#51149 = EDGE_CURVE ( 'NONE', #33316, #12604, #86124, .T. ) ;
#51148 = DIRECTION ( 'NONE',  ( -1.000000000000000000, 2.464095846557964090E-17, -0.000000000000000000 ) ) ;
#51150 =( REPRESENTATION_RELATIONSHIP ('NONE','NONE', #96270, #91803 ) REPRESENTATION_RELATIONSHIP_WITH_TRANSFORMATION ( #78954 )SHAPE_REPRESENTATION_RELATIONSHIP( ) );
#51151 = CARTESIAN_POINT ( 'NONE',  ( -63.52287095715006160, -23.47596703998600631, 11.44779298504228926 ) ) ;
#51153 = ORIENTED_EDGE ( 'NONE', *, *, #74616, .F. ) ;
#51152 = ADVANCED_FACE ( 'NONE', ( #62302 ), #48075, .T. ) ;
#51154 = CARTESIAN_POINT ( 'NONE',  ( 5.872047395031165351, -6.376774720514415407, 20.29192741308114734 ) ) ;
#51155 = EDGE_CURVE ( 'NONE', #53334, #80380, #70912, .T. ) ;
#51156 = CARTESIAN_POINT ( 'NONE',  ( -14.90462150274475306, 17.49973755783957685, 11.49999999999999645 ) ) ;
#51157 = CARTESIAN_POINT ( 'NONE',  ( -22.19569011343799048, 5.130922947863589378, 11.49999999999998934 ) ) ;
#51158 = CARTESIAN_POINT ( 'NONE',  ( -70.35039385224574460, -25.30458797330573972, 4.853613872476585378 ) ) ;
#51159 = EDGE_CURVE ( 'NONE', #89315, #78100, #93226, .T. ) ;
#51160 = CARTESIAN_POINT ( 'NONE',  ( -93.62287095715005592, -23.47593901973091235, -1.443836447539002865 ) ) ;
#51161 = DIRECTION ( 'NONE',  ( 1.000000000000000000, -7.960204194457801640E-17, 0.000000000000000000 ) ) ;
#51162 = CARTESIAN_POINT ( 'NONE',  ( -50.55620429048339304, -25.00158670708909270, 2.256160236439166855 ) ) ;
#51163 = EDGE_CURVE ( 'NONE', #89486, #99675, #54687, .T. ) ;
#51164 = CARTESIAN_POINT ( 'NONE',  ( -110.5132613601996070, -24.63355581998384380, 0.9682620441943931011 ) ) ;
#51165 = CARTESIAN_POINT ( 'NONE',  ( 17.35060923807083810, -13.37414737355047656, 11.49999999999998934 ) ) ;
#51166 = CARTESIAN_POINT ( 'NONE',  ( -59.62287095715004881, -24.64965695001468404, 8.947790433994185832 ) ) ;
#51167 = VECTOR ( 'NONE', #72036, 1000.000000000000227 ) ;
#51168 = DIRECTION ( 'NONE',  ( -3.773278334453079618E-23, 0.9999999999976377785, 2.173523156925979552E-06 ) ) ;
#51169 = DIRECTION ( 'NONE',  ( -0.8264557562326038109, 6.454799914155187856E-16, -0.5630016722799275897 ) ) ;
#51170 = DIRECTION ( 'NONE',  ( 5.328431011793917330E-15, 0.000000000000000000, 1.000000000000000000 ) ) ;
#51171 = VERTEX_POINT ( 'NONE', #8998 ) ;
#51172 = CIRCLE ( 'NONE', #85206, 1.249999999999997558 ) ;
#51173 = CARTESIAN_POINT ( 'NONE',  ( 1.124825640313904973, 20.40429917142216354, -1.500000000000002220 ) ) ;
#51174 = EDGE_LOOP ( 'NONE', ( #58205, #64185, #94069, #29016, #48778 ) ) ;
#51175 = VECTOR ( 'NONE', #52242, 1000.000000000000114 ) ;
#51176 = EDGE_LOOP ( 'NONE', ( #59918, #97243, #72844, #45718 ) ) ;
#51177 = ORIENTED_EDGE ( 'NONE', *, *, #40417, .T. ) ;
#51179 = EDGE_CURVE ( 'NONE', #1598, #7141, #16106, .T. ) ;
#51178 = ORIENTED_EDGE ( 'NONE', *, *, #7281, .F. ) ;
#51180 = CARTESIAN_POINT ( 'NONE',  ( 8.428894486204411507, 21.44871590506140890, -1.500000000000002220 ) ) ;
#51181 = CARTESIAN_POINT ( 'NONE',  ( 15.08554537508440774, -5.152774720514413431, -26.79085230644761495 ) ) ;
#51182 = CARTESIAN_POINT ( 'NONE',  ( -13.58233929615340152, 14.99024694321910900, -1.500000000000002220 ) ) ;
#51183 = AXIS2_PLACEMENT_3D ( 'NONE', #54480, #13528, #73954 ) ;
#51184 = ORIENTED_EDGE ( 'NONE', *, *, #13101, .T. ) ;
#51185 = CARTESIAN_POINT ( 'NONE',  ( -97.62287095715002749, -24.51283580621364067, 0.6167428607019886933 ) ) ;
#51186 = LINE ( 'NONE', #3518, #66039 ) ;
#51188 = EDGE_CURVE ( 'NONE', #29733, #65705, #16600, .T. ) ;
#51187 = AXIS2_PLACEMENT_3D ( 'NONE', #38541, #16199, #93830 ) ;
#51189 = CARTESIAN_POINT ( 'NONE',  ( -95.50514233772729256, -24.73486907724918282, 1.287355809206966128 ) ) ;
#51190 = CARTESIAN_POINT ( 'NONE',  ( -99.62355594549717352, -24.66019654487200086, 8.947790411086115725 ) ) ;
#51192 = ORIENTED_EDGE ( 'NONE', *, *, #67886, .F. ) ;
#51191 = CARTESIAN_POINT ( 'NONE',  ( 4.555389213293416617, -20.86945110937667280, 11.49999999999999645 ) ) ;
#51193 = CARTESIAN_POINT ( 'NONE',  ( 6.826756808399247589, -5.876774720514423400, 21.36722843294932161 ) ) ;
#51194 = VERTEX_POINT ( 'NONE', #8504 ) ;
#51195 = CARTESIAN_POINT ( 'NONE',  ( 18.30470771955606679, 12.64531542519679697, -1.500000000000002220 ) ) ;
#51196 = CARTESIAN_POINT ( 'NONE',  ( -6.067718162532647064, 19.77315050736717694, -1.500000000000002220 ) ) ;
#51197 = EDGE_LOOP ( 'NONE', ( #70031, #81041, #62892, #56052, #31066, #72434, #83010, #95801 ) ) ;
#51198 = CARTESIAN_POINT ( 'NONE',  ( 2.905472630834636139, -5.876774720514415407, 19.87563926270137671 ) ) ;
#51199 = ORIENTED_EDGE ( 'NONE', *, *, #59342, .F. ) ;
#51200 = CARTESIAN_POINT ( 'NONE',  ( -81.52287095715006160, -24.65952944569304606, 1.056160979905698794 ) ) ;
#51201 = VERTEX_POINT ( 'NONE', #79003 ) ;
#51202 = B_SPLINE_CURVE_WITH_KNOTS ( 'NONE', 3,
 ( #9464, #47038, #8467, #78964 ),
 .UNSPECIFIED., .F., .F.,
 ( 4, 4 ),
 ( 1.387778780781445676E-17, 0.0001000000000000028779 ),
 .UNSPECIFIED. ) ;
#51203 = CARTESIAN_POINT ( 'NONE',  ( -2.368302597431856782, 20.80102113048726409, -1.500000000000002220 ) ) ;
#51205 = EDGE_CURVE ( 'NONE', #47480, #59988, #32843, .T. ) ;
#51204 = CARTESIAN_POINT ( 'NONE',  ( 6.492371748702247203, -20.92784845389783399, 11.49999999999999645 ) ) ;
#51206 = CARTESIAN_POINT ( 'NONE',  ( -89.58585360431281686, -24.51419770103157703, 9.386484678747175181 ) ) ;
#51207 = CARTESIAN_POINT ( 'NONE',  ( -16.74547196562220464, 15.07928529822544661, 11.49999999999998934 ) ) ;
#51208 = CARTESIAN_POINT ( 'NONE',  ( 20.71091302404612833, 3.140364381853995912, 11.49999999999998934 ) ) ;
#51209 = CARTESIAN_POINT ( 'NONE',  ( -92.55472525529691552, -23.96169478059712787, 10.65365249895717525 ) ) ;
#51210 = CARTESIAN_POINT ( 'NONE',  ( -106.5228709571500758, -23.47596703998600631, 11.44779298504228038 ) ) ;
#51211 = CARTESIAN_POINT ( 'NONE',  ( -119.5211651280569924, -23.73791477778912551, 11.05961554403169878 ) ) ;
#51212 = DIRECTION ( 'NONE',  ( 0.000000000000000000, 0.000000000000000000, 1.000000000000000000 ) ) ;
#51213 = ORIENTED_EDGE ( 'NONE', *, *, #51359, .T. ) ;
#51214 = ORIENTED_EDGE ( 'NONE', *, *, #14916, .F. ) ;
#51215 = ORIENTED_EDGE ( 'NONE', *, *, #17363, .F. ) ;
#51216 = DIRECTION ( 'NONE',  ( 3.773278334444167608E-23, -1.000000000000000000, 0.000000000000000000 ) ) ;
#51217 = CARTESIAN_POINT ( 'NONE',  ( -20.40864349294084334, -6.676163967499375573, -1.500000000000002220 ) ) ;
#51218 = ADVANCED_FACE ( 'NONE', ( #94732 ), #62814, .F. ) ;
#51219 = DIRECTION ( 'NONE',  ( -1.000000000000000000, -3.773278334444166432E-23, -8.201307841325785021E-29 ) ) ;
#51220 = EDGE_LOOP ( 'NONE', ( #7175, #96514, #28714, #93768 ) ) ;
#51221 = CARTESIAN_POINT ( 'NONE',  ( -14.90395405082875335, 14.90835605916499418, -1.500000000000002220 ) ) ;
#51222 = DIRECTION ( 'NONE',  ( 0.000000000000000000, 0.000000000000000000, -1.000000000000000000 ) ) ;
#51223 = CARTESIAN_POINT ( 'NONE',  ( 3.797776442307698286, -6.376774720514427841, 21.83974358974358410 ) ) ;
#51224 = CARTESIAN_POINT ( 'NONE',  ( -50.55077666165203709, -24.15602025860895097, 10.28564288303536856 ) ) ;
#51225 = CARTESIAN_POINT ( 'NONE',  ( 11.80640562518893866, 3.316774720514426011, -27.06722565682295567 ) ) ;
#51226 = FACE_OUTER_BOUND ( 'NONE', #53815, .T. ) ;
#51227 = CARTESIAN_POINT ( 'NONE',  ( 17.94654606563480215, 12.89224558282342947, -1.500000000000002220 ) ) ;
#51228 = CARTESIAN_POINT ( 'NONE',  ( 9.940598223437577374, -5.876774720514426953, 17.91871304725684766 ) ) ;
#51229 = EDGE_CURVE ( 'NONE', #60724, #13389, #87633, .T. ) ;
#51230 = CARTESIAN_POINT ( 'NONE',  ( -44.62287095715004881, -24.65952944569303895, 1.056160979905693686 ) ) ;
#51231 = CARTESIAN_POINT ( 'NONE',  ( -94.52287095715006160, -24.65952944569304961, 1.056160979905700570 ) ) ;
#51232 = VECTOR ( 'NONE', #83691, 1000.000000000000114 ) ;
#51233 = CARTESIAN_POINT ( 'NONE',  ( -81.88534077628074215, -29.50249666744127808, 6.293933732382250845 ) ) ;
#51234 = CARTESIAN_POINT ( 'NONE',  ( 13.34776491790984210, -16.67230741956907991, 11.49999999999998934 ) ) ;
#51235 = CARTESIAN_POINT ( 'NONE',  ( -113.5562042904834072, -23.48786465467241769, 11.44779295918254292 ) ) ;
#51236 = DIRECTION ( 'NONE',  ( -1.000000000000000000, 1.232047923278981953E-16, 0.000000000000000000 ) ) ;
#51237 = PLANE ( 'NONE',  #81075 ) ;
#51238 = FACE_OUTER_BOUND ( 'NONE', #32061, .T. ) ;
#51239 = CC_DESIGN_DATE_AND_TIME_ASSIGNMENT ( #35911, #8456, ( #2120 ) ) ;
#51240 = CARTESIAN_POINT ( 'NONE',  ( -18.78231125015805958, 12.62931641965373153, -1.500000000000002220 ) ) ;
#51241 = AXIS2_PLACEMENT_3D ( 'NONE', #46919, #54533, #33189 ) ;
#51242 = ORIENTED_EDGE ( 'NONE', *, *, #21644, .T. ) ;
#51243 = CIRCLE ( 'NONE', #10752, 252.4458649670781085 ) ;
#51244 = DIRECTION ( 'NONE',  ( -3.773278334453080206E-23, 0.9999999999976377785, 2.173523156925979975E-06 ) ) ;
#51245 = CARTESIAN_POINT ( 'NONE',  ( -79.52213164415213953, -23.48783264082476308, -1.443836473390096575 ) ) ;
#51246 = CARTESIAN_POINT ( 'NONE',  ( -19.57314199983870751, -2.777824058246878280, 11.49999999999999645 ) ) ;
#51247 = CARTESIAN_POINT ( 'NONE',  ( -4.968349358974361252, -6.376774720514411854, 19.46153846153847056 ) ) ;
#51248 = VECTOR ( 'NONE', #7055, 1000.000000000000000 ) ;
#51249 = CARTESIAN_POINT ( 'NONE',  ( -67.53678271749727458, -24.65952944569304606, 1.056160979905700570 ) ) ;
#51250 = B_SPLINE_CURVE_WITH_KNOTS ( 'NONE', 3,
 ( #6593, #53782, #68498, #92821 ),
 .UNSPECIFIED., .F., .F.,
 ( 4, 4 ),
 ( 0.000000000000000000, 1.000000000000000000 ),
 .UNSPECIFIED. ) ;
#51251 = ORIENTED_EDGE ( 'NONE', *, *, #73199, .T. ) ;
#51252 = AXIS2_PLACEMENT_3D ( 'NONE', #6179, #21387, #91910 ) ;
#51253 = CARTESIAN_POINT ( 'NONE',  ( -54.52287095715006870, -29.50248528299804818, 1.056150453629033370 ) ) ;
#51254 = CARTESIAN_POINT ( 'NONE',  ( -29.31644179857717347, -25.26026486303936025, 2.549173870068830006 ) ) ;
#51255 = LINE ( 'NONE', #34536, #82058 ) ;
#51256 = CARTESIAN_POINT ( 'NONE',  ( -16.79864850723062020, -13.61054813162024679, -1.500000000000002220 ) ) ;
#51257 = CARTESIAN_POINT ( 'NONE',  ( 31.88667425545054002, -1.477225279485574028, -9.651215965565025812 ) ) ;
#51259 = CARTESIAN_POINT ( 'NONE',  ( -11.15089393765527959, -15.82809448842462885, -1.500000000000002220 ) ) ;
#51258 = AXIS2_PLACEMENT_3D ( 'NONE', #35924, #98306, #88722 ) ;
#51260 = B_SPLINE_CURVE_WITH_KNOTS ( 'NONE', 3,
 ( #58441, #75139, #5630, #51821, #81761, #42227 ),
 .UNSPECIFIED., .F., .F.,
 ( 4, 2, 4 ),
 ( 0.000000000000000000, 0.001380764517854760412, 0.002761529035709520824 ),
 .UNSPECIFIED. ) ;
#51261 = CARTESIAN_POINT ( 'NONE',  ( -10.23311166579590825, -4.222446552888387217, 29.28685113854110966 ) ) ;
#51262 = CARTESIAN_POINT ( 'NONE',  ( 282.9764569301858046, -5.356774720514427379, 20.79159422840526616 ) ) ;
#51263 = CARTESIAN_POINT ( 'NONE',  ( -2.602694502683683631, -19.63732897141692391, 11.49999999999998934 ) ) ;
#51264 = VERTEX_POINT ( 'NONE', #42474 ) ;
#51265 = CARTESIAN_POINT ( 'NONE',  ( -3.898967980886277829, 19.90457959416237088, 11.49999999999999645 ) ) ;
#51266 = CARTESIAN_POINT ( 'NONE',  ( 6.875727764383598561, 6.376774720514445605, -25.57138887952572404 ) ) ;
#51267 = CARTESIAN_POINT ( 'NONE',  ( 6.044119082205957838, -6.376774720514424288, 21.40268112089023589 ) ) ;
#51268 = VERTEX_POINT ( 'NONE', #4893 ) ;
#51269 = CARTESIAN_POINT ( 'NONE',  ( -110.5228709571500616, -24.99132157543167310, 2.256160258750667502 ) ) ;
#51270 = CARTESIAN_POINT ( 'NONE',  ( 15.15958133180904355, -5.152774720514426754, -26.63299148310929709 ) ) ;
#51271 = CYLINDRICAL_SURFACE ( 'NONE', #80804, 2.499999999999995115 ) ;
#51272 = DIRECTION ( 'NONE',  ( 0.000000000000000000, 0.000000000000000000, -1.000000000000000000 ) ) ;
#51273 = CARTESIAN_POINT ( 'NONE',  ( 18.22465585706453339, 0.000000000000000000, -2.153101996372891236 ) ) ;
#51274 = CARTESIAN_POINT ( 'NONE',  ( -13.81204400269958654, 14.50282280199826701, -1.500000000000002220 ) ) ;
#51275 = CARTESIAN_POINT ( 'NONE',  ( 32.45853543194704116, 0.3587747205144265483, 9.169203677920338080 ) ) ;
#51276 = ORIENTED_EDGE ( 'NONE', *, *, #9825, .F. ) ;
#51277 = VECTOR ( 'NONE', #30905, 1000.000000000000000 ) ;
#51278 = DIRECTION ( 'NONE',  ( 7.150924204855701834E-40, 2.173523156925979975E-06, -0.9999999999976378895 ) ) ;
#51279 = ADVANCED_FACE ( 'NONE', ( #18604 ), #28289, .T. ) ;
#51280 = CARTESIAN_POINT ( 'NONE',  ( -129.5228709571500758, -24.64898659630529920, 1.056161002820834804 ) ) ;
#51281 = CARTESIAN_POINT ( 'NONE',  ( -3.106028565906091998, -5.876774720514426953, 3.106028565906120864 ) ) ;
#51282 = EDGE_CURVE ( 'NONE', #39531, #72799, #81522, .T. ) ;
#51283 = CARTESIAN_POINT ( 'NONE',  ( -113.5228709571500616, -24.64898659630368627, 1.056161002820831474 ) ) ;
#51284 = DIRECTION ( 'NONE',  ( -3.773278334453079618E-23, 0.9999999999976377785, 2.173523156925979975E-06 ) ) ;
#51285 = B_SPLINE_CURVE_WITH_KNOTS ( 'NONE', 3,
 ( #37975, #78896, #61828, #68429, #1796, #76518, #17512, #7024, #40355, #60833, #48479, #91751 ),
 .UNSPECIFIED., .F., .F.,
 ( 4, 2, 2, 2, 2, 4 ),
 ( 6.686686736723900881E-09, 0.0004767310751705819308, 0.0009534554636544272143, 0.001430179852138272444, 0.001668542046380201618, 0.001906904240622130792 ),
 .UNSPECIFIED. ) ;
#51286 = CARTESIAN_POINT ( 'NONE',  ( -71.52287095715010423, -24.66019654487200086, 8.947790411086115725 ) ) ;
#51287 = ORIENTED_EDGE ( 'NONE', *, *, #25140, .F. ) ;
#51288 = CARTESIAN_POINT ( 'NONE',  ( 9.809556900635294951, 17.81656380412256269, 11.49999999999998934 ) ) ;
#51289 = ORIENTED_EDGE ( 'NONE', *, *, #71711, .T. ) ;
#51290 = EDGE_CURVE ( 'NONE', #88013, #54552, #41972, .T. ) ;
#51291 = CARTESIAN_POINT ( 'NONE',  ( -3.094460115123966570, -22.75893099265358188, 11.49999999999998934 ) ) ;
#51293 = CARTESIAN_POINT ( 'NONE',  ( -32.57492585626526704, -24.65952944569304606, 1.056160979905696351 ) ) ;
#51292 = B_SPLINE_CURVE_WITH_KNOTS ( 'NONE', 3,
 ( #95921, #94918, #33523, #16791 ),
 .UNSPECIFIED., .F., .F.,
 ( 4, 4 ),
 ( 0.09985723008135170831, 0.1088636613534670478 ),
 .UNSPECIFIED. ) ;
#51294 = ORIENTED_EDGE ( 'NONE', *, *, #12249, .F. ) ;
#51295 = DIRECTION ( 'NONE',  ( 0.000000000000000000, -2.173523156925980399E-06, 0.9999999999976378895 ) ) ;
#51296 = AXIS2_PLACEMENT_3D ( 'NONE', #41157, #48775, #49280 ) ;
#51297 = CARTESIAN_POINT ( 'NONE',  ( -77.62287095715005592, -24.64965695001468404, 8.947790433994182280 ) ) ;
#51298 = LINE ( 'NONE', #82238, #54501 ) ;
#51300 = VERTEX_POINT ( 'NONE', #34347 ) ;
#51299 = CARTESIAN_POINT ( 'NONE',  ( -13.45780860896912934, -16.40347334334247265, 11.49999999999999645 ) ) ;
#51301 = VERTEX_POINT ( 'NONE', #11005 ) ;
#51302 = CARTESIAN_POINT ( 'NONE',  ( -18.12599551585701008, -12.76988789260850332, -1.500000000000002220 ) ) ;
#51303 = CARTESIAN_POINT ( 'NONE',  ( -3.210669876418242197, 20.33209092710186638, 11.49999999999998934 ) ) ;
#51304 = CIRCLE ( 'NONE', #2717, 1.249999999999996003 ) ;
#51305 = EDGE_LOOP ( 'NONE', ( #40065, #51825, #84510, #1919 ) ) ;
#51306 = ORIENTED_EDGE ( 'NONE', *, *, #69404, .F. ) ;
#51307 = CARTESIAN_POINT ( 'NONE',  ( -94.52287095715006160, -29.50248528299804818, 1.056150453629040253 ) ) ;
#51308 = PLANE ( 'NONE',  #61596 ) ;
#51309 = ORIENTED_EDGE ( 'NONE', *, *, #88162, .F. ) ;
#51310 = VECTOR ( 'NONE', #4276, 1000.000000000000114 ) ;
#51311 = ORIENTED_EDGE ( 'NONE', *, *, #78969, .F. ) ;
#51312 = CIRCLE ( 'NONE', #64311, 1.500000000000000666 ) ;
#51313 = VERTEX_POINT ( 'NONE', #72416 ) ;
#51314 = CARTESIAN_POINT ( 'NONE',  ( 0.000000000000000000, 0.000000000000000000, 0.000000000000000000 ) ) ;
#51315 = CARTESIAN_POINT ( 'NONE',  ( -28.62972572368664714, -24.36142566672730325, 9.386484685950513551 ) ) ;
#51316 = PLANE ( 'NONE',  #14705 ) ;
#51317 = CARTESIAN_POINT ( 'NONE',  ( -0.3852054317258338245, -20.75737367715079174, -1.500000000000002220 ) ) ;
#51318 = CARTESIAN_POINT ( 'NONE',  ( 18.41774212405765709, -11.57998961627671441, 11.49999999999999645 ) ) ;
#51319 = ORIENTED_EDGE ( 'NONE', *, *, #22163, .F. ) ;
#51320 = CARTESIAN_POINT ( 'NONE',  ( -40.45231480346743069, -25.27806139640134120, 5.081397595443370996 ) ) ;
#51321 = DIRECTION ( 'NONE',  ( -3.773278334453080206E-23, 0.9999999999976377785, 2.173523156925979975E-06 ) ) ;
#51322 = CARTESIAN_POINT ( 'NONE',  ( -115.5516351120022591, -24.73486907724918282, 1.287355809206964352 ) ) ;
#51323 = CARTESIAN_POINT ( 'NONE',  ( -17.72129891523481149, -13.73837202384828515, -1.500000000000002220 ) ) ;
#51324 = DIRECTION ( 'NONE',  ( -3.773278334453080206E-23, 0.9999999999976377785, 2.173523156925979975E-06 ) ) ;
#51325 = CARTESIAN_POINT ( 'NONE',  ( 23.07151214508650128, 3.625915217019311583E-15, 0.000000000000000000 ) ) ;
#51327 = EDGE_CURVE ( 'NONE', #57623, #75580, #89851, .T. ) ;
#51326 = ORIENTED_EDGE ( 'NONE', *, *, #5495, .T. ) ;
#51328 = CARTESIAN_POINT ( 'NONE',  ( -0.3059464777392852941, -8.530684776139525027, -9.000000000000000000 ) ) ;
#51329 = CARTESIAN_POINT ( 'NONE',  ( -86.52287095715006160, -23.48783264083431277, -1.443836473375255336 ) ) ;
#51330 = ORIENTED_EDGE ( 'NONE', *, *, #13785, .T. ) ;
#51331 = B_SPLINE_CURVE_WITH_KNOTS ( 'NONE', 3,
 ( #86988, #72782, #94098, #55558 ),
 .UNSPECIFIED., .F., .F.,
 ( 4, 4 ),
 ( 0.000000000000000000, 9.999999999997510880E-05 ),
 .UNSPECIFIED. ) ;
#51332 = VERTEX_POINT ( 'NONE', #26229 ) ;
#51333 = CARTESIAN_POINT ( 'NONE',  ( 25.61870917940689196, -0.3587747205144265483, 28.79814474876424768 ) ) ;
#51334 = ADVANCED_FACE ( 'NONE', ( #49083 ), #20107, .F. ) ;
#51335 = ORIENTED_EDGE ( 'NONE', *, *, #65704, .T. ) ;
#51336 = CARTESIAN_POINT ( 'NONE',  ( -20.61954105445765251, -5.431428859615135885, -1.500000000000002220 ) ) ;
#51337 = B_SPLINE_CURVE_WITH_KNOTS ( 'NONE', 3,
 ( #71069, #77653, #9665, #70055 ),
 .UNSPECIFIED., .F., .F.,
 ( 4, 4 ),
 ( 0.000000000000000000, 9.999999999996123101E-05 ),
 .UNSPECIFIED. ) ;
#51338 = ORIENTED_EDGE ( 'NONE', *, *, #94608, .T. ) ;
#51339 = CYLINDRICAL_SURFACE ( 'NONE', #36538, 24.00000000000000000 ) ;
#51340 = CARTESIAN_POINT ( 'NONE',  ( 8.107222467604051630, 20.28165043084963060, 11.49999999999998934 ) ) ;
#51341 = CARTESIAN_POINT ( 'NONE',  ( -3.826923076923078426, -6.376774720514408301, 19.19230769230769695 ) ) ;
#51342 = CARTESIAN_POINT ( 'NONE',  ( 4.020035926878589905, 22.33396232419688587, 11.49999999999998934 ) ) ;
#51343 = CARTESIAN_POINT ( 'NONE',  ( -112.5895376238167245, -24.65952944569305316, 1.056160979905713670 ) ) ;
#51344 = CARTESIAN_POINT ( 'NONE',  ( -49.52287095715004028, -23.73934037231756022, 11.05740245334329153 ) ) ;
#51345 = CARTESIAN_POINT ( 'NONE',  ( 19.17116566557315949, -10.70166234769870961, -1.500000000000002220 ) ) ;
#51346 = DIRECTION ( 'NONE',  ( 0.000000000000000000, -0.9999999999976377785, -2.173523156925979975E-06 ) ) ;
#51347 = VERTEX_POINT ( 'NONE', #58189 ) ;
#51348 = CARTESIAN_POINT ( 'NONE',  ( 29.70917971445138051, -6.219445159570049064, 27.14760184111773356 ) ) ;
#51349 = CARTESIAN_POINT ( 'NONE',  ( -84.52287095715006160, -29.50250243563736774, 8.947779886222141599 ) ) ;
#51350 = VECTOR ( 'NONE', #80516, 1000.000000000000000 ) ;
#51351 = EDGE_LOOP ( 'NONE', ( #77587, #79306, #34967, #68654, #40460, #53071, #44821, #11575, #20305, #27278, #78489, #36997, #8512, #17264, #88504, #17088, #13729, #8465, #22625, #38810, #95082, #1931, #79262, #29647, #81531, #84377, #71651, #21972, #60101, #62389, #65302, #48465, #76140, #38484, #6305, #77231, #94603, #17104, #49511, #72415, #34215, #53736, #81343, #4012, #93531, #11029, #10873, #42856, #42118, #71820, #3869, #31675, #86209, #50982, #71535, #69745, #43980, #3815, #9919, #29087, #39720, #1000, #82347, #95984, #20997, #58950, #7034, #83903, #73603, #2434, #1661, #2324, #54322, #60198, #32215, #7485, #90233, #47094, #33174, #24963, #88435, #14732, #63720, #68966, #64391, #80048, #16802, #49092, #10573, #53846, #46301, #73806, #98452, #54586, #66156, #40868, #94996, #81552, #97253, #40734, #19819 ) ) ;
#51352 = DIRECTION ( 'NONE',  ( -3.773278334453080206E-23, 0.9999999999976377785, 2.173523156925979975E-06 ) ) ;
#51353 = CARTESIAN_POINT ( 'NONE',  ( 5.097264368846952998, 6.475225279485573360, -27.56135813788808164 ) ) ;
#51354 = AXIS2_PLACEMENT_3D ( 'NONE', #60720, #70820, #29752 ) ;
#51355 = CARTESIAN_POINT ( 'NONE',  ( -0.1490770655183800975, -21.12008023607309681, -1.443836447538997314 ) ) ;
#51356 = CARTESIAN_POINT ( 'NONE',  ( -13.59518820711925358, -16.35513075224449864, 11.49999999999998934 ) ) ;
#51357 = CARTESIAN_POINT ( 'NONE',  ( -112.5905343604989923, -24.15543982623908192, -0.2315651400026420559 ) ) ;
#51358 = CARTESIAN_POINT ( 'NONE',  ( -26.21213932664330670, -24.75186287970886667, 3.737064058008186418 ) ) ;
#51359 = EDGE_CURVE ( 'NONE', #42617, #99563, #83323, .T. ) ;
#51360 = DIRECTION ( 'NONE',  ( -0.2007054744626894649, 0.000000000000000000, 0.9796516281417116945 ) ) ;
#51361 = PLANE ( 'NONE',  #57336 ) ;
#51362 = B_SPLINE_SURFACE_WITH_KNOTS ( 'NONE', 3, 3, ( 
 ( #88698, #65880, #19166, #27786 ),
 ( #58739, #95798, #50135, #43022 ),
 ( #27294, #89688, #50628, #18669 ),
 ( #82071, #12557, #80078, #73966 ),
 ( #97790, #41523, #26292, #88198 ),
 ( #33903, #81582, #4464, #77912 ),
 ( #23196, #61789, #76980, #54181 ) ),
 .UNSPECIFIED., .F., .F., .F.,
 ( 4, 3, 4 ),
 ( 4, 4 ),
 ( 0.0004766839783824310508, 0.1029713700210899002, 0.2054660560637973643 ),
 ( 0.2595600248839645130, 0.2606925099585566397 ),
 .UNSPECIFIED. ) ;
#51363 = CARTESIAN_POINT ( 'NONE',  ( -117.5188394651187167, -24.15620529776629510, 10.23563542870659582 ) ) ;
#51364 = VERTEX_POINT ( 'NONE', #2911 ) ;
#51365 = CARTESIAN_POINT ( 'NONE',  ( 19.09806219120973125, -4.162641619376711510, 11.49999999999999645 ) ) ;
#51366 = CARTESIAN_POINT ( 'NONE',  ( -66.62287095715002749, -24.35013146730203459, 9.818937971375113705 ) ) ;
#51367 = CARTESIAN_POINT ( 'NONE',  ( -29.81175120719462157, -25.24633111994858581, 4.942810988825437235 ) ) ;
#51368 = ORIENTED_EDGE ( 'NONE', *, *, #58290, .F. ) ;
#51369 = CARTESIAN_POINT ( 'NONE',  ( 4.332134589405623792, -5.876774720514426953, 21.69242924468134959 ) ) ;
#51370 = EDGE_CURVE ( 'NONE', #17140, #30450, #76905, .T. ) ;
#51371 = CARTESIAN_POINT ( 'NONE',  ( -101.5228709571500758, -24.64965694238407323, 8.947790433994194714 ) ) ;
#51372 = CIRCLE ( 'NONE', #62762, 2.249999999999998668 ) ;
#51373 = CARTESIAN_POINT ( 'NONE',  ( -27.61217026053484958, -24.64375301970309806, 8.250468979048056539 ) ) ;
#51374 = CARTESIAN_POINT ( 'NONE',  ( 6.499999999999992895, 0.9999999999999993339, 1.084202172485504187E-16 ) ) ;
#51375 = CARTESIAN_POINT ( 'NONE',  ( 16.13486940644654766, 11.28601765141728741, 11.49999999999998934 ) ) ;
#51376 = ORIENTED_EDGE ( 'NONE', *, *, #57239, .F. ) ;
#51377 = DIRECTION ( 'NONE',  ( 0.000000000000000000, 0.000000000000000000, -1.000000000000000000 ) ) ;
#51378 = CARTESIAN_POINT ( 'NONE',  ( -72.62287095715005592, -29.50247984919015209, -1.443849546365055359 ) ) ;
#51379 = AXIS2_PLACEMENT_3D ( 'NONE', #20813, #6098, #45672 ) ;
#51380 = COORDINATED_UNIVERSAL_TIME_OFFSET ( 0, 0, .AHEAD. ) ;
#51381 = ORIENTED_EDGE ( 'NONE', *, *, #55274, .F. ) ;
#51382 = CARTESIAN_POINT ( 'NONE',  ( 8.456965425111590662, -0.2003331576018148041, 3.712238059855193839 ) ) ;
#51383 = CARTESIAN_POINT ( 'NONE',  ( -45.62287095715005592, -24.92604778743018556, 8.074972756849359001 ) ) ;
#51384 = CARTESIAN_POINT ( 'NONE',  ( -55.56003731193040807, -23.85016227208578954, -0.8807180028928371929 ) ) ;
#51385 = CARTESIAN_POINT ( 'NONE',  ( -63.22287095715004313, -23.47593901973090524, -1.443836447538997536 ) ) ;
#51386 = CARTESIAN_POINT ( 'NONE',  ( -31.62287095715005236, -23.95044443724991368, 10.65354141964649948 ) ) ;
#51387 = AXIS2_PLACEMENT_3D ( 'NONE', #17513, #62707, #63718 ) ;
#51388 = AXIS2_PLACEMENT_3D ( 'NONE', #84396, #99601, #55459 ) ;
#51389 = DIRECTION ( 'NONE',  ( 0.000000000000000000, -0.9999999999976377785, -2.173523156925979975E-06 ) ) ;
#51390 = ADVANCED_FACE ( 'NONE', ( #65814 ), #88137, .F. ) ;
#51391 = CARTESIAN_POINT ( 'NONE',  ( -107.6280297884409265, -24.15543982623907837, -0.2315651400026443874 ) ) ;
#51393 = EDGE_CURVE ( 'NONE', #88212, #81441, #85350, .T. ) ;
#51392 = CARTESIAN_POINT ( 'NONE',  ( 19.82558669001425500, -2.195561414069463702, 11.49999999999998934 ) ) ;
#51394 = DIRECTION ( 'NONE',  ( -3.773278334453079618E-23, 0.9999999999976377785, 2.173523156925979975E-06 ) ) ;
#51395 = CARTESIAN_POINT ( 'NONE',  ( -0.03888317010184255684, -22.54662680705505551, 8.463919116204994708 ) ) ;
#51396 = ORIENTED_EDGE ( 'NONE', *, *, #44976, .T. ) ;
#51397 = DIRECTION ( 'NONE',  ( -3.773278334453079618E-23, 0.9999999999976377785, 2.173523156925979975E-06 ) ) ;
#51398 = DIRECTION ( 'NONE',  ( 1.000000000000000000, 0.000000000000000000, 0.000000000000000000 ) ) ;
#51399 = PLANE ( 'NONE',  #71841 ) ;
#51400 = DIRECTION ( 'NONE',  ( -0.7071067811865516806, -0.7071067811865434649, 0.000000000000000000 ) ) ;
#51401 = FACE_OUTER_BOUND ( 'NONE', #73789, .T. ) ;
#51402 = ADVANCED_FACE ( 'NONE', ( #29718 ), #100209, .T. ) ;
#51403 = CARTESIAN_POINT ( 'NONE',  ( -2.070328576748420524, -6.376774720514410077, 19.46575348430201657 ) ) ;
#51404 = B_SPLINE_CURVE_WITH_KNOTS ( 'NONE', 3,
 ( #19637, #13516, #5418, #67329 ),
 .UNSPECIFIED., .F., .F.,
 ( 4, 4 ),
 ( 0.000000000000000000, 1.000000000000000000 ),
 .UNSPECIFIED. ) ;
#51405 = ORIENTED_EDGE ( 'NONE', *, *, #49017, .F. ) ;
#51406 = CARTESIAN_POINT ( 'NONE',  ( -97.52287095715007581, -23.47593901973090524, -1.443836447538996648 ) ) ;
#51407 = EDGE_CURVE ( 'NONE', #75293, #99976, #14982, .T. ) ;
#51408 = CARTESIAN_POINT ( 'NONE',  ( 6.274899854645557440, -5.876774720514428729, 21.83451738260096775 ) ) ;
#51409 = ORIENTED_EDGE ( 'NONE', *, *, #20418, .F. ) ;
#51410 = CARTESIAN_POINT ( 'NONE',  ( 3.706880958665978998, 19.89330832657401515, -1.500000000000002220 ) ) ;
#51411 = B_SPLINE_CURVE_WITH_KNOTS ( 'NONE', 3,
 ( #8285, #95024, #86908, #9786 ),
 .UNSPECIFIED., .F., .F.,
 ( 4, 4 ),
 ( 2.775557561562891351E-17, 8.203124999998923084E-05 ),
 .UNSPECIFIED. ) ;
#51412 = DIRECTION ( 'NONE',  ( -0.1478094111296165691, 0.9890158633619158257, 6.377659838150018832E-17 ) ) ;
#51413 = EDGE_CURVE ( 'NONE', #7766, #68548, #92545, .T. ) ;
#51414 = CARTESIAN_POINT ( 'NONE',  ( 15.03086228770605004, 5.128928118853486318, -26.95277610321158335 ) ) ;
#51415 = AXIS2_PLACEMENT_3D ( 'NONE', #47344, #1674, #47845 ) ;
#51416 = ADVANCED_FACE ( 'NONE', ( #28728 ), #76374, .F. ) ;
#51417 = CARTESIAN_POINT ( 'NONE',  ( -58.52287095715004739, -23.47593901973090169, -1.443836447538997092 ) ) ;
#51418 = ORIENTED_EDGE ( 'NONE', *, *, #62512, .F. ) ;
#51419 = CARTESIAN_POINT ( 'NONE',  ( -105.9228709571500673, -23.47596703998600631, 11.44779298504227860 ) ) ;
#51420 = FACE_OUTER_BOUND ( 'NONE', #64052, .T. ) ;
#51421 = CARTESIAN_POINT ( 'NONE',  ( 20.03642891561555928, 0.6179553080306146029, -1.500000000000002220 ) ) ;
#51422 = CARTESIAN_POINT ( 'NONE',  ( 19.54352652498339182, 7.673529024697476331, 11.49999999999999645 ) ) ;
#51423 = CIRCLE ( 'NONE', #7666, 1.700000000000008837 ) ;
#51424 = CARTESIAN_POINT ( 'NONE',  ( -28.94471403569382773, -25.05935760451456318, 6.779848816579228554 ) ) ;
#51425 = CARTESIAN_POINT ( 'NONE',  ( -111.6228709571500417, -24.50321055353806088, 9.387540953477531147 ) ) ;
#51426 = CARTESIAN_POINT ( 'NONE',  ( -21.42919730060085115, -5.301375089729956969, 11.49999999999998934 ) ) ;
#51427 = B_SPLINE_CURVE_WITH_KNOTS ( 'NONE', 3,
 ( #45543, #24185, #77461, #7961 ),
 .UNSPECIFIED., .F., .F.,
 ( 4, 4 ),
 ( 0.000000000000000000, 9.999999999998897304E-05 ),
 .UNSPECIFIED. ) ;
#51428 = CARTESIAN_POINT ( 'NONE',  ( -66.55620429048339304, -24.66019654487199020, 8.947790411086131712 ) ) ;
#51429 = CARTESIAN_POINT ( 'NONE',  ( -47.62287095715004881, -24.64898659630367916, 1.056161002820821038 ) ) ;
#51430 = CARTESIAN_POINT ( 'NONE',  ( -50.30027857337484676, -25.27344760046473482, 3.296100333510875391 ) ) ;
#51431 = ORIENTED_EDGE ( 'NONE', *, *, #55153, .T. ) ;
#51432 = LINE ( 'NONE', #21945, #5685 ) ;
#51433 = CARTESIAN_POINT ( 'NONE',  ( -31.56131489220916819, -23.73766607897669800, -1.055555164236445131 ) ) ;
#51434 = ORIENTED_EDGE ( 'NONE', *, *, #28038, .T. ) ;
#51435 = ORIENTED_EDGE ( 'NONE', *, *, #97339, .F. ) ;
#51436 = CARTESIAN_POINT ( 'NONE',  ( 16.26279755680690542, -1.684774720514426560, -27.67997040356620531 ) ) ;
#51437 = FACE_OUTER_BOUND ( 'NONE', #16117, .T. ) ;
#51438 = CARTESIAN_POINT ( 'NONE',  ( -76.55419634045316002, -23.96119346886880663, -0.6495511937832058047 ) ) ;
#51439 = CARTESIAN_POINT ( 'NONE',  ( -16.28974412851428255, -12.55652860423730388, -1.500000000000002220 ) ) ;
#51440 = CARTESIAN_POINT ( 'NONE',  ( -19.30636564405121902, 9.640216152154000184, 11.49999999999999645 ) ) ;
#51441 = ORIENTED_EDGE ( 'NONE', *, *, #6831, .F. ) ;
#51442 = CARTESIAN_POINT ( 'NONE',  ( -50.26609345566524922, -25.13378748658239559, 7.097951806649573037 ) ) ;
#51443 = CARTESIAN_POINT ( 'NONE',  ( -99.12672354517025042, -25.27198829872966712, 4.094481813589349706 ) ) ;
#51444 = PLANE ( 'NONE',  #22110 ) ;
#51445 = CARTESIAN_POINT ( 'NONE',  ( 4.697571063781373013, 21.84268702631108994, 11.49999999999998934 ) ) ;
#51446 = VECTOR ( 'NONE', #91788, 1000.000000000000114 ) ;
#51447 = CARTESIAN_POINT ( 'NONE',  ( -50.62287095715004170, -23.48783264082478084, -1.443836473390070596 ) ) ;
#51448 = CARTESIAN_POINT ( 'NONE',  ( -20.77875734969026311, 6.143225279485574397, 27.35402280011862430 ) ) ;
#51449 = ORIENTED_EDGE ( 'NONE', *, *, #11070, .T. ) ;
#51450 = DIRECTION ( 'NONE',  ( -0.1593164160933057683, 0.000000000000000000, 0.9872275723272647685 ) ) ;
#51451 = LINE ( 'NONE', #35229, #96093 ) ;
#51452 = CARTESIAN_POINT ( 'NONE',  ( 17.92008016455634589, 10.74458801173053324, 11.49999999999998934 ) ) ;
#51453 = ORIENTED_EDGE ( 'NONE', *, *, #29385, .T. ) ;
#51455 = ORIENTED_EDGE ( 'NONE', *, *, #91076, .T. ) ;
#51454 = FACE_OUTER_BOUND ( 'NONE', #35363, .T. ) ;
#51456 = CIRCLE ( 'NONE', #48202, 4.299999999999999822 ) ;
#51457 = ORIENTED_EDGE ( 'NONE', *, *, #90424, .T. ) ;
#51458 = EDGE_CURVE ( 'NONE', #32849, #33122, #80153, .T. ) ;
#51459 = CARTESIAN_POINT ( 'NONE',  ( -100.5576076336107434, -23.85049219812686161, 10.88485053497527133 ) ) ;
#51460 = CARTESIAN_POINT ( 'NONE',  ( -3.482456173223098528, 20.84670800329844198, -1.500000000000002220 ) ) ;
#51461 = ORIENTED_EDGE ( 'NONE', *, *, #79934, .F. ) ;
#51462 = DIRECTION ( 'NONE',  ( 0.000000000000000000, 0.000000000000000000, -1.000000000000000000 ) ) ;
#51463 = DIRECTION ( 'NONE',  ( 1.000000000000000000, 0.000000000000000000, 0.000000000000000000 ) ) ;
#51464 = CARTESIAN_POINT ( 'NONE',  ( -129.5895376238167387, -23.48786465467241769, 11.44779295918253581 ) ) ;
#51465 = VECTOR ( 'NONE', #69187, 1000.000000000000000 ) ;
#51466 = PLANE ( 'NONE',  #90704 ) ;
#51467 = CARTESIAN_POINT ( 'NONE',  ( 7.107139210497321002, -5.876774720514413630, 19.78447747620696617 ) ) ;
#51468 = CARTESIAN_POINT ( 'NONE',  ( -21.74948284930419717, -1.071797830193938372, -1.500000000000002220 ) ) ;
#51469 = CARTESIAN_POINT ( 'NONE',  ( -107.5228709571501042, -23.48783264083360578, -1.443836473376361118 ) ) ;
#51471 = VERTEX_POINT ( 'NONE', #30713 ) ;
#51470 = CARTESIAN_POINT ( 'NONE',  ( -7.140196579304709523, 21.16591527347414115, 11.49999999999999645 ) ) ;
#51472 = CARTESIAN_POINT ( 'NONE',  ( -57.52287095715005449, -23.48786465467241058, 11.44779295918254824 ) ) ;
#51473 = LINE ( 'NONE', #73802, #71916 ) ;
#51474 = CARTESIAN_POINT ( 'NONE',  ( -106.5228709571500900, -24.33927499327855060, 9.819080762295804732 ) ) ;
#51475 = ORIENTED_EDGE ( 'NONE', *, *, #37639, .T. ) ;
#51476 = ORIENTED_EDGE ( 'NONE', *, *, #67681, .T. ) ;
#51477 = ORIENTED_EDGE ( 'NONE', *, *, #40103, .T. ) ;
#51478 = PLANE ( 'NONE',  #70760 ) ;
#51479 = CARTESIAN_POINT ( 'NONE',  ( -86.58953762381669605, -23.47596703998600631, 11.44779298504227683 ) ) ;
#51480 = CARTESIAN_POINT ( 'NONE',  ( 30.59430046144282400, -4.508643932895013862, 26.46466010020539272 ) ) ;
#51481 = CARTESIAN_POINT ( 'NONE',  ( -43.62287095715004881, -24.64965695001467694, 8.947790433994187609 ) ) ;
#51482 = EDGE_CURVE ( 'NONE', #45115, #46021, #23518, .T. ) ;
#51483 = CARTESIAN_POINT ( 'NONE',  ( -87.52287095715006160, -24.33927499327855770, 9.819080762295810061 ) ) ;
#51484 = B_SPLINE_CURVE_WITH_KNOTS ( 'NONE', 3,
 ( #55001, #40269, #64131, #85940 ),
 .UNSPECIFIED., .F., .F.,
 ( 4, 4 ),
 ( 0.000000000000000000, 1.000000000000000000 ),
 .UNSPECIFIED. ) ;
#51485 = CARTESIAN_POINT ( 'NONE',  ( -36.52287095715009002, -24.66019654487199730, 8.947790411086124607 ) ) ;
#51486 = VERTEX_POINT ( 'NONE', #61683 ) ;
#51487 = CARTESIAN_POINT ( 'NONE',  ( 14.41255161864883583, -12.98630880007775268, 11.49999999999999645 ) ) ;
#51488 = LINE ( 'NONE', #52990, #37388 ) ;
#51489 = ORIENTED_EDGE ( 'NONE', *, *, #80045, .T. ) ;
#51490 = CARTESIAN_POINT ( 'NONE',  ( 3.202571139211427553, -6.376774720514406525, 18.81074098386681470 ) ) ;
#51491 = CARTESIAN_POINT ( 'NONE',  ( 2.710830299132254595, -5.876774720514410966, 19.05039662921485544 ) ) ;
#51492 = EDGE_CURVE ( 'NONE', #67443, #36561, #63648, .T. ) ;
#51493 = AXIS2_PLACEMENT_3D ( 'NONE', #89779, #90772, #66954 ) ;
#51494 = EDGE_CURVE ( 'NONE', #31671, #48067, #70281, .T. ) ;
#51495 = FACE_OUTER_BOUND ( 'NONE', #84125, .T. ) ;
#51496 = EDGE_CURVE ( 'NONE', #22449, #60562, #40329, .T. ) ;
#51497 = CARTESIAN_POINT ( 'NONE',  ( -36.52287095715006870, -23.96177878511308279, 10.65340807706330573 ) ) ;
#51498 = CARTESIAN_POINT ( 'NONE',  ( 10.47639735327893362, 16.54961352017854637, 11.49999999999998934 ) ) ;
#51499 = B_SPLINE_SURFACE_WITH_KNOTS ( 'NONE', 3, 1, ( 
 ( #47392, #45896 ),
 ( #30155, #61128 ),
 ( #76319, #77809 ),
 ( #78319, #86445 ),
 ( #23524, #8825 ),
 ( #39762, #70724 ),
 ( #31154, #92056 ),
 ( #54503, #7819 ),
 ( #6818, #92551 ),
 ( #77318, #85437 ),
 ( #1218, #23023 ),
 ( #32152, #38764 ),
 ( #63127, #15923 ),
 ( #94053, #22527 ),
 ( #24539, #55509 ),
 ( #53520, #46891 ),
 ( #84443, #76813 ),
 ( #38266, #69224 ),
 ( #8321, #100139 ) ),
 .UNSPECIFIED., .F., .F., .F.,
 ( 4, 1, 1, 1, 1, 1, 1, 1, 1, 1, 1, 1, 1, 1, 1, 1, 4 ),
 ( 2, 2 ),
 ( 0.000000000000000000, 0.06879079439061809575, 0.1351032894311278987, 0.1989786743106516376, 0.2619042997808557205, 0.3234949693679702309, 0.3851953779660500787, 0.4469692387407731005, 0.5097647767031340260, 0.5722505688473688013, 0.6334051756611546180, 0.6932511629217514848, 0.7525831627856720552, 0.8125792661534239070, 0.8732750849201905696, 0.9355499428950290186, 1.000000000000000000 ),
 ( 0.000000000000000000, 1.000000000000000000 ),
 .UNSPECIFIED. ) ;
#51500 = CARTESIAN_POINT ( 'NONE',  ( -66.62287095715005592, -23.48786465467241058, 11.44779295918254647 ) ) ;
#51502 = EDGE_CURVE ( 'NONE', #62579, #5690, #53750, .T. ) ;
#51501 = ORIENTED_EDGE ( 'NONE', *, *, #67948, .T. ) ;
#51503 = CARTESIAN_POINT ( 'NONE',  ( 18.51311748589099082, 11.02308708543723270, -1.500000000000002220 ) ) ;
#51504 = CARTESIAN_POINT ( 'NONE',  ( -56.52287095715006870, -24.64898659630367916, 1.056161002820822592 ) ) ;
#51505 = CARTESIAN_POINT ( 'NONE',  ( -70.51930845923730828, -25.12219141572745684, 7.087032725586937865 ) ) ;
#51506 = DIRECTION ( 'NONE',  ( -3.773278334453080206E-23, 0.9999999999976377785, 2.173523156925979975E-06 ) ) ;
#51507 = CARTESIAN_POINT ( 'NONE',  ( -99.52764846858842418, -25.27473375014014678, 3.999772248440511824 ) ) ;
#51508 = CARTESIAN_POINT ( 'NONE',  ( -21.75629724252761577, 7.406401271465676395, -1.500000000000002220 ) ) ;
#51509 = COORDINATED_UNIVERSAL_TIME_OFFSET ( 0, 0, .AHEAD. ) ;
#51510 = CARTESIAN_POINT ( 'NONE',  ( -49.52287095715006160, -24.64965694238406613, 8.947790433994203596 ) ) ;
#51511 = CARTESIAN_POINT ( 'NONE',  ( 32.60294298177590377, 2.682774720514426559, -11.48871326860665931 ) ) ;
#51512 = CARTESIAN_POINT ( 'NONE',  ( -5.623992922573770592, 19.38241096367466199, 11.49999999999999645 ) ) ;
#51513 = CARTESIAN_POINT ( 'NONE',  ( -109.2412217894342916, -25.10927504460140725, 3.330161293093501396 ) ) ;
#51514 = CARTESIAN_POINT ( 'NONE',  ( -91.52287095715009002, -23.73907113216989728, -1.053371485793250129 ) ) ;
#51515 = PRODUCT ( 'Plastic Part 2', 'Plastic Part 2', '', ( #74216 ) ) ;
#51516 = CARTESIAN_POINT ( 'NONE',  ( -104.5562042904834215, -24.65952944569305316, 1.056160979905702568 ) ) ;
#51517 = CARTESIAN_POINT ( 'NONE',  ( -121.6228709571500417, -24.65952944569305316, 1.056160979905705677 ) ) ;
#51518 = FACE_OUTER_BOUND ( 'NONE', #32349, .T. ) ;
#51520 = EDGE_CURVE ( 'NONE', #39655, #50276, #93102, .T. ) ;
#51519 = CARTESIAN_POINT ( 'NONE',  ( -19.70454523906213495, -2.556213046838741842, -1.500000000000002220 ) ) ;
#51521 = CARTESIAN_POINT ( 'NONE',  ( -113.5144507812068753, -24.65952944569304606, 1.056160979905704789 ) ) ;
#51522 = CARTESIAN_POINT ( 'NONE',  ( 19.74453702311487646, -0.1846442961375113490, -1.500000000000002220 ) ) ;
#51523 = VECTOR ( 'NONE', #21037, 1000.000000000000114 ) ;
#51524 = CARTESIAN_POINT ( 'NONE',  ( -126.5896042291024202, -24.35071581493544457, 9.817618358456011052 ) ) ;
#51525 = CARTESIAN_POINT ( 'NONE',  ( -0.4686347352592966087, -6.376774720514411854, 19.46274624311237034 ) ) ;
#51526 = DIRECTION ( 'NONE',  ( 0.000000000000000000, -2.173523156925979552E-06, 0.9999999999976378895 ) ) ;
#51527 = CARTESIAN_POINT ( 'NONE',  ( -7.851838630353038972, -19.11370409007043847, 11.49999999999999645 ) ) ;
#51528 = CARTESIAN_POINT ( 'NONE',  ( -53.58953762381672448, -24.66019654487199020, 8.947790411086131712 ) ) ;
#51529 = EDGE_CURVE ( 'NONE', #38437, #43756, #44027, .T. ) ;
#51530 = CIRCLE ( 'NONE', #69336, 1.306876713926001354 ) ;
#51531 = CARTESIAN_POINT ( 'NONE',  ( 31.30917625415073502, 4.464831821618584051, 0.9454093304329914682 ) ) ;
#51532 = CARTESIAN_POINT ( 'NONE',  ( -22.63693132222386950, 1.387278323242118416, 11.49999999999999645 ) ) ;
#51533 = ORIENTED_EDGE ( 'NONE', *, *, #87828, .T. ) ;
#51534 = CARTESIAN_POINT ( 'NONE',  ( -1.044871794871793602, -6.376774720514418959, 20.44941907051282115 ) ) ;
#51535 = EDGE_CURVE ( 'NONE', #70943, #98477, #99717, .T. ) ;
#51536 = CARTESIAN_POINT ( 'NONE',  ( -62.58953762381672448, -23.47593901973091235, -1.443836447539007972 ) ) ;
#51537 = AXIS2_PLACEMENT_3D ( 'NONE', #80809, #73204, #11292 ) ;
#51538 = CARTESIAN_POINT ( 'NONE',  ( -63.49532551922489176, -24.51314013834316796, 0.6176544820404160641 ) ) ;
#51539 = ADVANCED_FACE ( 'NONE', ( #1275 ), #8877, .T. ) ;
#51540 = DIRECTION ( 'NONE',  ( 0.000000000000000000, -1.000000000000000000, 0.000000000000000000 ) ) ;
#51541 = ORIENTED_EDGE ( 'NONE', *, *, #30695, .T. ) ;
#51542 = EDGE_CURVE ( 'NONE', #73142, #59834, #39821, .T. ) ;
#51543 = VERTEX_POINT ( 'NONE', #24590 ) ;
#51544 = DIRECTION ( 'NONE',  ( 1.000000000000000000, 0.000000000000000000, 0.000000000000000000 ) ) ;
#51545 = CARTESIAN_POINT ( 'NONE',  ( -6.237877366497927234, -22.00199818733190327, -1.500000000000002220 ) ) ;
#51547 = EDGE_CURVE ( 'NONE', #31857, #85110, #94881, .T. ) ;
#51546 = CARTESIAN_POINT ( 'NONE',  ( -6.660000000000001030, -9.123836073446797812, -2.666350264951732552 ) ) ;
#51548 = CARTESIAN_POINT ( 'NONE',  ( -13.01863397230089170, 17.21462230531794901, -1.500000000000002220 ) ) ;
#51549 = AXIS2_PLACEMENT_3D ( 'NONE', #93541, #78810, #1217 ) ;
#51550 = CARTESIAN_POINT ( 'NONE',  ( -113.5871604955099059, -24.66019654487200086, 8.947790411086106843 ) ) ;
#51551 = CARTESIAN_POINT ( 'NONE',  ( -32.55620429048340014, -23.48783264082478084, -1.443836473390075037 ) ) ;
#51552 = CARTESIAN_POINT ( 'NONE',  ( 4.940617368476682536, -22.01678987175928981, 11.49999999999999645 ) ) ;
#51553 = VERTEX_POINT ( 'NONE', #8374 ) ;
#51554 = CARTESIAN_POINT ( 'NONE',  ( -43.52287095715005449, -23.96127896942127933, -0.6493128930940295085 ) ) ;
#51555 = CARTESIAN_POINT ( 'NONE',  ( 17.26801960494244881, -13.64313956103151071, 11.49999999999998934 ) ) ;
#51556 = CARTESIAN_POINT ( 'NONE',  ( -64.52287095715006160, -24.50216790748205398, 0.6166512839542503954 ) ) ;
#51557 = CARTESIAN_POINT ( 'NONE',  ( -41.58766378979927936, -25.10925883918385537, 3.364589983749641799 ) ) ;
#51558 = EDGE_LOOP ( 'NONE', ( #30483, #10273, #15103, #27225, #55284, #45632 ) ) ;
#51559 = EDGE_CURVE ( 'NONE', #16105, #99116, #31613, .T. ) ;
#51560 = PLANE ( 'NONE',  #81611 ) ;
#51561 = CARTESIAN_POINT ( 'NONE',  ( -90.62479060358214156, -24.92592662359561473, 8.075495903018000021 ) ) ;
#51562 = ORIENTED_EDGE ( 'NONE', *, *, #38024, .F. ) ;
#51563 = LINE ( 'NONE', #28718, #33919 ) ;
#51564 = ORIENTED_EDGE ( 'NONE', *, *, #74322, .F. ) ;
#51565 = EDGE_LOOP ( 'NONE', ( #928, #80976 ) ) ;
#51566 = CARTESIAN_POINT ( 'NONE',  ( -65.52287095715004739, -24.91544648472619627, 1.928969306349230806 ) ) ;
#51567 = CARTESIAN_POINT ( 'NONE',  ( -92.62287095715005592, -23.48786465467241413, 11.44779295918254469 ) ) ;
#51568 = CARTESIAN_POINT ( 'NONE',  ( -57.62781167713143304, -24.51314013834315375, 0.6176544820404114011 ) ) ;
#51569 = CARTESIAN_POINT ( 'NONE',  ( 5.143668500415711442, -19.74887971880038151, -1.500000000000002220 ) ) ;
#51570 = ORIENTED_EDGE ( 'NONE', *, *, #44414, .T. ) ;
#51571 = CARTESIAN_POINT ( 'NONE',  ( -2.889365861140832159, -6.376774720514410077, 19.43823095447973870 ) ) ;
#51572 = CARTESIAN_POINT ( 'NONE',  ( -105.5497180537893200, -24.63355581998386867, 0.9682620441943899925 ) ) ;
#51573 = PLANE ( 'NONE',  #17266 ) ;
#51574 = ORIENTED_EDGE ( 'NONE', *, *, #34775, .F. ) ;
#51575 = CARTESIAN_POINT ( 'NONE',  ( -100.5228709571500616, -23.47596703998600631, 11.44779298504228215 ) ) ;
#51576 = CARTESIAN_POINT ( 'NONE',  ( -27.99827674658315502, -24.63646060442122732, 8.232207369485870174 ) ) ;
#51577 = ORIENTED_EDGE ( 'NONE', *, *, #50241, .T. ) ;
#51578 = CARTESIAN_POINT ( 'NONE',  ( 1.081820405348005165, -20.78239343107542680, 11.49999999999998934 ) ) ;
#51579 = ORIENTED_EDGE ( 'NONE', *, *, #36887, .F. ) ;
#51581 = VERTEX_POINT ( 'NONE', #71281 ) ;
#51580 = CARTESIAN_POINT ( 'NONE',  ( -101.5985593676237499, -23.48783264082477018, -1.443836473390089248 ) ) ;
#51582 = B_SPLINE_CURVE_WITH_KNOTS ( 'NONE', 3,
 ( #38445, #69397, #31841, #71407 ),
 .UNSPECIFIED., .F., .F.,
 ( 4, 4 ),
 ( 0.000000000000000000, 0.0001000000000000028644 ),
 .UNSPECIFIED. ) ;
#51583 = B_SPLINE_SURFACE_WITH_KNOTS ( 'NONE', 3, 1, ( 
 ( #60566, #92481 ),
 ( #22953, #5759 ),
 ( #91988, #76743 ),
 ( #7244, #22459 ),
 ( #53447, #15355 ),
 ( #90992, #20973 ),
 ( #53945, #21963 ),
 ( #84874, #46320 ),
 ( #98599, #76255 ),
 ( #5260, #91484 ),
 ( #84375, #82874 ),
 ( #13360, #75265 ),
 ( #71667, #7753 ),
 ( #64076, #54941 ),
 ( #85882, #8763 ),
 ( #71165, #31084 ),
 ( #17873, #23971 ),
 ( #9250, #32592 ),
 ( #16360, #39699 ) ),
 .UNSPECIFIED., .F., .F., .F.,
 ( 4, 1, 1, 1, 1, 1, 1, 1, 1, 1, 1, 1, 1, 1, 1, 1, 4 ),
 ( 2, 2 ),
 ( 0.000000000000000000, 0.06420729528298517452, 0.1264246897797454694, 0.1876802842649225589, 0.2482164244552149956, 0.3083050600086130189, 0.3696609913251429069, 0.4316985517867830136, 0.4959468922087650333, 0.5597580239721172690, 0.6222954078261602184, 0.6839106352841730629, 0.7450924080566231344, 0.8067402253892927977, 0.8690866181212024699, 0.9332900029747993598, 1.000000000000000000 ),
 ( 0.000000000000000000, 1.000000000000000000 ),
 .UNSPECIFIED. ) ;
#51584 = CARTESIAN_POINT ( 'NONE',  ( 30.53060340732036337, 5.297812262124996785, 1.539714685317421505 ) ) ;
#51585 = PLANE ( 'NONE',  #13034 ) ;
#51586 = VERTEX_POINT ( 'NONE', #1769 ) ;
#51587 = VERTEX_POINT ( 'NONE', #81886 ) ;
#51588 = CARTESIAN_POINT ( 'NONE',  ( -78.62287095715005592, -24.51283580621364777, 0.6167428607019836972 ) ) ;
#51589 = CARTESIAN_POINT ( 'NONE',  ( -76.52287095715011844, -24.33927499327856125, 9.819080762295813614 ) ) ;
#51590 = CARTESIAN_POINT ( 'NONE',  ( -52.62287095715004881, -23.96177878511308634, 10.65340807706330217 ) ) ;
#51591 = CARTESIAN_POINT ( 'NONE',  ( -71.20303962927951602, -25.24515144792784227, 5.785490083912771198 ) ) ;
#51593 = ORIENTED_EDGE ( 'NONE', *, *, #20604, .F. ) ;
#51592 = CARTESIAN_POINT ( 'NONE',  ( 14.67205787815721862, 16.58792043909384262, 11.49999999999999645 ) ) ;
#51594 = CARTESIAN_POINT ( 'NONE',  ( -108.6261718626276149, -24.34968618360934300, 0.1864209137778971292 ) ) ;
#51595 = CARTESIAN_POINT ( 'NONE',  ( 22.57354875331468591, -1.174960877787051716, -1.500000000000002220 ) ) ;
#51596 = AXIS2_PLACEMENT_3D ( 'NONE', #76684, #37146, #77687 ) ;
#51598 = ORIENTED_EDGE ( 'NONE', *, *, #53511, .T. ) ;
#51597 = CARTESIAN_POINT ( 'NONE',  ( -46.52287095715006160, -23.48786465467241058, 11.44779295918255002 ) ) ;
#51599 = ORIENTED_EDGE ( 'NONE', *, *, #26993, .F. ) ;
#51600 = CARTESIAN_POINT ( 'NONE',  ( -78.55620429048339304, -24.66019654487199730, 8.947790411086128159 ) ) ;
#51601 = EDGE_CURVE ( 'NONE', #93020, #64856, #26607, .T. ) ;
#51602 = CARTESIAN_POINT ( 'NONE',  ( -57.65693448539914812, -23.48786465467241058, 11.44779295918254647 ) ) ;
#51603 = ORIENTED_EDGE ( 'NONE', *, *, #17223, .T. ) ;
#51604 = EDGE_CURVE ( 'NONE', #88839, #93802, #64191, .T. ) ;
#51605 = VECTOR ( 'NONE', #51779, 1000.000000000000000 ) ;
#51606 = CARTESIAN_POINT ( 'NONE',  ( -126.5228709571500616, -23.73907113216990084, -1.053371485793243911 ) ) ;
#51607 = CARTESIAN_POINT ( 'NONE',  ( 14.63995501510512653, -16.76770752772931772, -1.500000000000002220 ) ) ;
#51608 = CARTESIAN_POINT ( 'NONE',  ( -24.90875734969025501, -3.316774720514426456, 26.43402280011862615 ) ) ;
#51609 = EDGE_CURVE ( 'NONE', #3529, #45653, #4765, .T. ) ;
#51610 = ORIENTED_EDGE ( 'NONE', *, *, #48272, .F. ) ;
#51611 = CARTESIAN_POINT ( 'NONE',  ( -110.5895376238167387, -23.48786465467241769, 11.44779295918254114 ) ) ;
#51612 = LINE ( 'NONE', #15027, #79970 ) ;
#51613 = DIRECTION ( 'NONE',  ( -3.773278334453080206E-23, 0.9999999999976377785, 2.173523156925979975E-06 ) ) ;
#51614 = EDGE_CURVE ( 'NONE', #34532, #17884, #72287, .T. ) ;
#51615 = ADVANCED_FACE ( 'NONE', ( #12362 ), #25601, .F. ) ;
#51616 = CARTESIAN_POINT ( 'NONE',  ( -108.6228709571500701, -23.96127896941633750, -0.6493128931037804863 ) ) ;
#51617 = CARTESIAN_POINT ( 'NONE',  ( -63.62287095715004881, -29.50247984919015209, -1.443849546365056913 ) ) ;
#51619 = CIRCLE ( 'NONE', #77528, 1.835999999999999632 ) ;
#51618 = CARTESIAN_POINT ( 'NONE',  ( 14.32981562401322506, -13.22600733894156200, -1.500000000000002220 ) ) ;
#51620 = ADVANCED_FACE ( 'NONE', ( #73283 ), #41332, .F. ) ;
#51621 = CARTESIAN_POINT ( 'NONE',  ( -15.31780299886000485, -15.04297462106122474, 11.49999999999998934 ) ) ;
#51622 = CARTESIAN_POINT ( 'NONE',  ( -25.54641640974780259, -24.58000095359798820, 4.381686515786591407 ) ) ;
#51623 = DIRECTION ( 'NONE',  ( 0.000000000000000000, 0.000000000000000000, -1.000000000000000000 ) ) ;
#51624 = FACE_BOUND ( 'NONE', #10379, .T. ) ;
#51625 = CARTESIAN_POINT ( 'NONE',  ( -7.631545101075025705, 21.52643039700453897, -1.500000000000002220 ) ) ;
#51626 = DATE_AND_TIME ( #53131, #11590 ) ;
#51627 = CARTESIAN_POINT ( 'NONE',  ( -106.5141254747104824, -24.35071581493544457, 9.817618358456019934 ) ) ;
#51628 = DIRECTION ( 'NONE',  ( 0.000000000000000000, 0.000000000000000000, 1.000000000000000000 ) ) ;
#51629 = CARTESIAN_POINT ( 'NONE',  ( 13.83478396660306942, -14.44641118834825910, 11.49999999999999645 ) ) ;
#51630 = FACE_OUTER_BOUND ( 'NONE', #52532, .T. ) ;
#51631 = CARTESIAN_POINT ( 'NONE',  ( -57.58953762381671737, -23.48786465467241058, 11.44779295918254824 ) ) ;
#51632 = CARTESIAN_POINT ( 'NONE',  ( -76.52287095715007581, -23.47596703998600631, 11.44779298504228571 ) ) ;
#51633 = ORIENTED_EDGE ( 'NONE', *, *, #97033, .T. ) ;
#51634 = CARTESIAN_POINT ( 'NONE',  ( 33.69795529655567634, -0.6647747205144264315, 23.11160796525322070 ) ) ;
#51635 = EDGE_CURVE ( 'NONE', #42990, #78774, #95112, .T. ) ;
#51636 = CARTESIAN_POINT ( 'NONE',  ( -65.52287095715010423, -24.15516710230292929, 10.28746687063725851 ) ) ;
#51637 = CARTESIAN_POINT ( 'NONE',  ( 19.97611268498323511, -8.487024919450899318, -1.500000000000002220 ) ) ;
#51638 = CARTESIAN_POINT ( 'NONE',  ( -60.62287095715004881, -25.00158670708908915, 2.256160236439166855 ) ) ;
#51639 = CARTESIAN_POINT ( 'NONE',  ( 12.76379665850700640, 14.79237594083867080, -1.500000000000002220 ) ) ;
#51640 = CARTESIAN_POINT ( 'NONE',  ( -129.5228709571500758, -29.50250786944525672, 11.44777988621622633 ) ) ;
#51641 = B_SPLINE_CURVE_WITH_KNOTS ( 'NONE', 3,
 ( #23401, #54387, #11698, #65527 ),
 .UNSPECIFIED., .F., .F.,
 ( 4, 4 ),
 ( 0.000000000000000000, 0.0001000000000000028915 ),
 .UNSPECIFIED. ) ;
#51642 = B_SPLINE_CURVE_WITH_KNOTS ( 'NONE', 3,
 ( #19779, #51750, #73095, #19284 ),
 .UNSPECIFIED., .F., .F.,
 ( 4, 4 ),
 ( 0.000000000000000000, 1.000000000000000000 ),
 .UNSPECIFIED. ) ;
#51643 = EDGE_CURVE ( 'NONE', #21243, #54056, #58558, .T. ) ;
#51644 = ORIENTED_EDGE ( 'NONE', *, *, #35484, .F. ) ;
#51645 = PERSON_AND_ORGANIZATION_ROLE ( 'classification_officer' ) ;
#51646 = FACE_OUTER_BOUND ( 'NONE', #3656, .T. ) ;
#51647 = CARTESIAN_POINT ( 'NONE',  ( 26.73860345374794178, 5.236715237616461849, -5.784298989603305685 ) ) ;
#51648 = CARTESIAN_POINT ( 'NONE',  ( 5.889875310795558150, 19.62242631308348706, 11.49999999999999645 ) ) ;
#51649 = CARTESIAN_POINT ( 'NONE',  ( 9.451856243913134392, -6.475225279485569807, -27.03492916892036746 ) ) ;
#51650 = CARTESIAN_POINT ( 'NONE',  ( -113.5562042904833788, -24.66019654487199730, 8.947790411086124607 ) ) ;
#51651 = VERTEX_POINT ( 'NONE', #34223 ) ;
#51652 = CARTESIAN_POINT ( 'NONE',  ( -109.4120340803280982, -25.29715050432110601, 4.545091671428740376 ) ) ;
#51653 = CARTESIAN_POINT ( 'NONE',  ( -39.44687923781921057, -25.28892616455411613, 4.188173659901107904 ) ) ;
#51654 = CARTESIAN_POINT ( 'NONE',  ( -127.6228709571500559, -23.47593901973091235, -1.443836447538995760 ) ) ;
#51655 = VECTOR ( 'NONE', #92388, 1000.000000000000114 ) ;
#51656 = CARTESIAN_POINT ( 'NONE',  ( -123.5228709571500474, -24.50321055353804311, 9.387540953477502725 ) ) ;
#51657 = ORIENTED_EDGE ( 'NONE', *, *, #44272, .T. ) ;
#51658 = DIRECTION ( 'NONE',  ( 0.000000000000000000, 0.000000000000000000, 1.000000000000000000 ) ) ;
#51659 = AXIS2_PLACEMENT_3D ( 'NONE', #52190, #67926, #45084 ) ;
#51660 = EDGE_CURVE ( 'NONE', #18886, #47314, #12126, .T. ) ;
#51661 = CARTESIAN_POINT ( 'NONE',  ( -20.34888222059871410, 10.79260868881566715, 11.49999999999999645 ) ) ;
#51662 = CARTESIAN_POINT ( 'NONE',  ( -21.15473383059569557, 8.456223909384457116, 11.49999999999998934 ) ) ;
#51663 = LINE ( 'NONE', #22182, #17836 ) ;
#51664 = CARTESIAN_POINT ( 'NONE',  ( -54.52287095715006870, -29.50247984919015209, -1.443849546365058689 ) ) ;
#51665 = CARTESIAN_POINT ( 'NONE',  ( -60.72380231473932355, -25.13069340115295702, 2.947789388436138580 ) ) ;
#51666 = VECTOR ( 'NONE', #31673, 1000.000000000000000 ) ;
#51667 = PLANE ( 'NONE',  #17133 ) ;
#51668 = CARTESIAN_POINT ( 'NONE',  ( -110.5509718465033018, -24.63355581998384380, 0.9682620441943931011 ) ) ;
#51669 = EDGE_CURVE ( 'NONE', #76243, #88521, #6466, .T. ) ;
#51670 = CARTESIAN_POINT ( 'NONE',  ( 18.32745805453730981, -11.99952526121574259, 11.49999999999998934 ) ) ;
#51671 = CARTESIAN_POINT ( 'NONE',  ( 6.420673076923079314, -5.876774720514427841, 21.83974358974358765 ) ) ;
#51672 = B_SPLINE_CURVE_WITH_KNOTS ( 'NONE', 3,
 ( #21378, #60481, #91397, #558 ),
 .UNSPECIFIED., .F., .F.,
 ( 4, 4 ),
 ( 0.000000000000000000, 1.000000000000000000 ),
 .UNSPECIFIED. ) ;
#51673 = LINE ( 'NONE', #59793, #93025 ) ;
#51674 = CARTESIAN_POINT ( 'NONE',  ( -103.5562042904833930, -24.65952944569304606, 1.056160979905701680 ) ) ;
#51675 = DIRECTION ( 'NONE',  ( -4.015954566446630556E-15, -1.000000000000000000, -1.297050502119899750E-15 ) ) ;
#51676 = ORIENTED_EDGE ( 'NONE', *, *, #52866, .T. ) ;
#51677 = B_SPLINE_CURVE_WITH_KNOTS ( 'NONE', 3,
 ( #89837, #64539, #89346, #10723, #81728, #20308 ),
 .UNSPECIFIED., .F., .F.,
 ( 4, 2, 4 ),
 ( 6.391158118969316353E-06, 0.001387004593080787881, 0.002767618028042606766 ),
 .UNSPECIFIED. ) ;
#51678 = CARTESIAN_POINT ( 'NONE',  ( 20.14718400222343320, -3.498931157112906476, -1.500000000000002220 ) ) ;
#51679 = VERTEX_POINT ( 'NONE', #87502 ) ;
#51680 = EDGE_LOOP ( 'NONE', ( #46212, #62805, #95448, #37692 ) ) ;
#51681 = ORIENTED_EDGE ( 'NONE', *, *, #73281, .F. ) ;
#51682 = ORIENTED_EDGE ( 'NONE', *, *, #76895, .F. ) ;
#51683 = CARTESIAN_POINT ( 'NONE',  ( -22.27228905017084060, 5.866681652885556986, 11.49999999999998934 ) ) ;
#51684 = DIRECTION ( 'NONE',  ( 0.000000000000000000, -1.000000000000000000, -0.000000000000000000 ) ) ;
#51685 = CARTESIAN_POINT ( 'NONE',  ( 20.24638344296597836, 0.1212440198127159030, -1.500000000000002220 ) ) ;
#51686 = ORIENTED_EDGE ( 'NONE', *, *, #79921, .F. ) ;
#51687 = DIRECTION ( 'NONE',  ( -3.773278334444167608E-23, 1.000000000000000000, 0.000000000000000000 ) ) ;
#51688 = PLANE ( 'NONE',  #33638 ) ;
#51689 = CARTESIAN_POINT ( 'NONE',  ( -95.54323782235148599, -24.92564183028979485, 1.928384488918254425 ) ) ;
#51690 = CARTESIAN_POINT ( 'NONE',  ( -53.56763007331336723, -23.48786465467240703, 11.44779295918255002 ) ) ;
#51692 = ORIENTED_EDGE ( 'NONE', *, *, #68448, .F. ) ;
#51691 = CARTESIAN_POINT ( 'NONE',  ( 21.15477495681221143, 3.540436534888726783, 11.49999999999999645 ) ) ;
#51693 = CARTESIAN_POINT ( 'NONE',  ( 32.16024265030974050, -5.965225279485572685, 14.03360796525321774 ) ) ;
#51694 = ORIENTED_EDGE ( 'NONE', *, *, #70217, .F. ) ;
#51695 = CARTESIAN_POINT ( 'NONE',  ( 14.63995501510512653, -16.76770752772931772, -1.500000000000002220 ) ) ;
#51696 = CARTESIAN_POINT ( 'NONE',  ( 7.508984785159893427, -19.29828013722326929, -1.500000000000002220 ) ) ;
#51698 = CLOSED_SHELL ( 'NONE', ( #92542, #89023, #93682, #62388, #73182, #62176, #37177, #71440, #34314, #22615, #79672, #1810, #1825, #31722, #89823, #10591, #91958, #65386, #86031, #83450, #82390, #53892, #22413, #37816, #10964, #49015, #19023, #84481, #31582, #26594, #22474, #26622, #79806, #59065, #8224, #11530, #92659 ) ) ;
#51697 = ORIENTED_EDGE ( 'NONE', *, *, #45378, .F. ) ;
#51699 = CARTESIAN_POINT ( 'NONE',  ( -28.66134147976880442, -23.58502333657346028, -1.055554491438110309 ) ) ;
#51700 = ORIENTED_EDGE ( 'NONE', *, *, #48454, .T. ) ;
#51701 = LINE ( 'NONE', #89260, #57502 ) ;
#51702 = ORIENTED_EDGE ( 'NONE', *, *, #21720, .T. ) ;
#51703 = CARTESIAN_POINT ( 'NONE',  ( 20.88312143257166653, -1.666129412636018214, -1.500000000000002220 ) ) ;
#51704 = CARTESIAN_POINT ( 'NONE',  ( -11.13288495942205536, 18.84158392345546318, 11.49999999999999645 ) ) ;
#51705 = CARTESIAN_POINT ( 'NONE',  ( -73.64405303056334162, -23.73791477778911840, 11.05961554403170766 ) ) ;
#51706 = CARTESIAN_POINT ( 'NONE',  ( -6.869692127560369066, -21.44495933931894527, -1.500000000000002220 ) ) ;
#51707 = CARTESIAN_POINT ( 'NONE',  ( 17.97375762979478253, -10.76934015532128797, -1.500000000000002220 ) ) ;
#51708 = CARTESIAN_POINT ( 'NONE',  ( 6.127395130496778641, -6.376774720514417183, 20.13872869980892943 ) ) ;
#51709 = CARTESIAN_POINT ( 'NONE',  ( -119.6248171011402519, -24.35071581493544457, 9.817618358456018157 ) ) ;
#51710 = CARTESIAN_POINT ( 'NONE',  ( -31.24388727629348494, -29.50250091417111520, 8.247779886223803203 ) ) ;
#51711 = EDGE_LOOP ( 'NONE', ( #11255, #87893, #78070, #34043, #23098, #38974 ) ) ;
#51712 = ORIENTED_EDGE ( 'NONE', *, *, #67777, .T. ) ;
#51713 = ORIENTED_EDGE ( 'NONE', *, *, #17001, .F. ) ;
#51714 = B_SPLINE_CURVE_WITH_KNOTS ( 'NONE', 3,
 ( #1097, #85829, #78692, #1604 ),
 .UNSPECIFIED., .F., .F.,
 ( 4, 4 ),
 ( 0.000000000000000000, 9.999999999999592548E-05 ),
 .UNSPECIFIED. ) ;
#51715 = CARTESIAN_POINT ( 'NONE',  ( -66.65278898335940028, -23.48783264082476308, -1.443836473390097463 ) ) ;
#51716 = CARTESIAN_POINT ( 'NONE',  ( -5.860608850286626925, 20.67097946995454905, -1.500000000000002220 ) ) ;
#51717 = ADVANCED_FACE ( 'NONE', ( #17989 ), #66191, .F. ) ;
#51718 = DIRECTION ( 'NONE',  ( -3.773278334453079618E-23, 0.9999999999976377785, 2.173523156925979975E-06 ) ) ;
#51719 = ORIENTED_EDGE ( 'NONE', *, *, #83070, .F. ) ;
#51720 = CARTESIAN_POINT ( 'NONE',  ( -13.19772682967519195, -16.48504770976277101, -1.500000000000002220 ) ) ;
#51721 = CARTESIAN_POINT ( 'NONE',  ( -100.4326965455114902, -25.19502912051678578, 3.293943094755625633 ) ) ;
#51722 = VECTOR ( 'NONE', #56675, 1000.000000000000000 ) ;
#51723 = ADVANCED_FACE ( 'NONE', ( #42351 ), #79878, .F. ) ;
#51724 = CARTESIAN_POINT ( 'NONE',  ( -64.57975988545082657, -24.65952944569304250, 1.056160979905695685 ) ) ;
#51726 = CARTESIAN_POINT ( 'NONE',  ( -83.55442485235529659, -23.96169478059713143, 10.65365249895718058 ) ) ;
#51725 = VECTOR ( 'NONE', #59155, 1000.000000000000000 ) ;
#51727 = DIRECTION ( 'NONE',  ( -3.773278334453079618E-23, 0.9999999999976377785, 2.173523156925979975E-06 ) ) ;
#51728 = DIRECTION ( 'NONE',  ( -0.000000000000000000, 2.173523156925979552E-06, -0.9999999999976378895 ) ) ;
#51729 = CARTESIAN_POINT ( 'NONE',  ( -11.88820881604258339, -18.65297325734525913, -1.500000000000002220 ) ) ;
#51730 = DIRECTION ( 'NONE',  ( 0.000000000000000000, -1.000000000000000000, 0.000000000000000000 ) ) ;
#51731 = EDGE_CURVE ( 'NONE', #34090, #15342, #10372, .T. ) ;
#51732 = CARTESIAN_POINT ( 'NONE',  ( -109.0560589239626950, -25.30235252500154175, 4.712086642211391840 ) ) ;
#51733 = DIRECTION ( 'NONE',  ( 1.000000000000000000, 0.000000000000000000, 0.000000000000000000 ) ) ;
#51734 = AXIS2_PLACEMENT_3D ( 'NONE', #24861, #47718, #10145 ) ;
#51735 = ADVANCED_FACE ( 'NONE', ( #50442 ), #42841, .F. ) ;
#51736 = B_SPLINE_CURVE_WITH_KNOTS ( 'NONE', 3,
 ( #35079, #43197, #58914, #98450 ),
 .UNSPECIFIED., .F., .F.,
 ( 4, 4 ),
 ( 0.000000000000000000, 9.999999999998897304E-05 ),
 .UNSPECIFIED. ) ;
#51737 = CARTESIAN_POINT ( 'NONE',  ( -100.6369790529841310, -23.85016227208580020, -0.8807180028928295323 ) ) ;
#51738 = AXIS2_PLACEMENT_3D ( 'NONE', #88126, #54801, #61911 ) ;
#51739 = CARTESIAN_POINT ( 'NONE',  ( -17.77321681866180469, -7.816401696202086136, -1.500000000000002220 ) ) ;
#51740 = AXIS2_PLACEMENT_3D ( 'NONE', #31441, #23314, #14203 ) ;
#51741 = CARTESIAN_POINT ( 'NONE',  ( -1.966620079519992181, -21.27258529651320274, -1.500000000000002220 ) ) ;
#51742 = DIRECTION ( 'NONE',  ( -3.773278334453080206E-23, 0.9999999999976377785, 2.173523156925979975E-06 ) ) ;
#51743 = EDGE_CURVE ( 'NONE', #45940, #42876, #7273, .T. ) ;
#51744 = CARTESIAN_POINT ( 'NONE',  ( -91.16090919880674903, -25.31768024997816013, 4.634761245912265792 ) ) ;
#51745 = FACE_OUTER_BOUND ( 'NONE', #72675, .T. ) ;
#51746 = LINE ( 'NONE', #36504, #99230 ) ;
#51747 = CARTESIAN_POINT ( 'NONE',  ( 19.67839991682829748, -11.23141783594569354, -1.500000000000002220 ) ) ;
#51748 = VERTEX_POINT ( 'NONE', #89005 ) ;
#51749 = CARTESIAN_POINT ( 'NONE',  ( -92.62287095715005592, -24.64898659630368627, 1.056161002820827921 ) ) ;
#51750 = CARTESIAN_POINT ( 'NONE',  ( -99.55620429048340725, -23.47593901973091235, -1.443836447539001089 ) ) ;
#51751 = CARTESIAN_POINT ( 'NONE',  ( 19.71268880909926580, -1.816447362451163450, 11.49999999999999645 ) ) ;
#51752 = DIRECTION ( 'NONE',  ( 0.000000000000000000, 1.000000000000000000, 0.000000000000000000 ) ) ;
#51753 = CONICAL_SURFACE ( 'NONE', #67909, 2.999999999999999112, 0.7853981633974412846 ) ;
#51754 = CARTESIAN_POINT ( 'NONE',  ( -119.5228709571500616, -24.66019654487200441, 8.947790411086108620 ) ) ;
#51755 = ORIENTED_EDGE ( 'NONE', *, *, #72123, .T. ) ;
#51756 = LINE ( 'NONE', #44639, #500 ) ;
#51757 = CARTESIAN_POINT ( 'NONE',  ( -29.47844009783932862, -24.60094155636027580, 2.848996143664383141 ) ) ;
#51758 = DIRECTION ( 'NONE',  ( 0.000000000000000000, 1.000000000000000000, 0.000000000000000000 ) ) ;
#51759 = CARTESIAN_POINT ( 'NONE',  ( 10.18377579766961283, -19.05927572544859672, 11.49999999999998934 ) ) ;
#51760 = CARTESIAN_POINT ( 'NONE',  ( -0.02075734969026423599, -3.316774720514426456, -0.08597719988137648983 ) ) ;
#51761 = CARTESIAN_POINT ( 'NONE',  ( -101.5562042904833930, -23.48786465467241413, 11.44779295918254469 ) ) ;
#51762 = CARTESIAN_POINT ( 'NONE',  ( -109.5228709571500616, -23.47593901973090524, -1.443836447538996426 ) ) ;
#51763 = DIRECTION ( 'NONE',  ( 0.7682573101345366862, 0.000000000000000000, -0.6401411605457395515 ) ) ;
#51764 = CARTESIAN_POINT ( 'NONE',  ( -18.99895575154661742, -5.639348582513488140, -1.500000000000002220 ) ) ;
#51765 = ORIENTED_EDGE ( 'NONE', *, *, #69369, .T. ) ;
#51766 = B_SPLINE_CURVE_WITH_KNOTS ( 'NONE', 3,
 ( #44324, #92465, #44820, #75740 ),
 .UNSPECIFIED., .F., .F.,
 ( 4, 4 ),
 ( 0.000000000000000000, 0.009506788565010804160 ),
 .UNSPECIFIED. ) ;
#51767 = CARTESIAN_POINT ( 'NONE',  ( 0.8729654516333695824, -20.24016528753796962, 11.49999999999999645 ) ) ;
#51768 = DIRECTION ( 'NONE',  ( 1.000000000000000000, 3.773278334444166432E-23, 8.201307841325785021E-29 ) ) ;
#51769 = AXIS2_PLACEMENT_3D ( 'NONE', #63631, #45895, #8824 ) ;
#51770 = CARTESIAN_POINT ( 'NONE',  ( 33.62145766639996936, -4.037870770857248104, -12.08356088300365094 ) ) ;
#51771 = ORIENTED_EDGE ( 'NONE', *, *, #48794, .T. ) ;
#51772 = B_SPLINE_SURFACE_WITH_KNOTS ( 'NONE', 3, 3, ( 
 ( #14348, #31580, #133, #47318 ),
 ( #39190, #92971, #14848, #77237 ),
 ( #632, #77736, #32080, #85362 ),
 ( #70650, #38690, #70146, #92471 ),
 ( #69656, #63056, #39691, #45324 ),
 ( #15348, #76246, #99574, #6743 ),
 ( #53935, #45814, #23963, #54429 ) ),
 .UNSPECIFIED., .F., .F., .F.,
 ( 4, 3, 4 ),
 ( 4, 4 ),
 ( 0.7945040050992245861, 0.8970133687736505657, 0.9995227324480764342 ),
 ( 0.6196514592668809218, 0.6209502560550047567 ),
 .UNSPECIFIED. ) ;
#51773 = CARTESIAN_POINT ( 'NONE',  ( -30.60464735295150263, -24.58764167366260622, 9.439037205594624780 ) ) ;
#51774 = LINE ( 'NONE', #97441, #34728 ) ;
#51775 = CARTESIAN_POINT ( 'NONE',  ( -71.52287095715010423, -23.96177878511308279, 10.65340807706330217 ) ) ;
#51776 = DIRECTION ( 'NONE',  ( 0.000000000000000000, 0.000000000000000000, -1.000000000000000000 ) ) ;
#51777 = CARTESIAN_POINT ( 'NONE',  ( -31.52287095715005449, -24.50321055353804311, 9.387540953477531147 ) ) ;
#51778 = CARTESIAN_POINT ( 'NONE',  ( -5.826506878040391690, 19.21762618028343184, -1.500000000000002220 ) ) ;
#51779 = DIRECTION ( 'NONE',  ( 0.000000000000000000, 0.000000000000000000, 1.000000000000000000 ) ) ;
#51780 = ORIENTED_EDGE ( 'NONE', *, *, #77008, .T. ) ;
#51781 = CARTESIAN_POINT ( 'NONE',  ( 20.53691900564983186, 10.01969956684014207, 11.49999999999999645 ) ) ;
#51782 = CARTESIAN_POINT ( 'NONE',  ( -102.5228709571500616, -24.50216790748204332, 0.6166512839542633850 ) ) ;
#51783 = CARTESIAN_POINT ( 'NONE',  ( -125.6228709571500559, -29.50250786944525672, 11.44777988621622633 ) ) ;
#51784 = DIRECTION ( 'NONE',  ( -0.000000000000000000, 2.173523156925979552E-06, -0.9999999999976378895 ) ) ;
#51785 = CARTESIAN_POINT ( 'NONE',  ( 30.54125281784916268, 0.6647747205144264315, 23.11160796525322070 ) ) ;
#51787 = EDGE_CURVE ( 'NONE', #47794, #58273, #89497, .T. ) ;
#51786 = AXIS2_PLACEMENT_3D ( 'NONE', #83919, #74801, #14896 ) ;
#51788 = DIRECTION ( 'NONE',  ( 0.000000000000000000, 0.9999999999976377785, 2.173523156925979975E-06 ) ) ;
#51790 = EDGE_CURVE ( 'NONE', #33210, #5560, #1620, .T. ) ;
#51789 = CARTESIAN_POINT ( 'NONE',  ( 4.981011153104904388, 21.88276397462241363, 11.49999999999999645 ) ) ;
#51791 = LINE ( 'NONE', #82725, #56610 ) ;
#51792 = ORIENTED_EDGE ( 'NONE', *, *, #17255, .F. ) ;
#51793 = AXIS2_PLACEMENT_3D ( 'NONE', #94966, #17850, #48811 ) ;
#51794 = CARTESIAN_POINT ( 'NONE',  ( -16.75749313124890350, -11.57646860041911019, -1.500000000000002220 ) ) ;
#51795 = ORIENTED_EDGE ( 'NONE', *, *, #86346, .F. ) ;
#51796 = B_SPLINE_CURVE_WITH_KNOTS ( 'NONE', 3,
 ( #90189, #99288, #51636, #29786, #22154, #82571, #76443, #44014 ),
 .UNSPECIFIED., .F., .F.,
 ( 4, 2, 2, 4 ),
 ( 6.391158118959873630E-06, 0.002007136338672917044, 0.003007508928949899959, 0.004007881519226882440 ),
 .UNSPECIFIED. ) ;
#51797 = CARTESIAN_POINT ( 'NONE',  ( 21.44032754495887261, 8.191337786432022483, -1.500000000000002220 ) ) ;
#51798 = DIRECTION ( 'NONE',  ( -0.000000000000000000, 0.000000000000000000, 1.000000000000000000 ) ) ;
#51799 = ORIENTED_EDGE ( 'NONE', *, *, #93664, .F. ) ;
#51800 = AXIS2_PLACEMENT_3D ( 'NONE', #46223, #9159, #1058 ) ;
#51801 = CARTESIAN_POINT ( 'NONE',  ( -37.62287095715006302, -24.33832256526968507, 0.1851278514119858165 ) ) ;
#51802 = CARTESIAN_POINT ( 'NONE',  ( -77.59209893028688043, -24.15620529776628800, 10.23563542870659937 ) ) ;
#51803 = VECTOR ( 'NONE', #27359, 1000.000000000000114 ) ;
#51804 = CARTESIAN_POINT ( 'NONE',  ( -5.366453405989236813, 0.000000000000000000, 0.000000000000000000 ) ) ;
#51806 = VERTEX_POINT ( 'NONE', #28596 ) ;
#51805 = CARTESIAN_POINT ( 'NONE',  ( 9.380127297304197143, -19.07726845333505494, 11.49999999999999645 ) ) ;
#51807 = CIRCLE ( 'NONE', #63190, 0.8160000000000007248 ) ;
#51808 = ORIENTED_EDGE ( 'NONE', *, *, #65552, .F. ) ;
#51809 = CARTESIAN_POINT ( 'NONE',  ( -22.11311035156252558, 1.696007508605793301, 11.49999999999998934 ) ) ;
#51810 = CARTESIAN_POINT ( 'NONE',  ( 19.39738937107077632, -6.937168198526852514, 11.49999999999998934 ) ) ;
#51811 = B_SPLINE_CURVE_WITH_KNOTS ( 'NONE', 3,
 ( #43574, #11117, #10621, #81129, #74512, #20216 ),
 .UNSPECIFIED., .F., .F.,
 ( 4, 2, 4 ),
 ( 6.391158118959990520E-06, 0.001387004593080782460, 0.002767618028042605031 ),
 .UNSPECIFIED. ) ;
#51813 = EDGE_LOOP ( 'NONE', ( #19097, #7228, #61426, #79283 ) ) ;
#51812 = VECTOR ( 'NONE', #97133, 1000.000000000000114 ) ;
#51814 = ORIENTED_EDGE ( 'NONE', *, *, #8697, .T. ) ;
#51815 = CARTESIAN_POINT ( 'NONE',  ( 7.347880794884120722E-16, 1.826774720514426464, -6.000000000000000888 ) ) ;
#51816 = CARTESIAN_POINT ( 'NONE',  ( -121.6228709571500417, -24.65952944569305316, 1.056160979905705677 ) ) ;
#51817 = ORIENTED_EDGE ( 'NONE', *, *, #44583, .T. ) ;
#51818 = VERTEX_POINT ( 'NONE', #12858 ) ;
#51819 = ORIENTED_EDGE ( 'NONE', *, *, #75058, .F. ) ;
#51820 = CARTESIAN_POINT ( 'NONE',  ( -127.4336594584713538, -25.30053190447140921, 4.607786779764230012 ) ) ;
#51821 = CARTESIAN_POINT ( 'NONE',  ( -46.52287095715007581, -23.94994826722564696, -0.6494450866342706963 ) ) ;
#51822 = CARTESIAN_POINT ( 'NONE',  ( -119.5895376238167245, -23.48783264082479150, -1.443836473390058384 ) ) ;
#51823 = CARTESIAN_POINT ( 'NONE',  ( 12.91705851660734972, -16.24616318834520001, -1.500000000000002220 ) ) ;
#51824 = CARTESIAN_POINT ( 'NONE',  ( -20.56741719582323213, 7.008553436993695485, 11.49999999999999645 ) ) ;
#51825 = ORIENTED_EDGE ( 'NONE', *, *, #88413, .F. ) ;
#51826 = CARTESIAN_POINT ( 'NONE',  ( -40.14671197708927508, -25.19036671141680017, 3.332572802394528910 ) ) ;
#51827 = CARTESIAN_POINT ( 'NONE',  ( -41.62287095715006302, -29.50250786944525672, 11.44777988621624232 ) ) ;
#51828 = CARTESIAN_POINT ( 'NONE',  ( -115.5222181705558882, -23.48783264082477018, -1.443836473390087916 ) ) ;
#51829 = CARTESIAN_POINT ( 'NONE',  ( 1.585521478320181865, 22.38520322874704149, 11.49999999999998934 ) ) ;
#51830 = CARTESIAN_POINT ( 'NONE',  ( -51.02503725990638372, -25.31296715355957616, 4.507473421736313490 ) ) ;
#51831 = VERTEX_POINT ( 'NONE', #46194 ) ;
#51832 = CARTESIAN_POINT ( 'NONE',  ( -59.52287095715005449, -23.95044443724991723, 10.65354141964649592 ) ) ;
#51833 = CARTESIAN_POINT ( 'NONE',  ( -50.54482650861676518, -25.11141432701465703, 2.838324031928523894 ) ) ;
#51834 = EDGE_LOOP ( 'NONE', ( #31733, #46863, #84564, #18496 ) ) ;
#51835 = ORIENTED_EDGE ( 'NONE', *, *, #10579, .F. ) ;
#51836 = CARTESIAN_POINT ( 'NONE',  ( -99.35333152103353882, -25.28669466114246944, 5.843841316355384841 ) ) ;
#51837 = ORIENTED_EDGE ( 'NONE', *, *, #63163, .F. ) ;
#51838 = CARTESIAN_POINT ( 'NONE',  ( 18.63368790978032763, -10.32677859091227113, -1.500000000000002220 ) ) ;
#51839 = ORIENTED_EDGE ( 'NONE', *, *, #16723, .T. ) ;
#51840 = CARTESIAN_POINT ( 'NONE',  ( -6.377963355984652694, -5.876774720514412742, 19.53740760792478426 ) ) ;
#51841 = CARTESIAN_POINT ( 'NONE',  ( 21.07893183998518438, -5.767110019903106455, 11.49999999999998934 ) ) ;
#51842 = PLANE ( 'NONE',  #20594 ) ;
#51843 = CARTESIAN_POINT ( 'NONE',  ( 22.16846167567618053, -4.910139430472912458, 11.49999999999998934 ) ) ;
#51844 = EDGE_CURVE ( 'NONE', #57584, #23928, #25088, .T. ) ;
#51845 = CARTESIAN_POINT ( 'NONE',  ( -41.17181748269097596, -25.28892478857502368, 3.555109730339158336 ) ) ;
#51846 = LINE ( 'NONE', #68561, #59609 ) ;
#51847 = CARTESIAN_POINT ( 'NONE',  ( -21.91604229967229500, -0.6759211909499470705, -1.500000000000002220 ) ) ;
#51848 = DIRECTION ( 'NONE',  ( 0.000000000000000000, 1.000000000000000000, -8.673617379884035472E-16 ) ) ;
#51849 = ORIENTED_EDGE ( 'NONE', *, *, #40103, .F. ) ;
#51850 = CARTESIAN_POINT ( 'NONE',  ( -122.5900848267528289, -24.15620529776629510, 10.23563542870659582 ) ) ;
#51851 = EDGE_CURVE ( 'NONE', #68549, #48682, #31537, .T. ) ;
#51853 = ORIENTED_EDGE ( 'NONE', *, *, #98598, .F. ) ;
#51852 = EDGE_CURVE ( 'NONE', #99333, #58343, #92359, .T. ) ;
#51854 = CARTESIAN_POINT ( 'NONE',  ( -116.6228709571499991, -24.33832256527049154, 0.1851278514138666176 ) ) ;
#51855 = ADVANCED_FACE ( 'NONE', ( #39076 ), #23268, .T. ) ;
#51856 = CARTESIAN_POINT ( 'NONE',  ( -39.62287095715004881, -23.48783264082477373, -1.443836473390072594 ) ) ;
#51857 = CARTESIAN_POINT ( 'NONE',  ( -20.44305909758882933, -23.48154892321408482, 0.04347934593173589934 ) ) ;
#51858 = CARTESIAN_POINT ( 'NONE',  ( -15.93125441714207646, -14.09135727244061265, -1.500000000000002220 ) ) ;
#51859 = DIRECTION ( 'NONE',  ( 0.000000000000000000, -1.000000000000000000, 0.000000000000000000 ) ) ;
#51860 = EDGE_CURVE ( 'NONE', #87031, #49847, #76704, .T. ) ;
#51861 = DIRECTION ( 'NONE',  ( -3.017716325409535726E-14, 0.000000000000000000, -1.000000000000000000 ) ) ;
#51862 = CIRCLE ( 'NONE', #27527, 19.00000000000000355 ) ;
#51863 = CARTESIAN_POINT ( 'NONE',  ( -85.55841925135938197, -23.85016227208579664, -0.8807180028928368598 ) ) ;
#51864 = CARTESIAN_POINT ( 'NONE',  ( -33.53809244281052315, -24.34968618360933235, 0.1864209137778845560 ) ) ;
#51865 = CARTESIAN_POINT ( 'NONE',  ( -44.62287095715005592, -23.72773821059535848, 11.05748984161097503 ) ) ;
#51866 = ORIENTED_EDGE ( 'NONE', *, *, #21085, .T. ) ;
#51867 = CARTESIAN_POINT ( 'NONE',  ( -19.30006219055749739, -3.230038287793697283, 11.49999999999999645 ) ) ;
#51868 = CARTESIAN_POINT ( 'NONE',  ( -58.62287095715002749, -23.96177878511307568, 10.65340807706330573 ) ) ;
#51869 = AXIS2_PLACEMENT_3D ( 'NONE', #4643, #80768, #11250 ) ;
#51870 = CARTESIAN_POINT ( 'NONE',  ( 10.57556460110582996, 0.7139560615726621151, -8.999999999999994671 ) ) ;
#51871 = EDGE_CURVE ( 'NONE', #87632, #88641, #70620, .T. ) ;
#51872 = VERTEX_POINT ( 'NONE', #79137 ) ;
#51873 = FACE_OUTER_BOUND ( 'NONE', #36082, .T. ) ;
#51874 = CARTESIAN_POINT ( 'NONE',  ( -101.8264017983208021, -25.18997244373181843, 6.677177547450886763 ) ) ;
#51875 = VECTOR ( 'NONE', #55353, 1000.000000000000114 ) ;
#51876 = CARTESIAN_POINT ( 'NONE',  ( -122.5895376238167245, -23.47593901973091235, -1.443836447538997536 ) ) ;
#51877 = CARTESIAN_POINT ( 'NONE',  ( -45.62287095715005592, -23.84047902841603062, -0.8780736468305723186 ) ) ;
#51878 = CARTESIAN_POINT ( 'NONE',  ( -16.18664964019209052, -11.25563402961023662, 11.49999999999998934 ) ) ;
#51879 = VECTOR ( 'NONE', #4930, 1000.000000000000114 ) ;
#51880 = ORIENTED_EDGE ( 'NONE', *, *, #30058, .T. ) ;
#51881 = AXIS2_PLACEMENT_3D ( 'NONE', #79355, #71256, #80869 ) ;
#51882 = CARTESIAN_POINT ( 'NONE',  ( -24.90875734969025501, -5.965225279485572685, 30.00402280011862288 ) ) ;
#51883 = CARTESIAN_POINT ( 'NONE',  ( 30.60113388085891017, -4.386958714992013952, 26.76092701747204927 ) ) ;
#51884 = AXIS2_PLACEMENT_3D ( 'NONE', #39736, #41252, #1186 ) ;
#51885 = SECURITY_CLASSIFICATION_LEVEL ( 'unclassified' ) ;
#51886 = VERTEX_POINT ( 'NONE', #32469 ) ;
#51887 = CARTESIAN_POINT ( 'NONE',  ( 8.197725756732245017, -0.4963810196290943111, 3.727086380289611700 ) ) ;
#51888 = CARTESIAN_POINT ( 'NONE',  ( 22.33191539159816585, -3.407774720514426647, -16.26852658953824360 ) ) ;
#51889 = CARTESIAN_POINT ( 'NONE',  ( -55.61923018639313199, -23.48783264082475952, -1.443836473390099462 ) ) ;
#51890 = CARTESIAN_POINT ( 'NONE',  ( -63.52287095715004739, -23.47593901973090169, -1.443836447538996870 ) ) ;
#51891 = CARTESIAN_POINT ( 'NONE',  ( -6.989144439031651501, -6.376774720514410077, 19.51167604195716621 ) ) ;
#51892 = B_SPLINE_CURVE_WITH_KNOTS ( 'NONE', 3,
 ( #88613, #3887, #40934, #65796 ),
 .UNSPECIFIED., .F., .F.,
 ( 4, 4 ),
 ( 0.000000000000000000, 9.999999999998206125E-05 ),
 .UNSPECIFIED. ) ;
#51893 = CARTESIAN_POINT ( 'NONE',  ( -70.25652273905276957, -25.24515042782171648, 5.316157094516560377 ) ) ;
#51894 = CARTESIAN_POINT ( 'NONE',  ( -71.52287095715006160, -23.47593901973090169, -1.443836447538996870 ) ) ;
#51895 = CARTESIAN_POINT ( 'NONE',  ( -3.050325703546597822, 19.74810961616558913, 11.49999999999998934 ) ) ;
#51896 = LINE ( 'NONE', #19929, #41838 ) ;
#51897 = CARTESIAN_POINT ( 'NONE',  ( -23.29179552176161749, -5.965225279485594001, -17.29637630388738501 ) ) ;
#51898 = ORIENTED_EDGE ( 'NONE', *, *, #79548, .F. ) ;
#51899 = CARTESIAN_POINT ( 'NONE',  ( -63.52287095715006160, -24.33832256527048798, 0.1851278514138573750 ) ) ;
#51900 = CARTESIAN_POINT ( 'NONE',  ( 4.653494883475234545, -6.376774720514415407, 20.13747874360300116 ) ) ;
#51901 = ADVANCED_FACE ( 'NONE', ( #31970 ), #17746, .T. ) ;
#51902 = CARTESIAN_POINT ( 'NONE',  ( -66.52287095715007581, -23.96127896941631974, -0.6493128931038036900 ) ) ;
#51903 = CARTESIAN_POINT ( 'NONE',  ( -66.62287095715005592, -24.65952944569304606, 1.056160979905696573 ) ) ;
#51904 = CARTESIAN_POINT ( 'NONE',  ( -8.499999999999987566, 18.99999999999977973, 2.100000000000000089 ) ) ;
#51905 = CARTESIAN_POINT ( 'NONE',  ( -39.52202227182803540, -23.48783264082476308, -1.443836473390098352 ) ) ;
#51906 = EDGE_CURVE ( 'NONE', #30329, #63299, #49217, .T. ) ;
#51907 = CARTESIAN_POINT ( 'NONE',  ( -28.41293738586069040, -25.26026315677608380, 1.764151969445674428 ) ) ;
#51908 = CARTESIAN_POINT ( 'NONE',  ( -51.04357394935764347, -25.31574462869783204, 4.940877928535408969 ) ) ;
#51909 = ORIENTED_EDGE ( 'NONE', *, *, #64051, .F. ) ;
#51910 = CARTESIAN_POINT ( 'NONE',  ( -2.369893591381136755, -5.876774720514410966, 19.15221817653405623 ) ) ;
#51911 = CARTESIAN_POINT ( 'NONE',  ( -127.5217006469362673, -23.96119346886880663, -0.6495511937832001426 ) ) ;
#51912 = ORIENTED_EDGE ( 'NONE', *, *, #72683, .F. ) ;
#51913 = CARTESIAN_POINT ( 'NONE',  ( -20.21730713243277933, 1.494317884549376974, -1.500000000000002220 ) ) ;
#51914 = LINE ( 'NONE', #83843, #37104 ) ;
#51915 = CARTESIAN_POINT ( 'NONE',  ( -98.89303308397306580, -25.26498937201382233, 6.110950154240443410 ) ) ;
#51916 = CARTESIAN_POINT ( 'NONE',  ( 14.76093561896379214, -3.316774720514426456, -28.39148769130088468 ) ) ;
#51917 = ORIENTED_EDGE ( 'NONE', *, *, #80387, .F. ) ;
#51918 = CARTESIAN_POINT ( 'NONE',  ( -77.52287095715007581, -23.72773821059536914, 11.05748984161097326 ) ) ;
#51919 = CARTESIAN_POINT ( 'NONE',  ( -46.52287095715005449, -24.50321055353803956, 9.387540953477520489 ) ) ;
#51920 = CARTESIAN_POINT ( 'NONE',  ( -9.072532997253766496, -17.89392090870456542, -1.500000000000002220 ) ) ;
#51921 = CARTESIAN_POINT ( 'NONE',  ( 8.398332666215036824, -19.25654272332048578, 11.49999999999999645 ) ) ;
#51922 = CARTESIAN_POINT ( 'NONE',  ( -28.60093854151381265, -24.95576419111307231, 7.235735347421135444 ) ) ;
#51923 = CARTESIAN_POINT ( 'NONE',  ( -24.90875734969025501, 5.965225279485572685, 26.43402280011862615 ) ) ;
#51924 = CARTESIAN_POINT ( 'NONE',  ( -22.07534667767119174, -0.2742745133902674826, 11.49999999999998934 ) ) ;
#51926 = CARTESIAN_POINT ( 'NONE',  ( 19.18951349294833264, 7.196795126939715459, -1.500000000000002220 ) ) ;
#51925 = CC_DESIGN_PERSON_AND_ORGANIZATION_ASSIGNMENT ( #45516, #47511, ( #79677 ) ) ;
#51927 = CARTESIAN_POINT ( 'NONE',  ( -93.58953762381673869, -23.47596703998600631, 11.44779298504227683 ) ) ;
#51928 = CARTESIAN_POINT ( 'NONE',  ( 21.57151214508649772, -9.529487854913506695, 1.500000000000000666 ) ) ;
#51929 = CARTESIAN_POINT ( 'NONE',  ( 1.437548984227666304, -5.319565594357255733, 0.000000000000000000 ) ) ;
#51930 = ORIENTED_EDGE ( 'NONE', *, *, #52595, .T. ) ;
#51931 = PLANE ( 'NONE',  #44593 ) ;
#51932 = CARTESIAN_POINT ( 'NONE',  ( -31.63564585891770520, -24.34968618360933590, 0.1864209137778850556 ) ) ;
#51933 = ORIENTED_EDGE ( 'NONE', *, *, #47565, .F. ) ;
#51934 = ORIENTED_EDGE ( 'NONE', *, *, #31794, .T. ) ;
#51935 = CARTESIAN_POINT ( 'NONE',  ( -55.52287095715005449, -23.48783264082477018, -1.443836473390094577 ) ) ;
#51936 = CARTESIAN_POINT ( 'NONE',  ( -100.4498239493576648, -25.04307398257883932, 7.563174194274490780 ) ) ;
#51937 = CARTESIAN_POINT ( 'NONE',  ( -76.54602688947991851, -24.34968618360934300, 0.1864209137778858327 ) ) ;
#51938 = CARTESIAN_POINT ( 'NONE',  ( -13.12974562303265813, -15.89414520977026513, -1.500000000000002220 ) ) ;
#51939 = CARTESIAN_POINT ( 'NONE',  ( -14.38888013576714719, -16.06800976983558726, 11.49999999999999645 ) ) ;
#51940 = EDGE_LOOP ( 'NONE', ( #94243, #87853, #5019, #70084, #9129 ) ) ;
#51941 = CARTESIAN_POINT ( 'NONE',  ( -35.52287095715005449, -23.48783264083451883, -1.443836473374936258 ) ) ;
#51942 = CARTESIAN_POINT ( 'NONE',  ( 22.33191539159856731, -2.682774720514426559, -16.26852658953777109 ) ) ;
#51943 = CARTESIAN_POINT ( 'NONE',  ( 20.54922051473491607, -8.805037660420627077, -1.500000000000002220 ) ) ;
#51944 = CARTESIAN_POINT ( 'NONE',  ( -10.11875734969026297, -5.965225279485572685, 30.51402280011862089 ) ) ;
#51945 = CARTESIAN_POINT ( 'NONE',  ( -84.51017505570197841, -24.15543982623907482, -0.2315651400026630391 ) ) ;
#51946 = ORIENTED_EDGE ( 'NONE', *, *, #21897, .F. ) ;
#51947 = LINE ( 'NONE', #90007, #3138 ) ;
#51948 = AXIS2_PLACEMENT_3D ( 'NONE', #67840, #74918, #21627 ) ;
#51949 = CARTESIAN_POINT ( 'NONE',  ( 33.74607884027702909, 5.965225279485572685, -4.999864028243830916 ) ) ;
#51950 = B_SPLINE_CURVE_WITH_KNOTS ( 'NONE', 3,
 ( #87602, #39423, #18084, #31813 ),
 .UNSPECIFIED., .F., .F.,
 ( 4, 4 ),
 ( 0.000000000000000000, 1.000000000000000000 ),
 .UNSPECIFIED. ) ;
#51951 = AXIS2_PLACEMENT_3D ( 'NONE', #12733, #50324, #81260 ) ;
#51952 = CARTESIAN_POINT ( 'NONE',  ( -11.44352472427880052, 17.46665840655709090, 11.49999999999998934 ) ) ;
#51953 = ORIENTED_EDGE ( 'NONE', *, *, #74190, .T. ) ;
#51955 = ORIENTED_EDGE ( 'NONE', *, *, #20317, .F. ) ;
#51954 = CARTESIAN_POINT ( 'NONE',  ( -67.58777801654929362, -24.35071581493543746, 9.817618358456023486 ) ) ;
#51956 = VERTEX_POINT ( 'NONE', #10130 ) ;
#51957 = VECTOR ( 'NONE', #34520, 1000.000000000000000 ) ;
#51958 = CARTESIAN_POINT ( 'NONE',  ( -100.6412043750470104, -23.48786465467241413, 11.44779295918254469 ) ) ;
#51959 = CARTESIAN_POINT ( 'NONE',  ( 19.82261944725993175, 7.364942908566579405, -1.500000000000002220 ) ) ;
#51960 = ORIENTED_EDGE ( 'NONE', *, *, #94921, .T. ) ;
#51961 = CARTESIAN_POINT ( 'NONE',  ( -15.87499999999997868, 0.000000000000000000, 0.000000000000000000 ) ) ;
#51962 = CARTESIAN_POINT ( 'NONE',  ( -48.87558633688828991, -25.25869780337663784, 6.071246232422383926 ) ) ;
#51963 = CARTESIAN_POINT ( 'NONE',  ( -48.62287095715004881, -24.66019654487199020, 8.947790411086135265 ) ) ;
#51964 = DIRECTION ( 'NONE',  ( -2.352173255807804438E-16, 2.352173255807796056E-16, 1.000000000000000000 ) ) ;
#51965 = CARTESIAN_POINT ( 'NONE',  ( -38.52287095715006870, -23.48786465467241058, 11.44779295918255180 ) ) ;
#51966 = CARTESIAN_POINT ( 'NONE',  ( 5.219777686717518961, -21.12652377152128480, -1.500000000000002220 ) ) ;
#51967 = CARTESIAN_POINT ( 'NONE',  ( -31.24388727629347784, -24.87479601683088148, 8.247789944647559324 ) ) ;
#51968 = EDGE_CURVE ( 'NONE', #61101, #45280, #60926, .T. ) ;
#51970 = VERTEX_POINT ( 'NONE', #16736 ) ;
#51969 = CARTESIAN_POINT ( 'NONE',  ( -1.228339276683141579, -22.28195500894762660, 11.49999999999999645 ) ) ;
#51971 = FACE_OUTER_BOUND ( 'NONE', #33755, .T. ) ;
#51972 = FACE_OUTER_BOUND ( 'NONE', #5357, .T. ) ;
#51973 = DIRECTION ( 'NONE',  ( 0.000000000000000000, 0.000000000000000000, -1.000000000000000000 ) ) ;
#51974 = ORIENTED_EDGE ( 'NONE', *, *, #67611, .T. ) ;
#51975 = ORIENTED_EDGE ( 'NONE', *, *, #68857, .T. ) ;
#51976 = VERTEX_POINT ( 'NONE', #41598 ) ;
#51977 = EDGE_CURVE ( 'NONE', #14722, #36363, #47703, .T. ) ;
#51978 = DIRECTION ( 'NONE',  ( 0.1478094111296165969, -0.9890158633619159367, 0.000000000000000000 ) ) ;
#51979 = CARTESIAN_POINT ( 'NONE',  ( -127.9228709571500531, -23.47593901973090524, -1.443836447538996204 ) ) ;
#51980 = EDGE_CURVE ( 'NONE', #84981, #60030, #49716, .T. ) ;
#51981 = CARTESIAN_POINT ( 'NONE',  ( 30.61558003201036726, -3.638743767327229151, 27.34189434213806535 ) ) ;
#51982 = CARTESIAN_POINT ( 'NONE',  ( -49.57059674196057841, -25.31466356504994053, 4.840235729264941611 ) ) ;
#51983 = CARTESIAN_POINT ( 'NONE',  ( -5.843762028675351772, -18.45606589188993141, -1.500000000000002220 ) ) ;
#51984 = CARTESIAN_POINT ( 'NONE',  ( -36.55620429048340014, -24.66019654487199020, 8.947790411086138818 ) ) ;
#51985 = EDGE_LOOP ( 'NONE', ( #1022, #96961, #56563, #24139 ) ) ;
#51986 = CARTESIAN_POINT ( 'NONE',  ( 18.67713048845720181, -5.233370074711279685, 11.49999999999999645 ) ) ;
#51987 = CARTESIAN_POINT ( 'NONE',  ( -30.47287095715007510, -23.47594215783195537, -5.102550391006585557E-05 ) ) ;
#51988 = EDGE_CURVE ( 'NONE', #39987, #29613, #93862, .T. ) ;
#51989 = ORIENTED_EDGE ( 'NONE', *, *, #92176, .F. ) ;
#51990 = CARTESIAN_POINT ( 'NONE',  ( -6.914873625533457968, -6.376774720514426953, 29.95171384920748281 ) ) ;
#51991 = CARTESIAN_POINT ( 'NONE',  ( -29.52287095715006160, -29.50250243563707286, 8.947779751028683393 ) ) ;
#51992 = DIRECTION ( 'NONE',  ( 0.000000000000000000, 0.000000000000000000, -1.000000000000000000 ) ) ;
#51993 = CARTESIAN_POINT ( 'NONE',  ( -63.93899109588087271, -24.04668586515358797, 10.47594215909545312 ) ) ;
#51994 = CARTESIAN_POINT ( 'NONE',  ( 2.166912399371504705, 19.51343182558466793, 11.49999999999998934 ) ) ;
#51995 = CARTESIAN_POINT ( 'NONE',  ( 7.089543269230769162, -6.376774720514413630, 19.75741185897435415 ) ) ;
#51996 = VERTEX_POINT ( 'NONE', #78620 ) ;
#51997 = CARTESIAN_POINT ( 'NONE',  ( -21.33164055427280914, -3.227942221655450972, -1.500000000000002220 ) ) ;
#51998 = CARTESIAN_POINT ( 'NONE',  ( -33.47773199953535084, -24.66019654487198665, 8.947790411086133489 ) ) ;
#51999 = CARTESIAN_POINT ( 'NONE',  ( -70.35718658181241381, -25.25639601273455526, 7.100646501951180412 ) ) ;
#52001 = B_SPLINE_CURVE_WITH_KNOTS ( 'NONE', 3,
 ( #19442, #72248, #2740, #41806 ),
 .UNSPECIFIED., .F., .F.,
 ( 4, 4 ),
 ( 0.06983579250763341517, 0.07884222377974890728 ),
 .UNSPECIFIED. ) ;
#52000 = DIRECTION ( 'NONE',  ( 0.000000000000000000, 1.000000000000000000, 0.000000000000000000 ) ) ;
#52002 = AXIS2_PLACEMENT_3D ( 'NONE', #50581, #94748, #11020 ) ;
#52003 = CARTESIAN_POINT ( 'NONE',  ( -72.62287095715005592, -29.50250243563736774, 8.947779886222143375 ) ) ;
#52004 = CARTESIAN_POINT ( 'NONE',  ( 18.09022303007301247, 14.20294132079179938, -1.500000000000002220 ) ) ;
#52005 = PERSON_AND_ORGANIZATION ( #70597, #27821 ) ;
#52006 = DIRECTION ( 'NONE',  ( 0.9994733861282923959, 0.000000000000000000, 0.03244919754393515293 ) ) ;
#52007 = CARTESIAN_POINT ( 'NONE',  ( -50.09975158262200523, -25.30285855287542773, 4.744951912546983230 ) ) ;
#52008 = CARTESIAN_POINT ( 'NONE',  ( -11.28321777122536140, 16.66956161807075887, 11.49999999999999645 ) ) ;
#52009 = CARTESIAN_POINT ( 'NONE',  ( -109.3293036055952143, -25.28814155227650318, 3.229614981432298304 ) ) ;
#52010 = DIRECTION ( 'NONE',  ( -0.000000000000000000, -0.000000000000000000, -1.000000000000000000 ) ) ;
#52011 = CARTESIAN_POINT ( 'NONE',  ( 9.843544857143434967, -6.475225279485573360, -27.49819965379373343 ) ) ;
#52012 = CARTESIAN_POINT ( 'NONE',  ( -29.49875734969025842, 0.3587747205144265483, 17.86602280011862476 ) ) ;
#52013 = DIRECTION ( 'NONE',  ( 0.000000000000000000, 0.000000000000000000, 1.000000000000000000 ) ) ;
#52014 = EDGE_CURVE ( 'NONE', #66289, #38454, #81598, .T. ) ;
#52015 = CARTESIAN_POINT ( 'NONE',  ( 13.99221305778824487, -14.08248706038611964, 11.49999999999998934 ) ) ;
#52016 = CARTESIAN_POINT ( 'NONE',  ( -113.5569085991196090, -23.73766607897670866, -1.055555164236448240 ) ) ;
#52017 = CARTESIAN_POINT ( 'NONE',  ( 1.028332004353105233, 19.75660188889424518, -1.500000000000002220 ) ) ;
#52018 = CARTESIAN_POINT ( 'NONE',  ( -126.5547688801620438, -24.66019654487200796, 8.947790411086103290 ) ) ;
#52019 = ADVANCED_FACE ( 'NONE', ( #24355 ), #70533, .T. ) ;
#52021 = AXIS2_PLACEMENT_3D ( 'NONE', #21155, #36891, #74454 ) ;
#52020 = DESIGN_CONTEXT ( 'detailed design', #47893, 'design' ) ;
#52022 = CARTESIAN_POINT ( 'NONE',  ( -0.8502773128684013582, -6.376774720514413630, 19.61227901093089798 ) ) ;
#52023 = DIRECTION ( 'NONE',  ( 0.000000000000000000, -1.000000000000000000, 0.000000000000000000 ) ) ;
#52024 = CARTESIAN_POINT ( 'NONE',  ( 18.07348078632662691, -10.09602009226539288, 11.49999999999999645 ) ) ;
#52025 = DIRECTION ( 'NONE',  ( 0.000000000000000000, -1.000000000000000000, 0.000000000000000000 ) ) ;
#52026 = CARTESIAN_POINT ( 'NONE',  ( 31.13513474936813807, 5.356774720514427379, 3.331262582247329185 ) ) ;
#52027 = CARTESIAN_POINT ( 'NONE',  ( -50.15966858932511485, -25.25138676263039983, 5.214258431718429065 ) ) ;
#52029 = EDGE_CURVE ( 'NONE', #10158, #76180, #41710, .T. ) ;
#52028 = CARTESIAN_POINT ( 'NONE',  ( 11.07647423179810531, -19.82844882884714366, 11.49999999999999645 ) ) ;
#52030 = ORIENTED_EDGE ( 'NONE', *, *, #51559, .T. ) ;
#52031 = CARTESIAN_POINT ( 'NONE',  ( -78.52287095715006160, -24.65952944569304606, 1.056160979905698794 ) ) ;
#52032 = CARTESIAN_POINT ( 'NONE',  ( -33.55620429048339304, -24.66019654487199020, 8.947790411086137041 ) ) ;
#52033 = CARTESIAN_POINT ( 'NONE',  ( 8.071512145086503054, -0.8690767389352458405, -3.741933809627420171 ) ) ;
#52034 = DIRECTION ( 'NONE',  ( -1.000000000000000000, -0.000000000000000000, -0.000000000000000000 ) ) ;
#52035 = EDGE_LOOP ( 'NONE', ( #85413, #69044, #85893, #41443, #1057, #59281, #1375 ) ) ;
#52036 = B_SPLINE_CURVE_WITH_KNOTS ( 'NONE', 3,
 ( #80320, #41780, #96541, #72720 ),
 .UNSPECIFIED., .F., .F.,
 ( 4, 4 ),
 ( 0.000000000000000000, 1.000000000000000000 ),
 .UNSPECIFIED. ) ;
#52037 = ORIENTED_EDGE ( 'NONE', *, *, #26586, .T. ) ;
#52038 = CARTESIAN_POINT ( 'NONE',  ( -100.3036073397659322, -25.12344534561801268, 7.099021671109709608 ) ) ;
#52039 = CARTESIAN_POINT ( 'NONE',  ( 17.53461989915211916, -14.66684187699354425, -1.500000000000002220 ) ) ;
#52040 = CARTESIAN_POINT ( 'NONE',  ( -29.62954789768681962, -24.43759654968573614, 0.6176547996449982536 ) ) ;
#52041 = CARTESIAN_POINT ( 'NONE',  ( 13.05104812959431548, -17.15854754814989391, -1.500000000000002220 ) ) ;
#52042 = CARTESIAN_POINT ( 'NONE',  ( 31.04236049493789906, -6.475225279485573360, 19.84760796525321780 ) ) ;
#52043 = CARTESIAN_POINT ( 'NONE',  ( -115.5562042904833930, -24.99156044556202616, 7.747789690856173195 ) ) ;
#52044 = CARTESIAN_POINT ( 'NONE',  ( -16.99934442671578694, -14.85117937636706031, 11.49999999999999645 ) ) ;
#52045 = EDGE_LOOP ( 'NONE', ( #32922, #51849, #71298, #4681 ) ) ;
#52046 = CARTESIAN_POINT ( 'NONE',  ( -70.00627666057835086, -25.24754250677208134, 4.873906482351993752 ) ) ;
#52047 = CARTESIAN_POINT ( 'NONE',  ( 16.65356921002588919, 14.36988287374134821, -1.500000000000002220 ) ) ;
#52048 = EDGE_CURVE ( 'NONE', #5456, #12501, #13819, .T. ) ;
#52049 = CARTESIAN_POINT ( 'NONE',  ( -105.6293760709154128, -24.40133493613049964, 9.663955038902797057 ) ) ;
#52050 = CARTESIAN_POINT ( 'NONE',  ( -28.88518304243395818, -25.21724837498792127, 6.883446113543877587 ) ) ;
#52051 = VERTEX_POINT ( 'NONE', #87764 ) ;
#52052 = LINE ( 'NONE', #20092, #62213 ) ;
#52053 = CARTESIAN_POINT ( 'NONE',  ( -116.6228709571500559, -29.50250243563736774, 8.947779886222134493 ) ) ;
#52054 = B_SPLINE_CURVE_WITH_KNOTS ( 'NONE', 3,
 ( #100387, #9065, #16174, #48144 ),
 .UNSPECIFIED., .F., .F.,
 ( 4, 4 ),
 ( 0.8193651591418213975, 0.8203659061825868681 ),
 .UNSPECIFIED. ) ;
#52055 = ORIENTED_EDGE ( 'NONE', *, *, #97587, .T. ) ;
#52056 = CARTESIAN_POINT ( 'NONE',  ( -116.5228709571500616, -24.65952944569305316, 1.056160979905705899 ) ) ;
#52057 = EDGE_CURVE ( 'NONE', #30457, #83907, #75459, .T. ) ;
#52058 = VERTEX_POINT ( 'NONE', #63444 ) ;
#52059 = B_SPLINE_CURVE_WITH_KNOTS ( 'NONE', 3,
 ( #85769, #32992, #63966, #94874, #25367, #56344, #8650, #9140, #86268, #8151, #87265, #23350, #54333, #17762, #31480, #85259, #48730, #1035, #39593, #31983, #79648, #10147, #72064, #15752, #62441, #30977, #46716 ),
 .UNSPECIFIED., .F., .F.,
 ( 4, 1, 1, 1, 1, 1, 1, 1, 1, 1, 1, 1, 1, 1, 1, 1, 1, 1, 1, 1, 1, 1, 1, 1, 4 ),
 ( 0.000000000000000000, 0.03378714634699089836, 0.06662165772429383404, 0.09928487809597265346, 0.1313611650426506072, 0.1635851875953436008, 0.1961039269870681889, 0.2289022543238170004, 0.2621580559050075143, 0.2959912222583161445, 0.3302178457247997301, 0.3650598258919544037, 0.4009507373401082209, 0.4376203820767376462, 0.4757075294370921026, 0.5153806916250490699, 0.5564135414931649093, 0.5997648298727309424, 0.6464241555840876119, 0.6964314445175666668, 0.7497815178015586612, 0.8065733069755320894, 0.8674355315653994314, 0.9318867532508745555, 1.000000000000000000 ),
 .UNSPECIFIED. ) ;
#52060 = EDGE_LOOP ( 'NONE', ( #35734, #63591 ) ) ;
#52061 = DIRECTION ( 'NONE',  ( -0.000000000000000000, -1.000000000000000000, -0.000000000000000000 ) ) ;
#52062 = CARTESIAN_POINT ( 'NONE',  ( -71.92287095715006728, -23.47596703998600631, 11.44779298504227860 ) ) ;
#52063 = CARTESIAN_POINT ( 'NONE',  ( -57.54804246586016347, -24.15543982623907127, -0.2315651400026663420 ) ) ;
#52064 = CARTESIAN_POINT ( 'NONE',  ( -8.052747710315523832, 18.77774781879659116, -1.500000000000002220 ) ) ;
#52065 = VERTEX_POINT ( 'NONE', #33971 ) ;
#52066 = CARTESIAN_POINT ( 'NONE',  ( -2.959136224476847765, -5.876774720514412742, 19.53857357749110335 ) ) ;
#52067 = ADVANCED_FACE ( 'NONE', ( #33465 ), #26361, .T. ) ;
#52068 = CARTESIAN_POINT ( 'NONE',  ( -30.59167141582165428, -24.92410949913932683, 1.600845668900849672 ) ) ;
#52069 = EDGE_CURVE ( 'NONE', #76858, #95755, #83917, .T. ) ;
#52070 = CARTESIAN_POINT ( 'NONE',  ( -54.52287095715005449, -23.48783264082476308, -1.443836473390096797 ) ) ;
#52071 = DIRECTION ( 'NONE',  ( 0.000000000000000000, 0.000000000000000000, -1.000000000000000000 ) ) ;
#52072 = ORIENTED_EDGE ( 'NONE', *, *, #39530, .T. ) ;
#52073 = CARTESIAN_POINT ( 'NONE',  ( -49.62287095715004170, -23.47596703998600631, 11.44779298504227505 ) ) ;
#52074 = CARTESIAN_POINT ( 'NONE',  ( -102.6228709571500559, -29.50247984919015209, -1.443849546365050029 ) ) ;
#52075 = ADVANCED_FACE ( 'NONE', ( #57827 ), #74528, .F. ) ;
#52076 = CARTESIAN_POINT ( 'NONE',  ( 11.01739540223112357, 17.63107602209319680, 11.49999999999998934 ) ) ;
#52077 = AXIS2_PLACEMENT_3D ( 'NONE', #76302, #29643, #91538 ) ;
#52078 = VERTEX_POINT ( 'NONE', #80648 ) ;
#52080 = EDGE_LOOP ( 'NONE', ( #39293, #27120, #52379, #16333 ) ) ;
#52079 = DIRECTION ( 'NONE',  ( -3.773278334444166432E-23, 1.000000000000000000, 0.000000000000000000 ) ) ;
#52081 = DIRECTION ( 'NONE',  ( -3.773278334453079030E-23, 0.9999999999976377785, 2.173523156925979128E-06 ) ) ;
#52082 = VERTEX_POINT ( 'NONE', #88769 ) ;
#52083 = ORIENTED_EDGE ( 'NONE', *, *, #71219, .F. ) ;
#52084 = DIRECTION ( 'NONE',  ( -3.773278334444167608E-23, 1.000000000000000000, 0.000000000000000000 ) ) ;
#52085 = CARTESIAN_POINT ( 'NONE',  ( -76.52287095715011844, -23.95044443724992789, 10.65354141964649415 ) ) ;
#52086 = CARTESIAN_POINT ( 'NONE',  ( -60.55620429048339304, -23.48786465467241058, 11.44779295918254824 ) ) ;
#52087 = FACE_OUTER_BOUND ( 'NONE', #31706, .T. ) ;
#52088 = EDGE_CURVE ( 'NONE', #80349, #58159, #65620, .T. ) ;
#52090 = VERTEX_POINT ( 'NONE', #20232 ) ;
#52089 = CARTESIAN_POINT ( 'NONE',  ( -20.57447749561850969, 8.151157241358404804, 11.49999999999999645 ) ) ;
#52091 = CARTESIAN_POINT ( 'NONE',  ( -2.701720430790308214, -0.3587747205144061202, -28.90526747363640681 ) ) ;
#52092 = CARTESIAN_POINT ( 'NONE',  ( 20.48348528492645571, -9.684159049092739835, -1.500000000000002220 ) ) ;
#52094 = EDGE_LOOP ( 'NONE', ( #54433, #73434, #18021, #71607 ) ) ;
#52093 = FACE_OUTER_BOUND ( 'NONE', #63738, .T. ) ;
#52095 = AXIS2_PLACEMENT_3D ( 'NONE', #10690, #64004, #41651 ) ;
#52096 = EDGE_LOOP ( 'NONE', ( #22825, #78650, #88621, #80376, #78277, #32812, #9275, #4031, #83180, #8905, #4059, #55448 ) ) ;
#52097 =( GEOMETRIC_REPRESENTATION_CONTEXT ( 3 ) GLOBAL_UNCERTAINTY_ASSIGNED_CONTEXT ( ( #15434 ) ) GLOBAL_UNIT_ASSIGNED_CONTEXT ( ( #34402, #89684, #29276 ) ) REPRESENTATION_CONTEXT ( 'NONE', 'WORKASPACE' ) );
#52098 = DIRECTION ( 'NONE',  ( 0.000000000000000000, 0.9999999999976377785, 2.173523156925979975E-06 ) ) ;
#52099 = B_SPLINE_CURVE_WITH_KNOTS ( 'NONE', 3,
 ( #17877, #80274, #10769, #88898 ),
 .UNSPECIFIED., .F., .F.,
 ( 4, 4 ),
 ( 0.000000000000000000, 9.999999999998897304E-05 ),
 .UNSPECIFIED. ) ;
#52100 = B_SPLINE_CURVE_WITH_KNOTS ( 'NONE', 3,
 ( #74692, #28033, #81817, #59990 ),
 .UNSPECIFIED., .F., .F.,
 ( 4, 4 ),
 ( 0.000000000000000000, 9.999999999998900014E-05 ),
 .UNSPECIFIED. ) ;
#52101 = EDGE_CURVE ( 'NONE', #19111, #71424, #39652, .T. ) ;
#52102 = CARTESIAN_POINT ( 'NONE',  ( -17.50950832565593984, 9.922426906265528146, 11.49999999999998934 ) ) ;
#52103 = EDGE_CURVE ( 'NONE', #40197, #45760, #33209, .T. ) ;
#52104 = DIRECTION ( 'NONE',  ( 0.000000000000000000, 1.000000000000000000, 0.000000000000000000 ) ) ;
#52105 = ORIENTED_EDGE ( 'NONE', *, *, #64730, .F. ) ;
#52106 = DIRECTION ( 'NONE',  ( -0.000000000000000000, 0.08715574274766166307, 0.9961946980917452121 ) ) ;
#52107 = CARTESIAN_POINT ( 'NONE',  ( -12.31279356157217109, -18.55646752483835016, -1.500000000000002220 ) ) ;
#52108 = EDGE_CURVE ( 'NONE', #34532, #33604, #72126, .T. ) ;
#52109 = ORIENTED_EDGE ( 'NONE', *, *, #87146, .F. ) ;
#52110 = FACE_OUTER_BOUND ( 'NONE', #99842, .T. ) ;
#52111 = CARTESIAN_POINT ( 'NONE',  ( -89.62287095715005592, -23.72773821059535848, 11.05748984161097681 ) ) ;
#52112 = CARTESIAN_POINT ( 'NONE',  ( -26.80500567364604336, -24.59566541176759813, 1.842733277147198923 ) ) ;
#52113 = EDGE_CURVE ( 'NONE', #63837, #78861, #51701, .T. ) ;
#52114 = PLANE ( 'NONE',  #51183 ) ;
#52115 = LINE ( 'NONE', #63744, #56933 ) ;
#52116 = ADVANCED_FACE ( 'NONE', ( #90754 ), #27855, .T. ) ;
#52117 = CARTESIAN_POINT ( 'NONE',  ( -11.52932745282126703, -15.74164922852205173, -1.500000000000002220 ) ) ;
#52118 = CARTESIAN_POINT ( 'NONE',  ( -15.31780299886000485, -15.04297462106122474, -1.500000000000002220 ) ) ;
#52119 = CARTESIAN_POINT ( 'NONE',  ( -2.373828433815573735, -6.376774720514410077, 19.48240003225459915 ) ) ;
#52120 = CARTESIAN_POINT ( 'NONE',  ( -46.55620429048339304, -23.47596703998600276, 11.44779298504227505 ) ) ;
#52121 = DIRECTION ( 'NONE',  ( -0.4771587602595987465, -0.8788171126619706008, 0.000000000000000000 ) ) ;
#52122 = CARTESIAN_POINT ( 'NONE',  ( -22.75767140345847750, 1.815691853630000629, -1.500000000000002220 ) ) ;
#52123 = AXIS2_PLACEMENT_3D ( 'NONE', #32739, #56094, #63722 ) ;
#52124 = PERSON_AND_ORGANIZATION ( #70597, #27821 ) ;
#52125 = FACE_OUTER_BOUND ( 'NONE', #38016, .T. ) ;
#52126 = CARTESIAN_POINT ( 'NONE',  ( -27.86046284349298219, 0.3587747205143967943, -8.091963836038763347 ) ) ;
#52127 = CARTESIAN_POINT ( 'NONE',  ( 18.82558416981596139, 6.732768832687442639, 11.49999999999999645 ) ) ;
#52128 = CARTESIAN_POINT ( 'NONE',  ( -50.52287095715005449, -24.63287334234177450, 0.9662140553045359681 ) ) ;
#52129 = CARTESIAN_POINT ( 'NONE',  ( -57.58953762381671737, -24.64898659630367916, 1.056161002820383610 ) ) ;
#52130 = CARTESIAN_POINT ( 'NONE',  ( 10.46399479596398052, -3.316774720514422903, -27.03001098546561209 ) ) ;
#52131 = EDGE_LOOP ( 'NONE', ( #18479, #10261, #79752, #40816, #83871, #51153, #33100, #8991, #81854, #15845, #11996, #9785, #1710, #21613, #14981, #3546, #37581, #56537, #46166, #1200 ) ) ;
#52132 = DIRECTION ( 'NONE',  ( -1.000000000000000000, -3.773278334444167608E-23, -8.201307833595939069E-29 ) ) ;
#52133 = DIRECTION ( 'NONE',  ( 3.773278334444167608E-23, -1.000000000000000000, 0.000000000000000000 ) ) ;
#52134 = CARTESIAN_POINT ( 'NONE',  ( -21.62197530259306788, 2.132803791230205359, -1.500000000000002220 ) ) ;
#52135 = PLANE ( 'NONE',  #33407 ) ;
#52136 = CARTESIAN_POINT ( 'NONE',  ( -7.889300446747370188, -17.95381117360125955, -1.500000000000002220 ) ) ;
#52137 = CARTESIAN_POINT ( 'NONE',  ( -100.1650658605970392, -25.13691562650546985, 7.079980769990460665 ) ) ;
#52138 = EDGE_LOOP ( 'NONE', ( #4793, #75229, #86647, #87142 ) ) ;
#52139 = CONTEXT_DEPENDENT_SHAPE_REPRESENTATION ( #99723, #49024 ) ;
#52140 = DIRECTION ( 'NONE',  ( 1.000000000000000000, 3.773278334444167608E-23, 8.201307833595939069E-29 ) ) ;
#52141 = CARTESIAN_POINT ( 'NONE',  ( -123.9228709571500531, -23.47596703998600631, 11.44779298504228038 ) ) ;
#52142 = CARTESIAN_POINT ( 'NONE',  ( -0.3173379506236611580, 20.48240526196808631, 11.49999999999999645 ) ) ;
#52143 = PLANE ( 'NONE',  #53831 ) ;
#52144 = VECTOR ( 'NONE', #39395, 1000.000000000000114 ) ;
#52145 = CARTESIAN_POINT ( 'NONE',  ( -113.5228709571501327, -24.66019654487200441, 8.947790411086112172 ) ) ;
#52146 = ORIENTED_EDGE ( 'NONE', *, *, #21678, .T. ) ;
#52147 = CARTESIAN_POINT ( 'NONE',  ( 31.24279708945211098, -4.510509370595455536, 1.827416827591516357 ) ) ;
#52148 = CARTESIAN_POINT ( 'NONE',  ( -40.35585260198725877, -25.28892422734320178, 3.296896784922714652 ) ) ;
#52149 = DIRECTION ( 'NONE',  ( 0.000000000000000000, -2.173523156925980399E-06, 0.9999999999976378895 ) ) ;
#52150 = CARTESIAN_POINT ( 'NONE',  ( -123.5228709571500474, -23.47593901973090524, -1.443836447538996204 ) ) ;
#52151 = EDGE_LOOP ( 'NONE', ( #18598, #12610, #80541, #94355 ) ) ;
#52152 = DIRECTION ( 'NONE',  ( 1.743630241030147080E-15, -6.974520964120588319E-15, 1.000000000000000000 ) ) ;
#52153 = AXIS2_PLACEMENT_3D ( 'NONE', #970, #68978, #53770 ) ;
#52154 = CARTESIAN_POINT ( 'NONE',  ( 1.550618966079767347, 22.99078241098900932, 11.49999999999999645 ) ) ;
#52155 = CARTESIAN_POINT ( 'NONE',  ( -15.20078144808659992, 16.97451310947862169, 11.49999999999998934 ) ) ;
#52156 = DIRECTION ( 'NONE',  ( -3.773278334453079030E-23, 0.9999999999976377785, 2.173523156925979128E-06 ) ) ;
#52157 = DIRECTION ( 'NONE',  ( -0.09721092304694051167, 0.000000000000000000, 0.9952638024365005887 ) ) ;
#52158 = CARTESIAN_POINT ( 'NONE',  ( -49.51604314152774577, -25.26360598679406166, 3.877879557975262070 ) ) ;
#52159 = APPROVAL_PERSON_ORGANIZATION ( #14793, #93371, #99522 ) ;
#52160 = CARTESIAN_POINT ( 'NONE',  ( -106.5228709571500758, -29.50247984919015209, -1.443849546365048253 ) ) ;
#52161 = FACE_OUTER_BOUND ( 'NONE', #4667, .T. ) ;
#52162 = CARTESIAN_POINT ( 'NONE',  ( 19.94191871449930531, -9.063712221575384476, 11.49999999999998934 ) ) ;
#52163 = CARTESIAN_POINT ( 'NONE',  ( 7.267403311989051318, -5.876774720514425177, 21.43157132964656952 ) ) ;
#52164 = EDGE_CURVE ( 'NONE', #38058, #45825, #62412, .T. ) ;
#52165 = CARTESIAN_POINT ( 'NONE',  ( -87.51796210385577979, -23.73791477778911840, 11.05961554403170588 ) ) ;
#52166 = FACE_OUTER_BOUND ( 'NONE', #71949, .T. ) ;
#52167 = LINE ( 'NONE', #44053, #78403 ) ;
#52168 = CARTESIAN_POINT ( 'NONE',  ( -112.6228709571501270, -23.94994826722516379, -0.6494450866351680896 ) ) ;
#52169 = CARTESIAN_POINT ( 'NONE',  ( -4.169309590939843879, -5.876774720514412742, 19.59793130852656518 ) ) ;
#52170 = ORIENTED_EDGE ( 'NONE', *, *, #92605, .F. ) ;
#52171 = CARTESIAN_POINT ( 'NONE',  ( 19.09590870110849181, 7.302211495713927469, -1.500000000000002220 ) ) ;
#52172 = ORIENTED_EDGE ( 'NONE', *, *, #27112, .F. ) ;
#52173 = EDGE_LOOP ( 'NONE', ( #62207, #98737, #66869, #82273 ) ) ;
#52174 = ORIENTED_EDGE ( 'NONE', *, *, #6221, .T. ) ;
#52175 = VERTEX_POINT ( 'NONE', #96370 ) ;
#52176 = CARTESIAN_POINT ( 'NONE',  ( 1.550618966079767347, 22.99078241098900932, 11.49999999999998934 ) ) ;
#52177 = CARTESIAN_POINT ( 'NONE',  ( -61.64237931368420220, -23.96119346886880308, -0.6495511937832122440 ) ) ;
#52178 = B_SPLINE_CURVE_WITH_KNOTS ( 'NONE', 3,
 ( #59888, #51266, #11689, #5581, #66020, #90820, #74590, #81215, #13181, #73605, #4600, #82702 ),
 .UNSPECIFIED., .F., .F.,
 ( 4, 2, 2, 2, 2, 4 ),
 ( -0.003357017750235514672, -0.001150730439442379169, 0.001055556871350756334, 0.002158700526747327555, 0.003261844182143899644, 0.005468131492937042953 ),
 .UNSPECIFIED. ) ;
#52179 = CARTESIAN_POINT ( 'NONE',  ( -17.47620107869530770, 10.18187089365592612, -1.500000000000002220 ) ) ;
#52180 = ORIENTED_EDGE ( 'NONE', *, *, #12419, .F. ) ;
#52181 = EDGE_CURVE ( 'NONE', #92642, #61188, #34329, .T. ) ;
#52182 = CARTESIAN_POINT ( 'NONE',  ( -48.52287095715005449, -24.33927499327854349, 9.819080762295810061 ) ) ;
#52183 = ADVANCED_FACE ( 'NONE', ( #4030 ), #35480, .T. ) ;
#52184 = CARTESIAN_POINT ( 'NONE',  ( -41.52762579262719100, -25.31532796546315822, 5.102889718565096544 ) ) ;
#52185 = EDGE_CURVE ( 'NONE', #97904, #89884, #81649, .T. ) ;
#52186 = CARTESIAN_POINT ( 'NONE',  ( -101.5228709571501184, -24.51387760970725793, 9.387446482453407626 ) ) ;
#52187 = CARTESIAN_POINT ( 'NONE',  ( -125.6228709571500559, -29.50249982740957577, 7.747779886224967605 ) ) ;
#52189 = VERTEX_POINT ( 'NONE', #5020 ) ;
#52188 = CARTESIAN_POINT ( 'NONE',  ( 6.029407872858970840, -20.54391778677962677, 11.49999999999999645 ) ) ;
#52190 = CARTESIAN_POINT ( 'NONE',  ( 27.86270917940689174, 0.3587747205144265483, 29.49402280011862487 ) ) ;
#52191 = EDGE_CURVE ( 'NONE', #4006, #2140, #535, .T. ) ;
#52192 = ORIENTED_EDGE ( 'NONE', *, *, #90091, .F. ) ;
#52193 = B_SPLINE_CURVE_WITH_KNOTS ( 'NONE', 3,
 ( #29856, #75019, #97860, #53210 ),
 .UNSPECIFIED., .F., .F.,
 ( 4, 4 ),
 ( 0.000000000000000000, 9.999999999998897304E-05 ),
 .UNSPECIFIED. ) ;
#52194 = CARTESIAN_POINT ( 'NONE',  ( -20.39401028033356766, -3.670942005906183692, -1.500000000000002220 ) ) ;
#52195 = ORIENTED_EDGE ( 'NONE', *, *, #4476, .T. ) ;
#52196 = VECTOR ( 'NONE', #61721, 1000.000000000000000 ) ;
#52197 = B_SPLINE_SURFACE_WITH_KNOTS ( 'NONE', 3, 3, ( 
 ( #24039, #15427, #94055, #94554 ),
 ( #54013, #46388, #55512, #85950 ),
 ( #23527, #78321, #8827, #69733 ),
 ( #1221, #86447, #16932, #78816 ),
 ( #54505, #47897, #9312, #40277 ),
 ( #1720, #63635, #32657, #58019 ),
 ( #87448, #17940, #65639, #96066 ) ),
 .UNSPECIFIED., .F., .F., .F.,
 ( 4, 3, 4 ),
 ( 4, 4 ),
 ( 0.7945040050992232539, 0.8970133687736493444, 0.9995227324480754350 ),
 ( 0.1595345371825157288, 0.1606209134664254301 ),
 .UNSPECIFIED. ) ;
#52198 = CARTESIAN_POINT ( 'NONE',  ( -123.6228709571500559, -23.48786465467241769, 11.44779295918253759 ) ) ;
#52199 = VERTEX_POINT ( 'NONE', #59822 ) ;
#52200 = CARTESIAN_POINT ( 'NONE',  ( 4.039061187531148178, -5.876774720514399419, 18.18637930035166761 ) ) ;
#52201 = VERTEX_POINT ( 'NONE', #21228 ) ;
#52202 = CARTESIAN_POINT ( 'NONE',  ( 11.23609023086081038, -17.74952302366565604, -1.500000000000002220 ) ) ;
#52203 = EDGE_CURVE ( 'NONE', #17176, #37373, #16167, .T. ) ;
#52204 = CARTESIAN_POINT ( 'NONE',  ( -6.321128248299066499, 21.05883132939252533, 11.49999999999999645 ) ) ;
#52205 = CARTESIAN_POINT ( 'NONE',  ( -37.60902819999402880, -23.73791477778911485, 11.05961554403171121 ) ) ;
#52206 = CARTESIAN_POINT ( 'NONE',  ( -14.39138815452349718, -17.32352244779961481, -1.500000000000002220 ) ) ;
#52207 = CARTESIAN_POINT ( 'NONE',  ( 8.737904895026865404, 19.08465823478955414, -1.500000000000002220 ) ) ;
#52208 = CARTESIAN_POINT ( 'NONE',  ( -80.62287095715005592, -24.99132157543084531, 2.256160258750667502 ) ) ;
#52209 = CARTESIAN_POINT ( 'NONE',  ( -119.5893875598164158, -24.35071581493544457, 9.817618358456018157 ) ) ;
#52210 = CARTESIAN_POINT ( 'NONE',  ( -27.83739072329610664, 5.965225279485592225, -8.084349702057698650 ) ) ;
#52212 = ADVANCED_FACE ( 'NONE', ( #66939 ), #56298, .T. ) ;
#52211 = ORIENTED_EDGE ( 'NONE', *, *, #70090, .F. ) ;
#52213 = VECTOR ( 'NONE', #2972, 1000.000000000000000 ) ;
#52214 = ORIENTED_EDGE ( 'NONE', *, *, #26470, .F. ) ;
#52215 = B_SPLINE_CURVE_WITH_KNOTS ( 'NONE', 3,
 ( #61435, #53319, #51820, #76131, #29964, #84752, #76625, #83749, #92362, #37080, #22335, #14229, #6127, #60933, #82749, #52316, #44702, #75138 ),
 .UNSPECIFIED., .F., .F.,
 ( 4, 2, 2, 2, 2, 2, 2, 2, 4 ),
 ( 1.734723475976807094E-18, 0.0005889166363242025149, 0.001177833272648403295, 0.001766749908972604184, 0.002355666545296804856, 0.002944583181621005744, 0.003533499817945206633, 0.004122416454269406220, 0.004711333090593606242 ),
 .UNSPECIFIED. ) ;
#52216 = ORIENTED_EDGE ( 'NONE', *, *, #43488, .T. ) ;
#52217 = AXIS2_PLACEMENT_3D ( 'NONE', #40666, #42678, #95943 ) ;
#52218 = CARTESIAN_POINT ( 'NONE',  ( 4.621320343559619737, 12.50000000000004974, 2.100000000000000089 ) ) ;
#52219 = EDGE_CURVE ( 'NONE', #70136, #52051, #57352, .T. ) ;
#52220 = CARTESIAN_POINT ( 'NONE',  ( 2.695732861974529104, -21.29187259674557708, -1.500000000000002220 ) ) ;
#52221 = CARTESIAN_POINT ( 'NONE',  ( -86.62287095715004170, -23.73934037231756733, 11.05740245334328975 ) ) ;
#52222 = EDGE_LOOP ( 'NONE', ( #56823, #64969, #10935, #13871 ) ) ;
#52223 = CARTESIAN_POINT ( 'NONE',  ( -19.14942259116913092, -8.910193081567555851, 11.49999999999998934 ) ) ;
#52224 = CARTESIAN_POINT ( 'NONE',  ( -60.62287095715004881, -25.00182538069145011, 7.747789668545098429 ) ) ;
#52225 = CARTESIAN_POINT ( 'NONE',  ( -64.63657109733628658, -24.15543982623906771, -0.2315651400026674800 ) ) ;
#52226 = CARTESIAN_POINT ( 'NONE',  ( -64.62287095715005592, -23.48783264082478084, -1.443836473390069042 ) ) ;
#52227 = CARTESIAN_POINT ( 'NONE',  ( 6.620851319379956301, 3.316774720514426011, -27.30756699305372592 ) ) ;
#52228 = LINE ( 'NONE', #92271, #14634 ) ;
#52229 = CARTESIAN_POINT ( 'NONE',  ( -20.57447749561850969, 8.151157241358404804, -1.500000000000002220 ) ) ;
#52230 = CARTESIAN_POINT ( 'NONE',  ( -116.6235093916941992, -24.65952944569305316, 1.056160979905712560 ) ) ;
#52231 = EDGE_CURVE ( 'NONE', #94339, #35113, #46591, .T. ) ;
#52232 = CARTESIAN_POINT ( 'NONE',  ( -3.004714864173751998, -6.376774720514411854, 19.63296556618507083 ) ) ;
#52233 = DIRECTION ( 'NONE',  ( 0.000000000000000000, 2.173523156925980399E-06, -0.9999999999976378895 ) ) ;
#52234 = CARTESIAN_POINT ( 'NONE',  ( 10.46399479596398052, -3.105441387181091084, -27.03001098546561209 ) ) ;
#52235 = EDGE_CURVE ( 'NONE', #46666, #36769, #23735, .T. ) ;
#52236 = CARTESIAN_POINT ( 'NONE',  ( -100.5114892534503639, -24.40034930558991633, 0.3402023900116076804 ) ) ;
#52237 = VECTOR ( 'NONE', #13269, 1000.000000000000227 ) ;
#52238 = CARTESIAN_POINT ( 'NONE',  ( 6.036767712469883307, 18.47306877840545170, 11.49999999999998934 ) ) ;
#52239 = LOCAL_TIME ( 0, 54, 15.00000000000000000, #87439 ) ;
#52240 = CARTESIAN_POINT ( 'NONE',  ( 18.17913347391500523, 11.28257676469832660, 11.49999999999998934 ) ) ;
#52241 = CARTESIAN_POINT ( 'NONE',  ( -113.5895376238167245, -23.48786465467241769, 11.44779295918254114 ) ) ;
#52242 = DIRECTION ( 'NONE',  ( -3.773278334453079618E-23, 0.9999999999976377785, 2.173523156925979975E-06 ) ) ;
#52243 = ADVANCED_FACE ( 'NONE', ( #72435 ), #40978, .T. ) ;
#52244 = CARTESIAN_POINT ( 'NONE',  ( -106.5228709571500758, -24.65952944569305316, 1.056160979905704123 ) ) ;
#52245 = LINE ( 'NONE', #7057, #71724 ) ;
#52246 = CARTESIAN_POINT ( 'NONE',  ( -21.16596634977960179, 8.012090315382277339, -1.500000000000002220 ) ) ;
#52247 = VERTEX_POINT ( 'NONE', #48096 ) ;
#52248 = LINE ( 'NONE', #68469, #15792 ) ;
#52249 = LINE ( 'NONE', #7563, #91334 ) ;
#52250 = CARTESIAN_POINT ( 'NONE',  ( -18.77405512783484198, 6.205181830411797606, 11.49999999999999645 ) ) ;
#52251 = CARTESIAN_POINT ( 'NONE',  ( -59.62287095715004170, -24.65952944569304606, 1.056160979905694131 ) ) ;
#52252 = VECTOR ( 'NONE', #94136, 1000.000000000000000 ) ;
#52253 = CARTESIAN_POINT ( 'NONE',  ( -119.6228709571500417, -24.66019654487199730, 8.947790411086121054 ) ) ;
#52254 = ORIENTED_EDGE ( 'NONE', *, *, #36459, .F. ) ;
#52255 = CARTESIAN_POINT ( 'NONE',  ( 0.000000000000000000, 1.826774720514426464, 0.000000000000000000 ) ) ;
#52256 = LINE ( 'NONE', #91306, #9326 ) ;
#52257 = CARTESIAN_POINT ( 'NONE',  ( 17.85095790706337127, 12.24325521369631176, -1.500000000000002220 ) ) ;
#52258 = CARTESIAN_POINT ( 'NONE',  ( -13.89275734969026566, -5.965225279485572685, 30.51402280011862089 ) ) ;
#52259 = CARTESIAN_POINT ( 'NONE',  ( -70.52287095715007581, -25.00158670708909625, 2.256160236439166411 ) ) ;
#52260 = CARTESIAN_POINT ( 'NONE',  ( -10.27832545704433365, -4.855524038559839717, 28.80005113363453972 ) ) ;
#52261 = CARTESIAN_POINT ( 'NONE',  ( -40.52287095715005449, -24.99156044556202261, 7.747789690856173195 ) ) ;
#52262 = CARTESIAN_POINT ( 'NONE',  ( -19.78623529325263775, -1.157695164950638844, 11.49999999999998934 ) ) ;
#52263 = ORIENTED_EDGE ( 'NONE', *, *, #56281, .T. ) ;
#52264 = CARTESIAN_POINT ( 'NONE',  ( 8.194921280291850962, -18.63391395107102610, 11.49999999999999645 ) ) ;
#52265 = CARTESIAN_POINT ( 'NONE',  ( 29.73860345376319358, -3.356774720514428267, 1.647607965253212958 ) ) ;
#52267 = CIRCLE ( 'NONE', #65260, 1.700000000000000178 ) ;
#52266 = CARTESIAN_POINT ( 'NONE',  ( 6.150000000000003908, 1.999999999999998224, 19.19609335255483629 ) ) ;
#52268 = ORIENTED_EDGE ( 'NONE', *, *, #77071, .F. ) ;
#52269 = CARTESIAN_POINT ( 'NONE',  ( -30.56674980027052158, -25.57033040079278052, 6.142048374048878046 ) ) ;
#52270 = CARTESIAN_POINT ( 'NONE',  ( 11.86515846156731335, -3.316774720514427788, -28.09350142571734921 ) ) ;
#52271 = CARTESIAN_POINT ( 'NONE',  ( -99.55620429048340725, -23.48786465467241769, 11.44779295918254114 ) ) ;
#52272 = LINE ( 'NONE', #35556, #73222 ) ;
#52273 = CARTESIAN_POINT ( 'NONE',  ( -87.52287095715006160, -23.47596703998600631, 11.44779298504228393 ) ) ;
#52274 = CARTESIAN_POINT ( 'NONE',  ( -9.072532997253766496, -17.89392090870456542, -1.500000000000002220 ) ) ;
#52275 = DIRECTION ( 'NONE',  ( 0.000000000000000000, -1.000000000000000000, 0.000000000000000000 ) ) ;
#52276 = ORIENTED_EDGE ( 'NONE', *, *, #7638, .T. ) ;
#52277 = LINE ( 'NONE', #34179, #73855 ) ;
#52278 = CARTESIAN_POINT ( 'NONE',  ( 19.59772090806136902, -11.66877021596143926, 11.49999999999999645 ) ) ;
#52279 = CARTESIAN_POINT ( 'NONE',  ( -30.47287095715009286, -25.14093768624189451, 3.040070784493352551 ) ) ;
#52280 = AXIS2_PLACEMENT_3D ( 'NONE', #30269, #61247, #92170 ) ;
#52281 = CARTESIAN_POINT ( 'NONE',  ( -86.62287095715004170, -23.72747288104441665, -1.053458166803661555 ) ) ;
#52282 = CARTESIAN_POINT ( 'NONE',  ( -67.62287095715005592, -23.48783264082478794, -1.443836473390067265 ) ) ;
#52283 = CARTESIAN_POINT ( 'NONE',  ( 5.864225667603142789, -5.876774720514424288, 21.27837265517432996 ) ) ;
#52284 = B_SPLINE_CURVE_WITH_KNOTS ( 'NONE', 3,
 ( #31634, #52996, #22508, #8304 ),
 .UNSPECIFIED., .F., .F.,
 ( 4, 4 ),
 ( 0.000000000000000000, 1.000000000000000000 ),
 .UNSPECIFIED. ) ;
#52285 = CARTESIAN_POINT ( 'NONE',  ( -31.92287095715004597, -23.47593901973090169, -1.443836447538998424 ) ) ;
#52286 = CARTESIAN_POINT ( 'NONE',  ( -50.02177129897295771, -25.29440776045719730, 5.833784451200525467 ) ) ;
#52287 = ORIENTED_EDGE ( 'NONE', *, *, #62184, .F. ) ;
#52288 = EDGE_CURVE ( 'NONE', #73698, #83369, #85640, .T. ) ;
#52289 = CARTESIAN_POINT ( 'NONE',  ( -7.038884989605349141, -19.10714869031923513, -1.500000000000002220 ) ) ;
#52291 = EDGE_CURVE ( 'NONE', #30337, #29704, #26699, .T. ) ;
#52290 = ORIENTED_EDGE ( 'NONE', *, *, #17013, .F. ) ;
#52292 = CARTESIAN_POINT ( 'NONE',  ( 8.986065527603487979, -21.13286776747340667, 11.49999999999998934 ) ) ;
#52293 = CARTESIAN_POINT ( 'NONE',  ( -123.6228709571500559, -29.50250786944525672, 11.44777988621622811 ) ) ;
#52294 = EDGE_CURVE ( 'NONE', #71759, #57678, #32865, .T. ) ;
#52295 = ORIENTED_EDGE ( 'NONE', *, *, #73946, .T. ) ;
#52296 = CARTESIAN_POINT ( 'NONE',  ( 32.98733314340959311, -5.965225279485572685, 2.074222136288530027 ) ) ;
#52297 = EDGE_CURVE ( 'NONE', #11909, #32345, #77781, .T. ) ;
#52298 = CARTESIAN_POINT ( 'NONE',  ( -77.54282457048891786, -24.51419770103158768, 9.386484678747166299 ) ) ;
#52299 = AXIS2_PLACEMENT_3D ( 'NONE', #86809, #9689, #1589 ) ;
#52300 = CARTESIAN_POINT ( 'NONE',  ( -87.62287095715004170, -23.47596703998600631, 11.44779298504227860 ) ) ;
#52302 = ORIENTED_EDGE ( 'NONE', *, *, #32289, .T. ) ;
#52301 = CARTESIAN_POINT ( 'NONE',  ( -19.37389216307569129, 8.798533688548827669, 11.49999999999999645 ) ) ;
#52303 = LOCAL_TIME ( 0, 54, 15.00000000000000000, #11567 ) ;
#52304 = ORIENTED_EDGE ( 'NONE', *, *, #51860, .F. ) ;
#52305 = CARTESIAN_POINT ( 'NONE',  ( -0.8124730928778809425, -22.15030348749839817, 11.49999999999998934 ) ) ;
#52306 = CARTESIAN_POINT ( 'NONE',  ( -15.36756058500021282, 13.76162614515376426, -1.500000000000002220 ) ) ;
#52307 = VERTEX_POINT ( 'NONE', #16125 ) ;
#52309 = ORIENTED_EDGE ( 'NONE', *, *, #32947, .T. ) ;
#52308 = AXIS2_PLACEMENT_3D ( 'NONE', #45529, #36905, #97801 ) ;
#52310 = FACE_OUTER_BOUND ( 'NONE', #41859, .T. ) ;
#52311 = EDGE_CURVE ( 'NONE', #84261, #51872, #31804, .T. ) ;
#52312 = CARTESIAN_POINT ( 'NONE',  ( -121.6228709571500701, -23.96127896941633750, -0.6493128931037788210 ) ) ;
#52313 = ORIENTED_EDGE ( 'NONE', *, *, #16502, .F. ) ;
#52314 = ORIENTED_EDGE ( 'NONE', *, *, #32762, .T. ) ;
#52315 = VECTOR ( 'NONE', #11413, 1000.000000000000000 ) ;
#52316 = CARTESIAN_POINT ( 'NONE',  ( -124.5120815788254305, -25.30053193007085355, 4.607778174927528170 ) ) ;
#52317 = CARTESIAN_POINT ( 'NONE',  ( -41.48140342314091100, -24.66019654487199375, 8.947790411086124607 ) ) ;
#52318 = CARTESIAN_POINT ( 'NONE',  ( 15.63775912259741041, -4.567193422986002282, -28.22903731538627525 ) ) ;
#52319 = CARTESIAN_POINT ( 'NONE',  ( 0.4431998670617953717, 20.78131286043265646, -1.500000000000002220 ) ) ;
#52320 = CARTESIAN_POINT ( 'NONE',  ( 1.937016913031804455, -21.67664703184077268, 11.49999999999999645 ) ) ;
#52321 = CARTESIAN_POINT ( 'NONE',  ( -50.40895856474225667, -25.03284467579915784, 7.563174216508125269 ) ) ;
#52322 = CARTESIAN_POINT ( 'NONE',  ( -113.6228709571500417, -24.66019654487199730, 8.947790411086121054 ) ) ;
#52323 = CARTESIAN_POINT ( 'NONE',  ( -115.6244853095894030, -24.83618233451451118, 1.606449574219534826 ) ) ;
#52324 = CARTESIAN_POINT ( 'NONE',  ( 1.585521478320181865, 22.38520322874704149, -1.500000000000002220 ) ) ;
#52325 = CARTESIAN_POINT ( 'NONE',  ( -51.14398700470657388, -25.26334676438652238, 4.389973610351469269 ) ) ;
#52326 = VERTEX_POINT ( 'NONE', #10019 ) ;
#52327 = CARTESIAN_POINT ( 'NONE',  ( -59.52287095715006160, -23.47596703998600631, 11.44779298504228926 ) ) ;
#52328 = CARTESIAN_POINT ( 'NONE',  ( -51.01487234523126091, -25.13344938650803329, 2.963234457400254040 ) ) ;
#52329 = B_SPLINE_SURFACE_WITH_KNOTS ( 'NONE', 3, 3, ( 
 ( #44621, #12660, #99392, #28383 ),
 ( #51737, #98892, #14151, #59855 ),
 ( #45129, #74564, #90793, #21261 ),
 ( #60855, #5053, #66975, #52236 ),
 ( #83165, #13649, #75546, #6554 ),
 ( #15157, #86672, #9548, #7551 ),
 ( #78545, #61356, #93782, #47627 ),
 ( #434, #17160, #24276, #32389 ),
 ( #31389, #8552, #46124, #92776 ),
 ( #38503, #69452, #92280, #54741 ) ),
 .UNSPECIFIED., .F., .F., .F.,
 ( 4, 3, 3, 4 ),
 ( 4, 4 ),
 ( 0.0004766839783820097840, 0.1491231665100171411, 0.2234464077758346878, 0.2977696490416522623 ),
 ( 0.2995301736809518056, 0.3007213872290413481 ),
 .UNSPECIFIED. ) ;
#52330 = ORIENTED_EDGE ( 'NONE', *, *, #41424, .T. ) ;
#52331 = ORIENTED_EDGE ( 'NONE', *, *, #69713, .F. ) ;
#52332 = CARTESIAN_POINT ( 'NONE',  ( -99.30055519532314179, -25.26880003473793934, 6.071376037430450623 ) ) ;
#52333 = ORIENTED_EDGE ( 'NONE', *, *, #27621, .F. ) ;
#52334 = CONICAL_SURFACE ( 'NONE', #70133, 2.999999999999999112, 0.7853981633974412846 ) ;
#52335 = CARTESIAN_POINT ( 'NONE',  ( -9.505907188867841029, -19.02311915605711690, -1.500000000000002220 ) ) ;
#52336 = ORIENTED_EDGE ( 'NONE', *, *, #52291, .T. ) ;
#52337 = FACE_OUTER_BOUND ( 'NONE', #15702, .T. ) ;
#52338 = CARTESIAN_POINT ( 'NONE',  ( 7.388015978253313243, 19.69965359013245632, 11.49999999999998934 ) ) ;
#52339 = CARTESIAN_POINT ( 'NONE',  ( 30.53060340732036337, -1.477225279485574028, -1.352392034746782823 ) ) ;
#52340 = CARTESIAN_POINT ( 'NONE',  ( -2.919094682108430483, 22.50186656173435296, 11.49999999999998934 ) ) ;
#52341 = CARTESIAN_POINT ( 'NONE',  ( -113.5228709571500616, -23.47596703998600631, 11.44779298504228038 ) ) ;
#52342 = DIRECTION ( 'NONE',  ( 0.000000000000000000, -1.000000000000000000, 0.000000000000000000 ) ) ;
#52343 = CARTESIAN_POINT ( 'NONE',  ( -12.46176837856299002, 18.05058065364367792, -1.500000000000002220 ) ) ;
#52344 = DIRECTION ( 'NONE',  ( 0.000000000000000000, 0.9999999999976377785, 2.173523156925979975E-06 ) ) ;
#52345 = EDGE_LOOP ( 'NONE', ( #38680, #12719, #25989, #55094 ) ) ;
#52346 = CARTESIAN_POINT ( 'NONE',  ( -122.5894804180817914, -24.35071581493544102, 9.817618358456019934 ) ) ;
#52347 = VECTOR ( 'NONE', #1284, 1000.000000000000227 ) ;
#52348 = EDGE_CURVE ( 'NONE', #55090, #62812, #33065, .T. ) ;
#52349 = CARTESIAN_POINT ( 'NONE',  ( -120.5228709571500900, -24.51163499207180507, 0.6490370598555513793 ) ) ;
#52350 = CIRCLE ( 'NONE', #94496, 129.7684398600581517 ) ;
#52351 = CARTESIAN_POINT ( 'NONE',  ( -126.9228709571500815, -23.47596703998600631, 11.44779298504227860 ) ) ;
#52352 = CARTESIAN_POINT ( 'NONE',  ( 22.02124265030973760, 3.456774720514426136, 16.20402280011862217 ) ) ;
#52353 = CARTESIAN_POINT ( 'NONE',  ( 13.65650298889772962, 16.33668418983593185, 11.49999999999998934 ) ) ;
#52354 = CARTESIAN_POINT ( 'NONE',  ( -112.5188950414697615, -23.96119346886881729, -0.6495511937831841554 ) ) ;
#52355 = FACE_OUTER_BOUND ( 'NONE', #36700, .T. ) ;
#52356 = EDGE_CURVE ( 'NONE', #42247, #9388, #95959, .T. ) ;
#52357 = DIRECTION ( 'NONE',  ( -0.6177208787939548751, -1.709253021876320418E-06, 0.7863974287210651060 ) ) ;
#52358 = CARTESIAN_POINT ( 'NONE',  ( -33.59407879448789203, -24.15543982623906771, -0.2315651400026580431 ) ) ;
#52359 = CARTESIAN_POINT ( 'NONE',  ( -117.6270234476128991, -23.96169478059714564, 10.65365249895717170 ) ) ;
#52360 = ORIENTED_EDGE ( 'NONE', *, *, #29611, .F. ) ;
#52361 = CARTESIAN_POINT ( 'NONE',  ( -98.97790923573467126, -25.21099978369031902, 6.596929975353639009 ) ) ;
#52362 = CARTESIAN_POINT ( 'NONE',  ( 15.22544387773384500, -12.34335808662847178, 11.49999999999999645 ) ) ;
#52363 = CARTESIAN_POINT ( 'NONE',  ( -75.52287095715006160, -24.99156044556120548, 7.747789690856173195 ) ) ;
#52364 = CARTESIAN_POINT ( 'NONE',  ( -129.6228709571500701, -23.48786465467241769, 11.44779295918253581 ) ) ;
#52365 = VERTEX_POINT ( 'NONE', #48606 ) ;
#52366 = CARTESIAN_POINT ( 'NONE',  ( -68.94158865110078693, -25.25654263764466023, 6.096958949246902293 ) ) ;
#52367 = CARTESIAN_POINT ( 'NONE',  ( -29.49875734969026198, 5.965225279485572685, 2.362022800118626531 ) ) ;
#52368 = CARTESIAN_POINT ( 'NONE',  ( -31.62287095715004526, -24.33832256526967797, 0.1851278514119824858 ) ) ;
#52369 = VECTOR ( 'NONE', #71485, 1000.000000000000000 ) ;
#52370 = CARTESIAN_POINT ( 'NONE',  ( -106.5228709571500900, -23.96127896941632329, -0.6493128931037995821 ) ) ;
#52371 = CARTESIAN_POINT ( 'NONE',  ( -16.05533900033903549, 11.45903963230415101, -1.500000000000002220 ) ) ;
#52373 = EDGE_LOOP ( 'NONE', ( #76404, #64511, #91508, #59800 ) ) ;
#52372 = ORGANIZATION ( 'NAUO-ORG11', 'UNSPECIFIED', 'UNSPECIFIED' ) ;
#52374 = DIRECTION ( 'NONE',  ( 0.000000000000000000, -0.9999999999976377785, -2.173523156925979975E-06 ) ) ;
#52375 = FACE_OUTER_BOUND ( 'NONE', #37242, .T. ) ;
#52376 = B_SPLINE_CURVE_WITH_KNOTS ( 'NONE', 3,
 ( #67085, #92386, #97995, #28496, #60470, #90402 ),
 .UNSPECIFIED., .F., .F.,
 ( 4, 2, 4 ),
 ( 6.384118678602582405E-06, 0.001386860460828368046, 0.002767336802978133219 ),
 .UNSPECIFIED. ) ;
#52377 = AXIS2_PLACEMENT_3D ( 'NONE', #93680, #93179, #39900 ) ;
#52378 = APPROVAL_DATE_TIME ( #82811, #92807 ) ;
#52379 = ORIENTED_EDGE ( 'NONE', *, *, #71943, .T. ) ;
#52380 = DIRECTION ( 'NONE',  ( -0.000000000000000000, 1.000000000000000000, -0.000000000000000000 ) ) ;
#52381 = DIRECTION ( 'NONE',  ( 0.000000000000000000, -1.000000000000000000, -1.224646799147353207E-16 ) ) ;
#52382 = CARTESIAN_POINT ( 'NONE',  ( -55.57509554726114231, -25.00158670708910336, 2.256160236439221034 ) ) ;
#52383 = CARTESIAN_POINT ( 'NONE',  ( -118.6249414734990637, -24.34968618360934300, 0.1864209137778906622 ) ) ;
#52384 = CARTESIAN_POINT ( 'NONE',  ( -31.62287095715005236, -24.64965695001467694, 8.947790433994189385 ) ) ;
#52385 = DIRECTION ( 'NONE',  ( 1.000000000000000000, 0.000000000000000000, -1.104558621438292892E-14 ) ) ;
#52386 = CIRCLE ( 'NONE', #78297, 27.94799999999999685 ) ;
#52387 = CARTESIAN_POINT ( 'NONE',  ( 25.05730599792488533, -1.684774720501991174, -18.59674224247030239 ) ) ;
#52388 = CARTESIAN_POINT ( 'NONE',  ( 15.90762396150235958, 12.10710967819287198, -1.500000000000002220 ) ) ;
#52389 = LINE ( 'NONE', #14306, #59725 ) ;
#52390 = CARTESIAN_POINT ( 'NONE',  ( -45.62923257921450215, -24.83644354573578283, 8.397322867130103674 ) ) ;
#52391 = ORIENTED_EDGE ( 'NONE', *, *, #39411, .F. ) ;
#52392 = FACE_OUTER_BOUND ( 'NONE', #64446, .T. ) ;
#52393 = CARTESIAN_POINT ( 'NONE',  ( 4.653846153846159517, -6.376774720514415407, 19.99999999999999289 ) ) ;
#52394 = CARTESIAN_POINT ( 'NONE',  ( -8.160000000000000142, -9.652339641703484574, 1.628518864987183790 ) ) ;
#52395 = CARTESIAN_POINT ( 'NONE',  ( -80.49780302488923667, -24.73531770709095312, 8.716586749053508498 ) ) ;
#52396 = CARTESIAN_POINT ( 'NONE',  ( -125.7763423481509903, -25.21288808264143455, 6.500921239251876926 ) ) ;
#52397 = CARTESIAN_POINT ( 'NONE',  ( -39.53919957490392534, -24.34968618360933235, 0.1864209137778788106 ) ) ;
#52398 = DIRECTION ( 'NONE',  ( -3.773278334453079030E-23, 0.9999999999976377785, 2.173523156925979128E-06 ) ) ;
#52399 = CARTESIAN_POINT ( 'NONE',  ( -2.148731487934370410, -5.876774720514411854, 19.46295461892501422 ) ) ;
#52400 = B_SPLINE_SURFACE_WITH_KNOTS ( 'NONE', 3, 1, ( 
 ( #86662, #2438 ),
 ( #63859, #10040 ),
 ( #19146, #64360 ),
 ( #95778, #73448 ),
 ( #50114, #32887 ),
 ( #48117, #42010 ),
 ( #81053, #34881 ),
 ( #25261, #10538 ),
 ( #56240, #56739 ),
 ( #95282, #72953 ),
 ( #49621, #80052 ),
 ( #88674, #25767 ),
 ( #71455, #41000 ),
 ( #11535, #1943 ),
 ( #3941, #65857 ),
 ( #41499, #72452 ),
 ( #3449, #96775 ),
 ( #27274, #18643 ),
 ( #88174, #64865 ) ),
 .UNSPECIFIED., .F., .F., .F.,
 ( 4, 1, 1, 1, 1, 1, 1, 1, 1, 1, 1, 1, 1, 1, 1, 1, 4 ),
 ( 2, 2 ),
 ( 0.000000000000000000, 0.07735147826526211912, 0.1497817737883345712, 0.2198699552839545879, 0.2879755066202366320, 0.3546781060271970709, 0.4187834319376942949, 0.4827347082469880535, 0.5473072519464166064, 0.5826981022599677651, 0.6240955651677915217, 0.6712929496345372282, 0.7243202075485738467, 0.7838489433400219752, 0.8494366971205808969, 0.9216570148062976919, 1.000000000000000000 ),
 ( 0.000000000000000000, 1.000000000000000000 ),
 .UNSPECIFIED. ) ;
#52401 = FACE_OUTER_BOUND ( 'NONE', #99487, .T. ) ;
#52402 = CARTESIAN_POINT ( 'NONE',  ( -127.5210452836834349, -24.51314013834318217, 0.6176544820404269442 ) ) ;
#52403 = VERTEX_POINT ( 'NONE', #86143 ) ;
#52404 = ADVANCED_FACE ( 'NONE', ( #71938 ), #78514, .T. ) ;
#52405 = CARTESIAN_POINT ( 'NONE',  ( -3.766600276044322904, -19.90762401167813067, -1.500000000000002220 ) ) ;
#52406 = CARTESIAN_POINT ( 'NONE',  ( -122.5557273655149118, -23.96119346886880663, -0.6495511937832028071 ) ) ;
#52407 = CARTESIAN_POINT ( 'NONE',  ( 3.794707603699265519E-15, -5.876774720514426953, 17.50000000000000000 ) ) ;
#52408 = AXIS2_PLACEMENT_3D ( 'NONE', #93004, #85395, #21491 ) ;
#52409 = EDGE_CURVE ( 'NONE', #99116, #92497, #18134, .T. ) ;
#52410 = CARTESIAN_POINT ( 'NONE',  ( 22.02124265030973760, 7.743225279485574042, 16.20402280011862217 ) ) ;
#52411 = EDGE_CURVE ( 'NONE', #884, #11305, #35410, .T. ) ;
#52412 = ORIENTED_EDGE ( 'NONE', *, *, #86332, .T. ) ;
#52413 = CARTESIAN_POINT ( 'NONE',  ( 4.621320343559619737, 12.50000000000004974, 2.100000000000000089 ) ) ;
#52414 = CARTESIAN_POINT ( 'NONE',  ( -46.52287095715006160, -23.47596703998600631, 11.44779298504229104 ) ) ;
#52415 = CARTESIAN_POINT ( 'NONE',  ( -0.3114230556345199963, -20.10660241673355486, -1.500000000000002220 ) ) ;
#52416 = AXIS2_PLACEMENT_3D ( 'NONE', #58664, #35827, #34334 ) ;
#52417 = ADVANCED_FACE ( 'NONE', ( #20127 ), #42984, .T. ) ;
#52418 = CARTESIAN_POINT ( 'NONE',  ( -17.44821286160079410, -11.81026508430653088, 11.49999999999999645 ) ) ;
#52419 = CARTESIAN_POINT ( 'NONE',  ( -79.52287095715006160, -29.50250786944525672, 11.44777988621623521 ) ) ;
#52420 = CARTESIAN_POINT ( 'NONE',  ( -70.51358061702791247, -23.85049219812685806, 10.88485053497527311 ) ) ;
#52421 = CARTESIAN_POINT ( 'NONE',  ( 17.94654606563480215, 12.89224558282342947, -1.500000000000002220 ) ) ;
#52422 = EDGE_CURVE ( 'NONE', #42104, #90352, #41517, .T. ) ;
#52423 = CARTESIAN_POINT ( 'NONE',  ( -14.38416181709762043, 14.64695106392160895, 11.49999999999998934 ) ) ;
#52424 = CARTESIAN_POINT ( 'NONE',  ( -13.36367879947601445, -6.376774720514426953, 20.00000000000000355 ) ) ;
#52425 = CARTESIAN_POINT ( 'NONE',  ( -55.58953762381671737, -24.99132157543083821, 2.256160258750496084 ) ) ;
#52426 = CARTESIAN_POINT ( 'NONE',  ( -125.6228709571500559, -23.47596703998600631, 11.44779298504227860 ) ) ;
#52427 = ORIENTED_EDGE ( 'NONE', *, *, #82517, .F. ) ;
#52428 = CARTESIAN_POINT ( 'NONE',  ( -27.70544111104076990, -24.64017222881049207, 8.251826729410561612 ) ) ;
#52429 = CARTESIAN_POINT ( 'NONE',  ( -4.568292318365942073, -5.965225279485572685, 30.06720597538392425 ) ) ;
#52430 = ORIENTED_EDGE ( 'NONE', *, *, #58026, .F. ) ;
#52431 = ORIENTED_EDGE ( 'NONE', *, *, #37536, .F. ) ;
#52432 = LINE ( 'NONE', #45812, #17823 ) ;
#52433 = CARTESIAN_POINT ( 'NONE',  ( -71.62287095715004170, -24.50321055353806443, 9.387540953477532923 ) ) ;
#52435 = EDGE_CURVE ( 'NONE', #923, #86931, #54812, .T. ) ;
#52434 = CARTESIAN_POINT ( 'NONE',  ( -0.3982818654701407723, -6.376774720514410077, 19.46306892155547530 ) ) ;
#52436 = CARTESIAN_POINT ( 'NONE',  ( -18.11865614447288664, 9.752654332028551920, -1.500000000000002220 ) ) ;
#52437 = CARTESIAN_POINT ( 'NONE',  ( 20.98369277809155165, -4.918611649023987731, 11.49999999999999645 ) ) ;
#52438 = VERTEX_POINT ( 'NONE', #51089 ) ;
#52439 = DIRECTION ( 'NONE',  ( 3.773278334444167608E-23, -1.000000000000000000, 0.000000000000000000 ) ) ;
#52440 = DIRECTION ( 'NONE',  ( 0.000000000000000000, 0.000000000000000000, 1.000000000000000000 ) ) ;
#52441 = CARTESIAN_POINT ( 'NONE',  ( 21.86734719908870872, 4.625976558377421277, -1.500000000000002220 ) ) ;
#52443 = DIRECTION ( 'NONE',  ( 0.000000000000000000, -0.9999999999976377785, -2.173523156925979128E-06 ) ) ;
#52442 = VECTOR ( 'NONE', #62089, 1000.000000000000114 ) ;
#52444 = CARTESIAN_POINT ( 'NONE',  ( -84.64006920983196380, -23.73766607897669445, -1.055555164236457566 ) ) ;
#52445 = ORIENTED_EDGE ( 'NONE', *, *, #63095, .F. ) ;
#52446 = DIRECTION ( 'NONE',  ( -0.000000000000000000, -1.000000000000000000, -0.000000000000000000 ) ) ;
#52447 = CARTESIAN_POINT ( 'NONE',  ( -35.46876340121657023, -24.92592662359560407, 8.075495903017991139 ) ) ;
#52448 = CARTESIAN_POINT ( 'NONE',  ( -10.06633388967972209, 18.29571535785830960, 11.49999999999998934 ) ) ;
#52449 = ORIENTED_EDGE ( 'NONE', *, *, #53172, .T. ) ;
#52451 = ORIENTED_EDGE ( 'NONE', *, *, #86302, .F. ) ;
#52450 = FACE_OUTER_BOUND ( 'NONE', #90588, .T. ) ;
#52452 = ORIENTED_EDGE ( 'NONE', *, *, #30758, .F. ) ;
#52453 = AXIS2_PLACEMENT_3D ( 'NONE', #81077, #89192, #58247 ) ;
#52454 = CARTESIAN_POINT ( 'NONE',  ( -100.6255024803089384, -24.83644354573579349, 8.397322867130096569 ) ) ;
#52455 = CARTESIAN_POINT ( 'NONE',  ( 6.686094007546604878, -20.02240253118446844, -1.500000000000002220 ) ) ;
#52456 = ORIENTED_EDGE ( 'NONE', *, *, #6982, .F. ) ;
#52457 = CARTESIAN_POINT ( 'NONE',  ( -117.5535922921180543, -24.34968618360934656, 0.1864209137778901071 ) ) ;
#52458 = CARTESIAN_POINT ( 'NONE',  ( -35.58953762381671737, -25.00182538069144655, 7.747789668545102870 ) ) ;
#52459 = CARTESIAN_POINT ( 'NONE',  ( -19.23829340896090656, 10.21096329589227025, 11.49999999999998934 ) ) ;
#52460 = CARTESIAN_POINT ( 'NONE',  ( -110.2414738297690775, -25.25449932609592096, 6.186391010255299250 ) ) ;
#52461 = VECTOR ( 'NONE', #58855, 1000.000000000000000 ) ;
#52462 = FACE_OUTER_BOUND ( 'NONE', #1193, .T. ) ;
#52463 = CARTESIAN_POINT ( 'NONE',  ( -80.11765714520616655, -25.14277807208376458, 7.046040345931035453 ) ) ;
#52464 = CARTESIAN_POINT ( 'NONE',  ( 20.57166443188586769, -7.073620337204646447, -1.500000000000002220 ) ) ;
#52465 = CARTESIAN_POINT ( 'NONE',  ( -106.5228709571500758, -23.48786465467242479, 11.44779295918253936 ) ) ;
#52467 = ORIENTED_EDGE ( 'NONE', *, *, #65844, .T. ) ;
#52466 = CARTESIAN_POINT ( 'NONE',  ( -10.28394192611005842, 19.82837715243953625, 11.49999999999999645 ) ) ;
#52468 = CARTESIAN_POINT ( 'NONE',  ( -45.62287095715007723, -24.83602698348160231, 1.605859176311266623 ) ) ;
#52469 = CARTESIAN_POINT ( 'NONE',  ( -10.11875734969026297, -3.316774720514426456, 30.51402280011862089 ) ) ;
#52470 = ADVANCED_FACE ( 'NONE', ( #3926 ), #12016, .F. ) ;
#52471 = CARTESIAN_POINT ( 'NONE',  ( -77.62287095715007013, -23.48783264082478794, -1.443836473390065933 ) ) ;
#52472 = EDGE_LOOP ( 'NONE', ( #28552, #72489, #41468, #82535 ) ) ;
#52473 = ORIENTED_EDGE ( 'NONE', *, *, #24455, .F. ) ;
#52474 = EDGE_CURVE ( 'NONE', #91631, #49598, #72973, .T. ) ;
#52475 = ORIENTED_EDGE ( 'NONE', *, *, #52710, .F. ) ;
#52476 = CARTESIAN_POINT ( 'NONE',  ( -0.02075734969026423599, 5.965225279485572685, -0.08597719988137648983 ) ) ;
#52477 = CARTESIAN_POINT ( 'NONE',  ( -20.27875734969026311, 3.456774720514426136, 25.15402280011862146 ) ) ;
#52478 = CARTESIAN_POINT ( 'NONE',  ( 30.60111574538730039, -4.387371784078713866, 26.76015704162893627 ) ) ;
#52479 = CARTESIAN_POINT ( 'NONE',  ( -43.62287095715003460, -23.47596703998600276, 11.44779298504227505 ) ) ;
#52480 = LINE ( 'NONE', #46356, #31381 ) ;
#52481 = CARTESIAN_POINT ( 'NONE',  ( -4.359330469889163950, 18.88329184224734192, -1.500000000000002220 ) ) ;
#52482 = EDGE_CURVE ( 'NONE', #62581, #24865, #2695, .T. ) ;
#52483 = CARTESIAN_POINT ( 'NONE',  ( -103.6228709571500559, -24.64898659630368627, 1.056161002820829697 ) ) ;
#52484 = EDGE_LOOP ( 'NONE', ( #97869, #71445, #71397, #71677 ) ) ;
#52485 = CARTESIAN_POINT ( 'NONE',  ( 19.04819733361787470, -3.913502273677552878, 11.49999999999999645 ) ) ;
#52486 = CARTESIAN_POINT ( 'NONE',  ( -88.22287095715006444, -23.47596703998600631, 11.44779298504227860 ) ) ;
#52487 = EDGE_CURVE ( 'NONE', #68362, #18995, #86667, .T. ) ;
#52488 = VERTEX_POINT ( 'NONE', #42495 ) ;
#52490 = DIRECTION ( 'NONE',  ( 0.000000000000000000, 1.000000000000000000, 0.000000000000000000 ) ) ;
#52489 = AXIS2_PLACEMENT_3D ( 'NONE', #68633, #99551, #84845 ) ;
#52491 = CARTESIAN_POINT ( 'NONE',  ( 3.398951772795901771, -6.376774720514402972, 18.23562605320997676 ) ) ;
#52492 = CARTESIAN_POINT ( 'NONE',  ( -116.5228709571500474, -24.33832256527048088, 0.1851278514138653408 ) ) ;
#52493 = CARTESIAN_POINT ( 'NONE',  ( -63.94589268014165384, -23.78087380709146004, 10.97511746239721298 ) ) ;
#52494 = CARTESIAN_POINT ( 'NONE',  ( 18.19143915067776263, 7.407926943018095400, 11.49999999999998934 ) ) ;
#52495 = AXIS2_PLACEMENT_3D ( 'NONE', #69945, #93780, #432 ) ;
#52496 = CARTESIAN_POINT ( 'NONE',  ( -46.54684453743023198, -24.15543982623906771, -0.2315651400026683127 ) ) ;
#52497 = EDGE_LOOP ( 'NONE', ( #56482, #53395, #11831, #85871 ) ) ;
#52498 = CARTESIAN_POINT ( 'NONE',  ( 0.7969447072908428797, -21.54811710690876225, -1.500000000000002220 ) ) ;
#52499 = DIRECTION ( 'NONE',  ( 1.000000000000000000, 0.000000000000000000, 0.000000000000000000 ) ) ;
#52500 = CARTESIAN_POINT ( 'NONE',  ( -115.9228709571500815, -23.47593901973090524, -1.443836447538996426 ) ) ;
#52501 = CARTESIAN_POINT ( 'NONE',  ( -6.660000000000001030, -2.890508098367099432, -0.2344417481469836528 ) ) ;
#52502 = CARTESIAN_POINT ( 'NONE',  ( -99.59031406714542811, -25.18439430774925114, 3.731155517086302886 ) ) ;
#52503 = CARTESIAN_POINT ( 'NONE',  ( 8.428894486204411507, 21.44871590506140890, -1.500000000000002220 ) ) ;
#52504 = CC_DESIGN_DATE_AND_TIME_ASSIGNMENT ( #67612, #42781, ( #97564 ) ) ;
#52505 = PERSON_AND_ORGANIZATION_ROLE ( 'design_owner' ) ;
#52506 = PLANE ( 'NONE',  #41817 ) ;
#52507 = CARTESIAN_POINT ( 'NONE',  ( -50.10007593363737044, -25.29249258120279009, 4.255736650380444352 ) ) ;
#52508 = CARTESIAN_POINT ( 'NONE',  ( 17.11712468798820908, 10.61635618877791742, 11.49999999999999645 ) ) ;
#52509 = DIRECTION ( 'NONE',  ( 0.000000000000000000, 0.000000000000000000, 1.000000000000000000 ) ) ;
#52510 = LINE ( 'NONE', #6817, #59665 ) ;
#52511 = DIRECTION ( 'NONE',  ( 0.000000000000000000, 0.000000000000000000, -1.000000000000000000 ) ) ;
#52512 = DIRECTION ( 'NONE',  ( 0.000000000000000000, 0.9999999999976377785, 2.173523156925979975E-06 ) ) ;
#52513 = CARTESIAN_POINT ( 'NONE',  ( -110.7296117302316532, -25.18425597211279410, 3.360883082042677383 ) ) ;
#52514 = CARTESIAN_POINT ( 'NONE',  ( 4.721227339208565965, -19.33841413273825793, -1.500000000000002220 ) ) ;
#52515 = CARTESIAN_POINT ( 'NONE',  ( -113.5205660264642802, -23.73766607897670866, -1.055555164236448240 ) ) ;
#52516 = CARTESIAN_POINT ( 'NONE',  ( 18.24634267693259559, -7.554628487255452107, -1.500000000000002220 ) ) ;
#52517 = CARTESIAN_POINT ( 'NONE',  ( 30.00738719773716312, -1.477225279485574028, -9.049252915307087974 ) ) ;
#52518 = LINE ( 'NONE', #5342, #67829 ) ;
#52519 = CARTESIAN_POINT ( 'NONE',  ( -1.653359744423585465, -6.376774720514413630, 19.34586827028017098 ) ) ;
#52520 = CARTESIAN_POINT ( 'NONE',  ( 11.71144010791963730, -17.07555522294065753, 11.49999999999999645 ) ) ;
#52521 = CARTESIAN_POINT ( 'NONE',  ( -98.62287095715005592, -24.64898659630529210, 1.056161002820829697 ) ) ;
#52522 = DIRECTION ( 'NONE',  ( -8.503546450866701308E-16, 0.000000000000000000, 1.000000000000000000 ) ) ;
#52523 = CARTESIAN_POINT ( 'NONE',  ( -128.5228709571500758, -24.64965694238575722, 8.947790433994189385 ) ) ;
#52524 = CARTESIAN_POINT ( 'NONE',  ( 12.08046422559826816, 19.21373320108137861, 11.49999999999999645 ) ) ;
#52525 = ORIENTED_EDGE ( 'NONE', *, *, #66303, .F. ) ;
#52526 = CARTESIAN_POINT ( 'NONE',  ( -78.55620429048339304, -24.65952944569304606, 1.056160979905699904 ) ) ;
#52527 = CARTESIAN_POINT ( 'NONE',  ( 2.246611357655420083, -0.1632191352058117717, 0.1632191352058111888 ) ) ;
#52528 = CARTESIAN_POINT ( 'NONE',  ( 3.569899647507075890, 19.86734082857295647, 11.49999999999998934 ) ) ;
#52529 = EDGE_CURVE ( 'NONE', #13388, #46438, #73922, .T. ) ;
#52530 = CARTESIAN_POINT ( 'NONE',  ( -63.49958784806312906, -24.34968618360933235, 0.1864209137778804204 ) ) ;
#52531 = CARTESIAN_POINT ( 'NONE',  ( -52.52287095715006870, -23.47596703998600631, 11.44779298504229104 ) ) ;
#52532 = EDGE_LOOP ( 'NONE', ( #57937, #8352, #53076, #54774 ) ) ;
#52533 = ORIENTED_EDGE ( 'NONE', *, *, #18024, .T. ) ;
#52534 = CARTESIAN_POINT ( 'NONE',  ( 0.3180806761505774460, -5.876774720514415407, 20.02963804100705403 ) ) ;
#52535 = CARTESIAN_POINT ( 'NONE',  ( 11.15996004898972771, 19.99216496293481882, 11.49999999999998934 ) ) ;
#52536 = CARTESIAN_POINT ( 'NONE',  ( -29.51208538039775320, -23.65073901887618391, -1.055554856561816246 ) ) ;
#52537 = CARTESIAN_POINT ( 'NONE',  ( -4.138935798035190849, -21.16376344109877294, -1.500000000000002220 ) ) ;
#52538 = CARTESIAN_POINT ( 'NONE',  ( -123.5890690777296754, -24.51314013834316796, 0.6176544820404235026 ) ) ;
#52539 = CARTESIAN_POINT ( 'NONE',  ( -34.57522798308936984, -24.65952944569304606, 1.056160979905694353 ) ) ;
#52540 = EDGE_CURVE ( 'NONE', #72780, #83889, #13632, .T. ) ;
#52541 = CARTESIAN_POINT ( 'NONE',  ( 6.973883220674568229, 19.69035807221911938, 11.49999999999999645 ) ) ;
#52542 = ORIENTED_EDGE ( 'NONE', *, *, #70205, .F. ) ;
#52543 = CARTESIAN_POINT ( 'NONE',  ( -27.75896112051811926, -24.78822140492940918, 2.278705362813905122 ) ) ;
#52544 = CARTESIAN_POINT ( 'NONE',  ( 13.70243205411677145, -17.22335469805116048, 11.49999999999998934 ) ) ;
#52545 = EDGE_CURVE ( 'NONE', #24081, #26377, #12377, .T. ) ;
#52546 = VECTOR ( 'NONE', #90707, 1000.000000000000000 ) ;
#52547 = FACE_OUTER_BOUND ( 'NONE', #30699, .T. ) ;
#52548 = CARTESIAN_POINT ( 'NONE',  ( -41.86772617331516955, -25.10926054140117003, 4.147750411746549126 ) ) ;
#52549 = EDGE_LOOP ( 'NONE', ( #81625, #21827, #32100, #78502 ) ) ;
#52550 = CARTESIAN_POINT ( 'NONE',  ( 3.960454120839856706, -6.376774720514402972, 18.17119035270509997 ) ) ;
#52551 = CARTESIAN_POINT ( 'NONE',  ( -90.50269173505331821, -24.73531770709095312, 8.716586749053512051 ) ) ;
#52552 = ORIENTED_EDGE ( 'NONE', *, *, #63488, .T. ) ;
#52553 = DIRECTION ( 'NONE',  ( -3.773278334453079030E-23, 0.9999999999976377785, 2.173523156925979128E-06 ) ) ;
#52554 = B_SPLINE_CURVE_WITH_KNOTS ( 'NONE', 3,
 ( #9061, #46638, #31902, #62359, #93285, #79065 ),
 .UNSPECIFIED., .F., .F.,
 ( 4, 2, 4 ),
 ( 1.570755371634190273E-05, 0.001396183895866089054, 0.002776660238015836446 ),
 .UNSPECIFIED. ) ;
#52555 = EDGE_LOOP ( 'NONE', ( #67961, #10491, #26344, #11374 ) ) ;
#52556 = ORIENTED_EDGE ( 'NONE', *, *, #3697, .T. ) ;
#52557 = CARTESIAN_POINT ( 'NONE',  ( -71.54508653244631944, -24.35071581493543391, 9.817618358456021710 ) ) ;
#52558 = CARTESIAN_POINT ( 'NONE',  ( -42.52287095715005449, -29.50248528299804818, 1.056150453629031594 ) ) ;
#52560 = EDGE_CURVE ( 'NONE', #77258, #46666, #26748, .T. ) ;
#52559 = CARTESIAN_POINT ( 'NONE',  ( -36.52201406890371516, -23.48783264082477018, -1.443836473390095909 ) ) ;
#52561 = CARTESIAN_POINT ( 'NONE',  ( 17.64890103348723116, 10.21726211432410203, -1.500000000000002220 ) ) ;
#52562 = B_SPLINE_CURVE_WITH_KNOTS ( 'NONE', 3,
 ( #11795, #37130, #51366, #67106, #28515, #66118 ),
 .UNSPECIFIED., .F., .F.,
 ( 4, 2, 4 ),
 ( 1.570887131794638196E-05, 0.001396322306279760422, 0.002776935741241574537 ),
 .UNSPECIFIED. ) ;
#52563 = CIRCLE ( 'NONE', #15307, 3.060000000000000053 ) ;
#52564 = ORIENTED_EDGE ( 'NONE', *, *, #53233, .F. ) ;
#52565 = CARTESIAN_POINT ( 'NONE',  ( -3.108787716482549701, -6.376774720514417183, 20.32624910079993086 ) ) ;
#52566 = FACE_OUTER_BOUND ( 'NONE', #69651, .T. ) ;
#52567 = CARTESIAN_POINT ( 'NONE',  ( 2.499999999999988454, 22.00000000000000000, 2.100000000000000089 ) ) ;
#52568 = CARTESIAN_POINT ( 'NONE',  ( -25.53602269318328055, -24.91361206832937469, 5.313022737699515829 ) ) ;
#52569 = ORIENTED_EDGE ( 'NONE', *, *, #38465, .T. ) ;
#52570 = DIRECTION ( 'NONE',  ( 0.000000000000000000, 0.5144957554275265688, -0.8574929257125440962 ) ) ;
#52571 = CARTESIAN_POINT ( 'NONE',  ( -29.12273499046074221, -25.26247934485601832, 7.596950907507011408 ) ) ;
#52572 = CARTESIAN_POINT ( 'NONE',  ( 14.06386034339543478, -15.33156129944631729, 11.49999999999998934 ) ) ;
#52573 = ORIENTED_EDGE ( 'NONE', *, *, #41531, .F. ) ;
#52575 = EDGE_LOOP ( 'NONE', ( #66449, #5146, #53719, #10365 ) ) ;
#52574 = CARTESIAN_POINT ( 'NONE',  ( 4.653515142448186204, -6.376774720514413630, 19.86181745814487343 ) ) ;
#52576 = LINE ( 'NONE', #20123, #79521 ) ;
#52577 = ORIENTED_EDGE ( 'NONE', *, *, #50823, .T. ) ;
#52578 = EDGE_LOOP ( 'NONE', ( #56312, #50390, #50599, #77484 ) ) ;
#52579 = CARTESIAN_POINT ( 'NONE',  ( 7.423834877195115922, 10.77516967368741163, -0.9427051940160163790 ) ) ;
#52580 = CARTESIAN_POINT ( 'NONE',  ( -117.0508404609613251, -25.24693487555287064, 3.801655821953186631 ) ) ;
#52581 = CARTESIAN_POINT ( 'NONE',  ( 22.02124265030973760, -5.356774720514425603, 12.85402280011862430 ) ) ;
#52582 = CARTESIAN_POINT ( 'NONE',  ( -99.64934318012689118, -29.50249369713380077, 4.927347193923941049 ) ) ;
#52584 = ORIENTED_EDGE ( 'NONE', *, *, #85027, .T. ) ;
#52583 = CARTESIAN_POINT ( 'NONE',  ( -16.97254739485517661, -14.18817111035334655, 11.49999999999999645 ) ) ;
#52585 = FACE_OUTER_BOUND ( 'NONE', #64697, .T. ) ;
#52586 = CARTESIAN_POINT ( 'NONE',  ( 17.19246737676917292, 14.74310579602587090, -1.500000000000002220 ) ) ;
#52588 = ORIENTED_EDGE ( 'NONE', *, *, #1246, .T. ) ;
#52587 = CARTESIAN_POINT ( 'NONE',  ( -92.52287095715006160, -24.34917612407051379, 0.1852690917482314736 ) ) ;
#52589 = EDGE_CURVE ( 'NONE', #82121, #82898, #49601, .T. ) ;
#52590 = ORIENTED_EDGE ( 'NONE', *, *, #58665, .F. ) ;
#52591 = AXIS2_PLACEMENT_3D ( 'NONE', #1708, #94039, #92534 ) ;
#52592 = B_SPLINE_CURVE_WITH_KNOTS ( 'NONE', 3,
 ( #88870, #19340, #81243, #12218, #43195, #74135 ),
 .UNSPECIFIED., .F., .F.,
 ( 4, 2, 4 ),
 ( 0.000000000000000000, 0.001380764517854764532, 0.002761529035709529064 ),
 .UNSPECIFIED. ) ;
#52593 = DIRECTION ( 'NONE',  ( -0.9952638024365005887, 0.000000000000000000, -0.09721092304694052555 ) ) ;
#52594 = EDGE_CURVE ( 'NONE', #91590, #75060, #19124, .T. ) ;
#52595 = EDGE_CURVE ( 'NONE', #97022, #43843, #55976, .T. ) ;
#52596 = CARTESIAN_POINT ( 'NONE',  ( -4.889416449700032530, -19.50743224814450016, -1.500000000000002220 ) ) ;
#52597 = B_SPLINE_SURFACE_WITH_KNOTS ( 'NONE', 3, 3, ( 
 ( #3991, #74001, #41561, #4494 ),
 ( #18211, #49183, #88231, #94831 ),
 ( #34934, #80107, #96827, #87219 ),
 ( #17713, #72509, #48683, #3002 ),
 ( #50169, #79606, #41055, #11587 ),
 ( #49677, #80604, #11096, #42564 ),
 ( #37432, #99315, #74488, #60779 ),
 ( #82107, #14076, #83085, #84094 ),
 ( #97330, #90716, #66410, #58771 ),
 ( #45550, #12588, #29808, #97821 ) ),
 .UNSPECIFIED., .F., .F., .F.,
 ( 4, 3, 3, 4 ),
 ( 4, 4 ),
 ( 0.7022005934544808259, 0.7765311282028795059, 0.8508616629512781859, 0.9995227324480754350 ),
 ( 0.1995180756172104108, 0.2006497107716917472 ),
 .UNSPECIFIED. ) ;
#52598 = CARTESIAN_POINT ( 'NONE',  ( -36.62287095715004170, -23.47596703998600276, 11.44779298504227505 ) ) ;
#52599 = ORIENTED_EDGE ( 'NONE', *, *, #56569, .T. ) ;
#52600 = FACE_OUTER_BOUND ( 'NONE', #11270, .T. ) ;
#52601 = CARTESIAN_POINT ( 'NONE',  ( 5.437191932089902480, -21.69250089042843754, -1.500000000000002220 ) ) ;
#52602 = ORIENTED_EDGE ( 'NONE', *, *, #1438, .F. ) ;
#52603 = ORIENTED_EDGE ( 'NONE', *, *, #4292, .T. ) ;
#52604 = CARTESIAN_POINT ( 'NONE',  ( 9.940598223437573822, -5.876774720514426953, 18.21871304725684837 ) ) ;
#52605 = DIRECTION ( 'NONE',  ( -3.773278334453079618E-23, 0.9999999999976377785, 2.173523156925979975E-06 ) ) ;
#52606 = DIRECTION ( 'NONE',  ( -0.9978940991575084851, -0.000000000000000000, -0.06486421869277853025 ) ) ;
#52607 = CARTESIAN_POINT ( 'NONE',  ( -96.62287095715005592, -23.48786465467241413, 11.44779295918254114 ) ) ;
#52608 = DIRECTION ( 'NONE',  ( 0.6599726524652352877, 0.000000000000000000, -0.7512896232465891000 ) ) ;
#52609 = CARTESIAN_POINT ( 'NONE',  ( 0.4223197742854877812, 19.52780805513575402, -1.500000000000002220 ) ) ;
#52610 = CARTESIAN_POINT ( 'NONE',  ( -47.52287095715006160, -24.65952944569304606, 1.056160979905693686 ) ) ;
#52611 = CARTESIAN_POINT ( 'NONE',  ( -16.43003769262999469, -13.82051474754189258, 11.49999999999998934 ) ) ;
#52612 = CARTESIAN_POINT ( 'NONE',  ( -25.53214279450137170, -24.58000196289700057, 4.846047347457761667 ) ) ;
#52613 = CARTESIAN_POINT ( 'NONE',  ( -90.52287095715006160, -29.50248789122583659, 2.256150453626215580 ) ) ;
#52614 = LINE ( 'NONE', #28777, #40940 ) ;
#52616 = VECTOR ( 'NONE', #12203, 1000.000000000000114 ) ;
#52615 = CARTESIAN_POINT ( 'NONE',  ( 4.317061085376620255, -22.40314112565372540, -1.500000000000002220 ) ) ;
#52617 = EDGE_CURVE ( 'NONE', #85384, #14389, #30733, .T. ) ;
#52618 = APPROVAL_STATUS ( 'not_yet_approved' ) ;
#52619 = CARTESIAN_POINT ( 'NONE',  ( -96.51073854974256960, -24.35071581493543391, 9.817618358456023486 ) ) ;
#52620 = FACE_OUTER_BOUND ( 'NONE', #60611, .T. ) ;
#52621 = CARTESIAN_POINT ( 'NONE',  ( -12.72357806474857966, 15.40231687525621318, 11.49999999999999645 ) ) ;
#52622 = LINE ( 'NONE', #53637, #92167 ) ;
#52623 = CARTESIAN_POINT ( 'NONE',  ( -74.58126559791662658, -24.66019654487199730, 8.947790411086108620 ) ) ;
#52624 = CARTESIAN_POINT ( 'NONE',  ( -17.66201745896767505, 0.3587747205144061202, -23.06272557202527906 ) ) ;
#52625 = ORIENTED_EDGE ( 'NONE', *, *, #57672, .F. ) ;
#52626 = CARTESIAN_POINT ( 'NONE',  ( -56.62287095715005592, -23.47593901973091235, -1.443836447539007972 ) ) ;
#52627 = CARTESIAN_POINT ( 'NONE',  ( 10.73203334292264088, -3.902996417034998000, -26.95265065337511601 ) ) ;
#52628 = VECTOR ( 'NONE', #85246, 1000.000000000000114 ) ;
#52629 = CARTESIAN_POINT ( 'NONE',  ( -6.878457297428972161, 20.61903435171069532, 11.49999999999998934 ) ) ;
#52630 = EDGE_CURVE ( 'NONE', #62142, #53704, #75900, .T. ) ;
#52631 = CARTESIAN_POINT ( 'NONE',  ( -66.22287095715006444, -23.47596703998600276, 11.44779298504227860 ) ) ;
#52632 = CARTESIAN_POINT ( 'NONE',  ( -10.82925958622295859, 16.30987832687952022, -1.500000000000002220 ) ) ;
#52633 = CARTESIAN_POINT ( 'NONE',  ( -100.3728165607841447, -25.13336937450139175, 7.100323077445898079 ) ) ;
#52635 = EDGE_LOOP ( 'NONE', ( #63322, #65187, #5874, #31984 ) ) ;
#52634 = B_SPLINE_CURVE_WITH_KNOTS ( 'NONE', 3,
 ( #63860, #94774, #9040, #93774, #92766, #54234 ),
 .UNSPECIFIED., .F., .F.,
 ( 4, 2, 4 ),
 ( 6.384118678617699402E-06, 0.001386860460828380189, 0.002767336802978142760 ),
 .UNSPECIFIED. ) ;
#52636 = ADVANCED_FACE ( 'NONE', ( #60703 ), #84516, .T. ) ;
#52637 = CARTESIAN_POINT ( 'NONE',  ( 14.52511747680497933, -5.965225279485572685, -27.86035006098926559 ) ) ;
#52638 = CARTESIAN_POINT ( 'NONE',  ( 3.632573734185411851, -5.876774720514429617, 21.82795992345630509 ) ) ;
#52639 = CARTESIAN_POINT ( 'NONE',  ( 18.57849760351508195, 8.651319581928444080, 11.49999999999999645 ) ) ;
#52640 = FACE_OUTER_BOUND ( 'NONE', #36326, .T. ) ;
#52641 = CARTESIAN_POINT ( 'NONE',  ( -40.58953762381673158, -23.48783264082478084, -1.443836473390072817 ) ) ;
#52642 = B_SPLINE_CURVE_WITH_KNOTS ( 'NONE', 3,
 ( #16977, #38316, #61185, #23580, #92106, #22573, #77864, #78864 ),
 .UNSPECIFIED., .F., .F.,
 ( 4, 2, 2, 4 ),
 ( -0.001240355328176663422, -0.0002398155169398021556, 0.0007607242942970591105, 0.002761803916770780992 ),
 .UNSPECIFIED. ) ;
#52643 = ORIENTED_EDGE ( 'NONE', *, *, #73738, .F. ) ;
#52644 = CARTESIAN_POINT ( 'NONE',  ( 27.53860345374808105, -4.772774720514425972, -6.982392034746241372 ) ) ;
#52645 = CYLINDRICAL_SURFACE ( 'NONE', #73693, 1.325999999999990298 ) ;
#52646 = FACE_OUTER_BOUND ( 'NONE', #65061, .T. ) ;
#52647 = ADVANCED_FACE ( 'NONE', ( #99721 ), #13502, .F. ) ;
#52648 = CARTESIAN_POINT ( 'NONE',  ( -85.62287095715005592, -29.50247984919015209, -1.443849546365051806 ) ) ;
#52649 = ORIENTED_EDGE ( 'NONE', *, *, #77818, .F. ) ;
#52650 = LINE ( 'NONE', #68870, #62553 ) ;
#52651 = CARTESIAN_POINT ( 'NONE',  ( -10.12245940999746985, -20.73198382670940987, 11.49999999999999645 ) ) ;
#52652 = CARTESIAN_POINT ( 'NONE',  ( -7.601706241105644857, -21.46296766604531570, -1.500000000000002220 ) ) ;
#52653 = CARTESIAN_POINT ( 'NONE',  ( -70.50669286463424612, -25.31517374732275982, 4.857674065044717437 ) ) ;
#52654 = CARTESIAN_POINT ( 'NONE',  ( -105.6228709571500559, -24.91544648472627088, 1.928969306349436197 ) ) ;
#52655 = CARTESIAN_POINT ( 'NONE',  ( -98.52287095715007581, -23.47593901973090524, -1.443836447538996648 ) ) ;
#52656 = VECTOR ( 'NONE', #3238, 1000.000000000000000 ) ;
#52657 = DIRECTION ( 'NONE',  ( 0.000000000000000000, 1.000000000000000000, -0.000000000000000000 ) ) ;
#52658 = CARTESIAN_POINT ( 'NONE',  ( -110.6301004589282115, -24.15503026093913519, -0.2815557561904549755 ) ) ;
#52659 = CARTESIAN_POINT ( 'NONE',  ( 11.09338859787202480, -18.89396691112096605, 11.49999999999998934 ) ) ;
#52660 = ADVANCED_FACE ( 'NONE', ( #83012 ), #23100, .T. ) ;
#52661 = CARTESIAN_POINT ( 'NONE',  ( 3.176458874063931681, -0.3587747205143967943, -28.85257003503889806 ) ) ;
#52662 = B_SPLINE_CURVE_WITH_KNOTS ( 'NONE', 3,
 ( #83113, #44569, #77495, #9499, #24716, #17615, #18117, #70404, #78497, #1402, #40461, #33330, #47076, #55195 ),
 .UNSPECIFIED., .F., .F.,
 ( 4, 2, 2, 2, 2, 2, 4 ),
 ( 3.469446951953614189E-18, 0.0003991292329371358004, 0.0007982584658742681314, 0.001197387698811397914, 0.001596516931748527806, 0.002394775397622781951, 0.003193033863497036530 ),
 .UNSPECIFIED. ) ;
#52663 = CARTESIAN_POINT ( 'NONE',  ( -50.62287095715007723, -24.83602698348159876, 1.605859176311268177 ) ) ;
#52664 = CARTESIAN_POINT ( 'NONE',  ( -41.42859576553861700, -25.30281640502126095, 4.441720959794929868 ) ) ;
#52665 = EDGE_CURVE ( 'NONE', #36333, #80276, #15448, .T. ) ;
#52666 = CARTESIAN_POINT ( 'NONE',  ( -78.55032942013556863, -24.15543982623907127, -0.2315651400026641771 ) ) ;
#52667 = CARTESIAN_POINT ( 'NONE',  ( -112.6228709571500559, -24.64898659630368272, 1.056161002820831474 ) ) ;
#52668 = CARTESIAN_POINT ( 'NONE',  ( -107.6228709571500701, -24.64965695001469115, 8.947790433994176951 ) ) ;
#52669 = ORIENTED_EDGE ( 'NONE', *, *, #76573, .T. ) ;
#52670 = CARTESIAN_POINT ( 'NONE',  ( -4.302178748239556150, -20.00421716419250373, -1.500000000000002220 ) ) ;
#52671 = VERTEX_POINT ( 'NONE', #6403 ) ;
#52672 = ORIENTED_EDGE ( 'NONE', *, *, #10138, .F. ) ;
#52673 = ORIENTED_EDGE ( 'NONE', *, *, #69956, .T. ) ;
#52674 = ORIENTED_EDGE ( 'NONE', *, *, #69988, .F. ) ;
#52675 = CARTESIAN_POINT ( 'NONE',  ( 21.63105218614105851, 7.968772182826888262, 11.49999999999998934 ) ) ;
#52677 = EDGE_CURVE ( 'NONE', #41225, #24356, #75399, .T. ) ;
#52676 = CARTESIAN_POINT ( 'NONE',  ( -35.52287095715006160, -24.83602698348240878, 1.605859176314146763 ) ) ;
#52678 = CARTESIAN_POINT ( 'NONE',  ( 6.697674113365701842, 19.09646837838083400, -1.500000000000002220 ) ) ;
#52679 = EDGE_LOOP ( 'NONE', ( #42161, #43719, #72400, #45699 ) ) ;
#52680 = CARTESIAN_POINT ( 'NONE',  ( -90.52287095715003318, -25.00182538069145366, 7.747789668545104647 ) ) ;
#52681 = PLANE ( 'NONE',  #22236 ) ;
#52682 = EDGE_CURVE ( 'NONE', #80276, #36333, #30011, .T. ) ;
#52683 = CARTESIAN_POINT ( 'NONE',  ( -127.6228709571500559, -23.47596703998600631, 11.44779298504227860 ) ) ;
#52684 = CARTESIAN_POINT ( 'NONE',  ( -99.63465650044997801, -23.73791477778911840, 11.05961554403170410 ) ) ;
#52686 = VERTEX_POINT ( 'NONE', #67313 ) ;
#52685 = CARTESIAN_POINT ( 'NONE',  ( -2.231587876719630437, -21.34735720706076378, 11.49999999999999645 ) ) ;
#52687 = CARTESIAN_POINT ( 'NONE',  ( -128.6228709571500417, -23.47593901973091235, -1.443836447538995760 ) ) ;
#52688 = DIRECTION ( 'NONE',  ( -4.163336342344339393E-15, 0.000000000000000000, -1.000000000000000000 ) ) ;
#52689 = EDGE_LOOP ( 'NONE', ( #76265, #14240, #46420, #35753 ) ) ;
#52690 = CARTESIAN_POINT ( 'NONE',  ( -1.843323519027639357, -20.62917239659568835, -1.500000000000002220 ) ) ;
#52691 = AXIS2_PLACEMENT_3D ( 'NONE', #11595, #33438, #3999 ) ;
#52692 = B_SPLINE_CURVE_WITH_KNOTS ( 'NONE', 3,
 ( #9466, #43298, #2366, #56661 ),
 .UNSPECIFIED., .F., .F.,
 ( 4, 4 ),
 ( 2.778582473997085907E-06, 0.0004643190030723578360 ),
 .UNSPECIFIED. ) ;
#52694 = VERTEX_POINT ( 'NONE', #5897 ) ;
#52693 = CARTESIAN_POINT ( 'NONE',  ( -80.62287095715004170, -23.48783264082478439, -1.443836473390065489 ) ) ;
#52695 = CARTESIAN_POINT ( 'NONE',  ( -28.64432147930652661, -24.00272683650521088, -0.2315644524145782090 ) ) ;
#52696 = VERTEX_POINT ( 'NONE', #44974 ) ;
#52697 = CARTESIAN_POINT ( 'NONE',  ( 3.797776442307698286, -6.376774720514401196, 18.16025641025640525 ) ) ;
#52698 = ORIENTED_EDGE ( 'NONE', *, *, #20476, .T. ) ;
#52699 = CARTESIAN_POINT ( 'NONE',  ( -20.97355972163249049, 0.1317905507124840780, -1.500000000000002220 ) ) ;
#52700 = CARTESIAN_POINT ( 'NONE',  ( 12.93620265873104991, 17.78788284566447331, 11.49999999999999645 ) ) ;
#52701 = VECTOR ( 'NONE', #71180, 1000.000000000000114 ) ;
#52702 = CARTESIAN_POINT ( 'NONE',  ( -37.58684943389518196, -24.35071581493542325, 9.817618358456030592 ) ) ;
#52703 = CARTESIAN_POINT ( 'NONE',  ( 22.38532167473930556, -2.757513164441831144, 11.49999999999998934 ) ) ;
#52704 = AXIS2_PLACEMENT_3D ( 'NONE', #14970, #45942, #60675 ) ;
#52705 = CARTESIAN_POINT ( 'NONE',  ( -9.893913718187896222, 18.50344063021147889, 11.49999999999998934 ) ) ;
#52706 = CARTESIAN_POINT ( 'NONE',  ( -48.58953762381671737, -23.48783264082478439, -1.443836473390070596 ) ) ;
#52707 = B_SPLINE_CURVE_WITH_KNOTS ( 'NONE', 3,
 ( #17171, #41521, #93795, #9559, #87187, #79573 ),
 .UNSPECIFIED., .F., .F.,
 ( 4, 2, 4 ),
 ( 1.570755371634170283E-05, 0.001396183895866089488, 0.002776660238015837313 ),
 .UNSPECIFIED. ) ;
#52708 = CARTESIAN_POINT ( 'NONE',  ( -45.62287095715004881, -29.50250786944525672, 11.44777988621624054 ) ) ;
#52710 = EDGE_CURVE ( 'NONE', #42982, #73818, #10618, .T. ) ;
#52709 = CARTESIAN_POINT ( 'NONE',  ( 6.403846153846157740, -6.376774720514426065, 21.48076923076922995 ) ) ;
#52711 = ORIENTED_EDGE ( 'NONE', *, *, #67383, .F. ) ;
#52712 = EDGE_LOOP ( 'NONE', ( #76492, #71917, #40657, #84207, #78981, #59053 ) ) ;
#52713 = ORIENTED_EDGE ( 'NONE', *, *, #61834, .T. ) ;
#52714 = CARTESIAN_POINT ( 'NONE',  ( 7.749999999999998224, 25.69999999999999574, 2.100000000000000089 ) ) ;
#52715 = CARTESIAN_POINT ( 'NONE',  ( -0.8555947871142663974, 21.52075748220454798, -1.500000000000002220 ) ) ;
#52716 = ADVANCED_FACE ( 'NONE', ( #29235 ), #76882, .F. ) ;
#52717 = DIRECTION ( 'NONE',  ( -1.000000000000000000, 0.000000000000000000, 0.000000000000000000 ) ) ;
#52718 = ORIENTED_EDGE ( 'NONE', *, *, #13328, .F. ) ;
#52719 = CARTESIAN_POINT ( 'NONE',  ( 13.68530018921192060, -16.06810839794082924, 11.49999999999998934 ) ) ;
#52720 = DIRECTION ( 'NONE',  ( 3.773278334444167608E-23, -1.000000000000000000, 0.000000000000000000 ) ) ;
#52721 = DIRECTION ( 'NONE',  ( 0.000000000000000000, 0.000000000000000000, 1.000000000000000000 ) ) ;
#52722 = CARTESIAN_POINT ( 'NONE',  ( -83.50067839706997574, -24.66019654487199375, 8.947790411086122830 ) ) ;
#52723 = DIRECTION ( 'NONE',  ( -0.1478094111296165691, 0.9890158633619158257, -0.000000000000000000 ) ) ;
#52724 = CARTESIAN_POINT ( 'NONE',  ( -41.62287095715006302, -23.47593901973091235, -1.443836447539011525 ) ) ;
#52725 = CARTESIAN_POINT ( 'NONE',  ( -16.08457400211760913, 15.13120210334024662, -1.500000000000002220 ) ) ;
#52726 = CARTESIAN_POINT ( 'NONE',  ( 6.499999999999992895, 1.999999999999998668, 0.000000000000000000 ) ) ;
#52727 = VERTEX_POINT ( 'NONE', #91132 ) ;
#52728 = FACE_OUTER_BOUND ( 'NONE', #97867, .T. ) ;
#52729 = CARTESIAN_POINT ( 'NONE',  ( 12.46431485231495806, 4.283161447665844612, -27.85634418129429690 ) ) ;
#52730 = CARTESIAN_POINT ( 'NONE',  ( 14.76093561896379214, 5.965225279485572685, -26.55548769130089681 ) ) ;
#52731 = CYLINDRICAL_SURFACE ( 'NONE', #83539, 6.000000000000000888 ) ;
#52732 = CARTESIAN_POINT ( 'NONE',  ( 16.42231304340664266, 10.40281881132301045, -1.500000000000002220 ) ) ;
#52733 = AXIS2_PLACEMENT_3D ( 'NONE', #42929, #24804, #2488 ) ;
#52734 = CARTESIAN_POINT ( 'NONE',  ( -20.23222619987061677, -6.887663580918623296, -1.500000000000002220 ) ) ;
#52735 = CARTESIAN_POINT ( 'NONE',  ( -69.47951456376665647, -25.09778000710391765, 7.297977585176790072 ) ) ;
#52736 = CARTESIAN_POINT ( 'NONE',  ( -1.751198251822016161, 22.56127314141087581, 0.000000000000000000 ) ) ;
#52737 = CARTESIAN_POINT ( 'NONE',  ( -73.62287095715005592, -24.64898659630367916, 1.056161002820824368 ) ) ;
#52738 = CARTESIAN_POINT ( 'NONE',  ( -36.62287095715007013, -24.35013146730203459, 9.818937971375119034 ) ) ;
#52739 = CARTESIAN_POINT ( 'NONE',  ( -1.322449806865925614, 22.60218017400935864, -1.500000000000002220 ) ) ;
#52740 = EDGE_CURVE ( 'NONE', #20076, #83403, #36645, .T. ) ;
#52741 = ORIENTED_EDGE ( 'NONE', *, *, #33526, .F. ) ;
#52742 = CARTESIAN_POINT ( 'NONE',  ( -128.5895376238167103, -24.65952944569305316, 1.056160979905707897 ) ) ;
#52743 = DIRECTION ( 'NONE',  ( 0.4561809899890718056, 0.000000000000000000, -0.8898870177570803452 ) ) ;
#52744 = CARTESIAN_POINT ( 'NONE',  ( -2.602694502683683631, -19.63732897141692391, 11.49999999999999645 ) ) ;
#52745 = B_SPLINE_CURVE_WITH_KNOTS ( 'NONE', 3,
 ( #10046, #73453, #96287, #56246, #18159, #17659 ),
 .UNSPECIFIED., .F., .F.,
 ( 4, 2, 4 ),
 ( 6.384118696097665072E-06, 0.001386860460837120376, 0.002767336802978143193 ),
 .UNSPECIFIED. ) ;
#52746 = CARTESIAN_POINT ( 'NONE',  ( -94.52287095715006160, -29.50250786944525672, 11.44777988621623344 ) ) ;
#52747 = ORIENTED_EDGE ( 'NONE', *, *, #78299, .T. ) ;
#52748 = CARTESIAN_POINT ( 'NONE',  ( -99.62287095715005592, -29.50250243563736774, 8.947779886222138046 ) ) ;
#52750 = EDGE_CURVE ( 'NONE', #23691, #74060, #83515, .T. ) ;
#52749 = CARTESIAN_POINT ( 'NONE',  ( -115.6228709571500701, -25.00158670708909625, 2.256160236439165967 ) ) ;
#52751 = CARTESIAN_POINT ( 'NONE',  ( -8.642975711230413083, 19.83371042614930957, -1.500000000000002220 ) ) ;
#52752 = EDGE_CURVE ( 'NONE', #23327, #82927, #84015, .T. ) ;
#52753 = CARTESIAN_POINT ( 'NONE',  ( -41.52287095715006870, -29.50250243563736774, 8.947779886222148704 ) ) ;
#52754 = CARTESIAN_POINT ( 'NONE',  ( -11.04204518803028456, 15.98388583709530941, -1.500000000000002220 ) ) ;
#52755 = EDGE_CURVE ( 'NONE', #72664, #36632, #86252, .T. ) ;
#52756 = CARTESIAN_POINT ( 'NONE',  ( -61.62287095715004170, -23.73907113216991505, -1.053371485793230589 ) ) ;
#52757 = CARTESIAN_POINT ( 'NONE',  ( -27.83739072329610664, 0.3587747205143967943, -8.084349702057700426 ) ) ;
#52758 = CARTESIAN_POINT ( 'NONE',  ( 10.49454761162020588, -16.79419365751139637, 11.49999999999998934 ) ) ;
#52759 = ORIENTED_EDGE ( 'NONE', *, *, #40430, .F. ) ;
#52760 = EDGE_CURVE ( 'NONE', #79973, #35655, #62482, .T. ) ;
#52761 = CARTESIAN_POINT ( 'NONE',  ( -8.348131891436525009, -18.51812344263101906, 11.49999999999999645 ) ) ;
#52762 = CARTESIAN_POINT ( 'NONE',  ( -80.62685931099697711, -24.83618233451450408, 1.606449574219532384 ) ) ;
#52763 = AXIS2_PLACEMENT_3D ( 'NONE', #60134, #21532, #52509 ) ;
#52764 = AXIS2_PLACEMENT_3D ( 'NONE', #43935, #24077, #47430 ) ;
#52765 = CARTESIAN_POINT ( 'NONE',  ( 33.54680291763921929, -3.871631182425088191, -11.45966867074879580 ) ) ;
#52766 = ORIENTED_EDGE ( 'NONE', *, *, #5101, .T. ) ;
#52767 = CARTESIAN_POINT ( 'NONE',  ( -102.6335722854369266, -23.73791477778911840, 11.05961554403170410 ) ) ;
#52768 = CARTESIAN_POINT ( 'NONE',  ( -116.4728709571500502, -25.21147115889351298, 5.000950864497187176 ) ) ;
#52769 = CARTESIAN_POINT ( 'NONE',  ( -27.86046284349297864, 5.965225279485572685, -8.091963836038754465 ) ) ;
#52770 = CARTESIAN_POINT ( 'NONE',  ( -28.32169924589829080, -5.965225279485592225, -8.244178532169447848 ) ) ;
#52771 = AXIS2_PLACEMENT_3D ( 'NONE', #6038, #44112, #52721 ) ;
#52772 = DIRECTION ( 'NONE',  ( -0.000000000000000000, -0.000000000000000000, -1.000000000000000000 ) ) ;
#52773 = CARTESIAN_POINT ( 'NONE',  ( -14.83682921977595548, 13.52632505182701017, 11.49999999999998934 ) ) ;
#52774 = EDGE_CURVE ( 'NONE', #30745, #63171, #39340, .T. ) ;
#52775 = ADVANCED_FACE ( 'NONE', ( #32223 ), #8392, .F. ) ;
#52776 = AXIS2_PLACEMENT_3D ( 'NONE', #4503, #94901, #92891 ) ;
#52777 = CARTESIAN_POINT ( 'NONE',  ( 29.73860345376319003, -1.682774720514426114, -8.849814207987163783 ) ) ;
#52778 = VERTEX_POINT ( 'NONE', #77887 ) ;
#52779 = LINE ( 'NONE', #23302, #28501 ) ;
#52780 = VECTOR ( 'NONE', #79836, 1000.000000000000114 ) ;
#52781 = CARTESIAN_POINT ( 'NONE',  ( 17.58993269669914383, -14.52173041563253975, 11.49999999999999645 ) ) ;
#52782 = CARTESIAN_POINT ( 'NONE',  ( -49.57368764975930731, -25.31297113922084208, 4.259411968733069820 ) ) ;
#52783 = DIRECTION ( 'NONE',  ( -3.773278334453079618E-23, 0.9999999999976377785, 2.173523156925978705E-06 ) ) ;
#52784 = CARTESIAN_POINT ( 'NONE',  ( -114.5895376238166961, -24.65952944569305316, 1.056160979905700570 ) ) ;
#52785 = CARTESIAN_POINT ( 'NONE',  ( 5.671135738765417322, -5.876774720514422512, 20.99074880795119924 ) ) ;
#52786 = EDGE_CURVE ( 'NONE', #34762, #56620, #38841, .T. ) ;
#52787 = CARTESIAN_POINT ( 'NONE',  ( -10.34999999999999254, 2.239999999999997105, 2.100000000000000977 ) ) ;
#52788 = CARTESIAN_POINT ( 'NONE',  ( 0.000000000000000000, -4.056774720514426669, 0.000000000000000000 ) ) ;
#52789 = VERTEX_POINT ( 'NONE', #62197 ) ;
#52790 = CARTESIAN_POINT ( 'NONE',  ( -20.29798418530817017, 1.744846428065259136, -1.500000000000002220 ) ) ;
#52791 = ORIENTED_EDGE ( 'NONE', *, *, #86089, .F. ) ;
#52792 = CARTESIAN_POINT ( 'NONE',  ( 3.929728083993185184, -22.62717521373229701, -1.500000000000002220 ) ) ;
#52793 = EDGE_CURVE ( 'NONE', #30324, #18231, #7532, .T. ) ;
#52794 = FACE_OUTER_BOUND ( 'NONE', #79618, .T. ) ;
#52795 = EDGE_LOOP ( 'NONE', ( #84807, #695, #61398, #85457, #38447, #71778, #77791, #92686, #27854, #64626, #63133, #68776, #14482, #33427, #61612, #38926, #48357 ) ) ;
#52796 = CARTESIAN_POINT ( 'NONE',  ( -101.3869470976398333, -25.19665614377478136, 6.627173498926840267 ) ) ;
#52797 = EDGE_CURVE ( 'NONE', #82714, #21186, #81406, .T. ) ;
#52798 = CARTESIAN_POINT ( 'NONE',  ( -77.54619546820211440, -24.35071581493544102, 9.817618358456021710 ) ) ;
#52799 = EDGE_CURVE ( 'NONE', #68647, #57214, #26772, .T. ) ;
#52800 = CARTESIAN_POINT ( 'NONE',  ( -51.64512824026234483, -23.96169478059713143, 10.65365249895718236 ) ) ;
#52802 = ORIENTED_EDGE ( 'NONE', *, *, #67835, .T. ) ;
#52801 = CARTESIAN_POINT ( 'NONE',  ( 15.87343765641381665, 14.11872912734625274, 11.49999999999999645 ) ) ;
#52803 = AXIS2_PLACEMENT_3D ( 'NONE', #48293, #16326, #92443 ) ;
#52804 = ORIENTED_EDGE ( 'NONE', *, *, #80816, .F. ) ;
#52805 = CARTESIAN_POINT ( 'NONE',  ( 10.53326394202159300, -19.55463526559320542, -1.500000000000002220 ) ) ;
#52806 = CARTESIAN_POINT ( 'NONE',  ( -11.82494684808912844, 16.90534455221803967, 11.49999999999998934 ) ) ;
#52807 = VERTEX_POINT ( 'NONE', #9389 ) ;
#52808 = ORIENTED_EDGE ( 'NONE', *, *, #74911, .F. ) ;
#52809 = CARTESIAN_POINT ( 'NONE',  ( 6.480733632922428988, -6.376774720514426065, 21.47849199606610782 ) ) ;
#52810 = EDGE_CURVE ( 'NONE', #85607, #14971, #40248, .T. ) ;
#52811 = CARTESIAN_POINT ( 'NONE',  ( -40.07214526342530547, -25.12798243322264469, 2.874043696753044053 ) ) ;
#52812 = VERTEX_POINT ( 'NONE', #33229 ) ;
#52813 = VERTEX_POINT ( 'NONE', #15994 ) ;
#52814 = DIRECTION ( 'NONE',  ( 0.000000000000000000, 0.000000000000000000, -1.000000000000000000 ) ) ;
#52815 = FACE_OUTER_BOUND ( 'NONE', #26073, .T. ) ;
#52816 = CARTESIAN_POINT ( 'NONE',  ( -18.54028579900546703, -9.471972883075929772, -1.500000000000002220 ) ) ;
#52817 = CARTESIAN_POINT ( 'NONE',  ( 6.711561834375728175, -20.75310922853297058, 11.49999999999999645 ) ) ;
#52818 = CARTESIAN_POINT ( 'NONE',  ( -39.58615480296015221, -25.23770002871814455, 3.714675945737659912 ) ) ;
#52819 = CARTESIAN_POINT ( 'NONE',  ( -89.81226385320383088, -29.50249166729307149, 3.993452963156916002 ) ) ;
#52820 = CARTESIAN_POINT ( 'NONE',  ( -3.368041826647835357, -22.21310627845187824, -1.500000000000002220 ) ) ;
#52821 = CARTESIAN_POINT ( 'NONE',  ( -50.72939492065860634, -25.31296752812565387, 4.679804727249790908 ) ) ;
#52822 = ORIENTED_EDGE ( 'NONE', *, *, #603, .F. ) ;
#52823 = CARTESIAN_POINT ( 'NONE',  ( 15.14080536460164517, 5.152774720514427642, -26.62908960815038384 ) ) ;
#52824 = CARTESIAN_POINT ( 'NONE',  ( 32.33408272158504815, 4.458032690740698634, 0.9207958043952065852 ) ) ;
#52825 = EDGE_LOOP ( 'NONE', ( #80089, #20399, #21991, #86950 ) ) ;
#52826 = EDGE_LOOP ( 'NONE', ( #58719, #65682, #10720, #95866 ) ) ;
#52827 = CARTESIAN_POINT ( 'NONE',  ( -46.56868764939927985, -23.48786465467240703, 11.44779295918255180 ) ) ;
#52828 = EDGE_LOOP ( 'NONE', ( #24979, #53495, #86203, #55082 ) ) ;
#52829 = VECTOR ( 'NONE', #55294, 1000.000000000000000 ) ;
#52830 = CARTESIAN_POINT ( 'NONE',  ( 20.90283063341239966, -4.354886778353011856, -1.500000000000002220 ) ) ;
#52831 = ORIENTED_EDGE ( 'NONE', *, *, #68687, .F. ) ;
#52832 = CARTESIAN_POINT ( 'NONE',  ( -5.926585084595196840, -5.876774720514416295, 20.19722303762275573 ) ) ;
#52833 = VECTOR ( 'NONE', #52839, 1000.000000000000000 ) ;
#52834 = CARTESIAN_POINT ( 'NONE',  ( 4.297136154115697160, 20.59472113332480703, 11.49999999999998934 ) ) ;
#52835 = CARTESIAN_POINT ( 'NONE',  ( -30.54993633120672314, -24.48461703701380543, 0.5642940035406466270 ) ) ;
#52836 = CARTESIAN_POINT ( 'NONE',  ( -41.46524908126663433, -25.18431059086284307, 4.157779966712787711 ) ) ;
#52837 = CARTESIAN_POINT ( 'NONE',  ( -79.11611000704996854, -25.15699314367416051, 3.101158825156976828 ) ) ;
#52838 = CARTESIAN_POINT ( 'NONE',  ( -17.52905966558703454, -13.16386835867055716, -1.500000000000002220 ) ) ;
#52839 = DIRECTION ( 'NONE',  ( -0.9496245541219264785, -6.845827386180410961E-16, -0.3133898629642195011 ) ) ;
#52840 = ORIENTED_EDGE ( 'NONE', *, *, #40173, .T. ) ;
#52841 = B_SPLINE_CURVE_WITH_KNOTS ( 'NONE', 3,
 ( #62139, #31672, #16440, #40294, #47911, #25056 ),
 .UNSPECIFIED., .F., .F.,
 ( 4, 2, 4 ),
 ( 1.570755371633777598E-05, 0.001396183895866085151, 0.002776660238015832543 ),
 .UNSPECIFIED. ) ;
#52842 = CARTESIAN_POINT ( 'NONE',  ( -122.5214654115758037, -23.73791477778912551, 11.05961554403169878 ) ) ;
#52843 = CIRCLE ( 'NONE', #86868, 1.306876713926001798 ) ;
#52844 = VECTOR ( 'NONE', #79851, 1000.000000000000114 ) ;
#52845 = CARTESIAN_POINT ( 'NONE',  ( -84.59526703719879492, -23.96169478059713498, 10.65365249895717881 ) ) ;
#52846 = CARTESIAN_POINT ( 'NONE',  ( -128.5228709571500758, -24.65952944569305316, 1.056160979905707675 ) ) ;
#52847 = CARTESIAN_POINT ( 'NONE',  ( -30.60198721217873796, -24.75207560356990300, 8.640809912072075605 ) ) ;
#52848 = CARTESIAN_POINT ( 'NONE',  ( 14.64190796094839264, -15.47823801613018269, 11.49999999999998934 ) ) ;
#52849 = CARTESIAN_POINT ( 'NONE',  ( -112.5553945339797508, -23.96119346886881729, -0.6495511937831841554 ) ) ;
#52850 = CARTESIAN_POINT ( 'NONE',  ( -20.77875734969026311, -6.143225279485574397, 27.35402280011862430 ) ) ;
#52851 = LINE ( 'NONE', #53360, #50225 ) ;
#52852 = CARTESIAN_POINT ( 'NONE',  ( -85.62287095714999907, -24.51254535404255108, 9.355368623467660072 ) ) ;
#52853 = B_SPLINE_CURVE_WITH_KNOTS ( 'NONE', 3,
 ( #63588, #70676, #32612, #79781 ),
 .UNSPECIFIED., .F., .F.,
 ( 4, 4 ),
 ( 1.387778780781445521E-17, 9.999999999997510880E-05 ),
 .UNSPECIFIED. ) ;
#52854 = CARTESIAN_POINT ( 'NONE',  ( -3.368041826647835357, -22.21310627845187824, -1.500000000000002220 ) ) ;
#52855 = EDGE_CURVE ( 'NONE', #85611, #68707, #58413, .T. ) ;
#52856 = CARTESIAN_POINT ( 'NONE',  ( -109.9096082921335125, -25.11552134530501590, 2.805129186380272088 ) ) ;
#52857 = ORIENTED_EDGE ( 'NONE', *, *, #92599, .F. ) ;
#52858 = EDGE_CURVE ( 'NONE', #12032, #26463, #80141, .T. ) ;
#52859 = CARTESIAN_POINT ( 'NONE',  ( -81.52287095715004739, -24.35013146730203815, 9.818937971375106599 ) ) ;
#52860 = CARTESIAN_POINT ( 'NONE',  ( 18.24213732562919787, -7.162457363581539838, 11.49999999999999645 ) ) ;
#52861 = DIRECTION ( 'NONE',  ( 3.496357139254347770E-15, -0.9940716917543757081, -0.1087265912856345829 ) ) ;
#52862 = EDGE_CURVE ( 'NONE', #937, #3121, #94123, .T. ) ;
#52863 = CARTESIAN_POINT ( 'NONE',  ( -100.6228709571500985, -24.51254535404255464, 9.355368623467651190 ) ) ;
#52864 = B_SPLINE_CURVE_WITH_KNOTS ( 'NONE', 3,
 ( #72118, #33044, #17820, #23917, #71614, #40663, #8205, #78196, #1600, #32540, #48787, #39144, #55897, #32037 ),
 .UNSPECIFIED., .F., .F.,
 ( 4, 2, 2, 2, 2, 2, 4 ),
 ( 8.673617379884035472E-19, 0.0001881572706675479123, 0.0003763145413350949572, 0.0007526290826701718083, 0.001128943624005248605, 0.001317100894672787112, 0.001505258165340325402 ),
 .UNSPECIFIED. ) ;
#52865 = ORIENTED_EDGE ( 'NONE', *, *, #44741, .F. ) ;
#52866 = EDGE_CURVE ( 'NONE', #52968, #14119, #14894, .T. ) ;
#52867 = CARTESIAN_POINT ( 'NONE',  ( -69.20785623293232902, -25.30035436060855503, 5.366416221723499191 ) ) ;
#52868 = CARTESIAN_POINT ( 'NONE',  ( -3.826923076923078426, -6.376774720514408301, 19.19230769230769695 ) ) ;
#52869 = DIRECTION ( 'NONE',  ( 0.000000000000000000, 1.000000000000000000, 0.000000000000000000 ) ) ;
#52870 = AXIS2_PLACEMENT_3D ( 'NONE', #55886, #86811, #40652 ) ;
#52871 = EDGE_CURVE ( 'NONE', #67215, #94249, #78391, .T. ) ;
#52872 = CARTESIAN_POINT ( 'NONE',  ( -116.6228709571500701, -23.48783264082478794, -1.443836473390058606 ) ) ;
#52873 = EDGE_CURVE ( 'NONE', #50095, #58927, #96140, .T. ) ;
#52874 = CARTESIAN_POINT ( 'NONE',  ( 2.169241753049089727, -19.58708112974024829, 11.49999999999998934 ) ) ;
#52875 = ORIENTED_EDGE ( 'NONE', *, *, #49972, .T. ) ;
#52876 = DIRECTION ( 'NONE',  ( 0.000000000000000000, -0.9999999999976377785, -2.173523156925979552E-06 ) ) ;
#52877 = PLANE ( 'NONE',  #99814 ) ;
#52878 = MECHANICAL_CONTEXT ( 'NONE', #9663, 'mechanical' ) ;
#52879 = ORIENTED_EDGE ( 'NONE', *, *, #68820, .F. ) ;
#52880 = CARTESIAN_POINT ( 'NONE',  ( -45.62287095715004881, -23.47593901973091235, -1.443836447539009749 ) ) ;
#52881 = CARTESIAN_POINT ( 'NONE',  ( -67.62287095715007013, -24.51283580621364422, 0.6167428607019762588 ) ) ;
#52882 = CARTESIAN_POINT ( 'NONE',  ( -90.62287095715004170, -23.48786465467241058, 11.44779295918254469 ) ) ;
#52883 = DIRECTION ( 'NONE',  ( 0.000000000000000000, -1.000000000000000000, 0.000000000000000000 ) ) ;
#52884 = CARTESIAN_POINT ( 'NONE',  ( -102.6228709571500559, -29.50248528299804818, 1.056150453629042030 ) ) ;
#52885 = DIRECTION ( 'NONE',  ( -0.2488812114211667037, 0.000000000000000000, -0.9685340172660599212 ) ) ;
#52886 = CARTESIAN_POINT ( 'NONE',  ( -91.52287095715001897, -23.95044443724991368, 10.65354141964648882 ) ) ;
#52887 = CARTESIAN_POINT ( 'NONE',  ( 19.98059151383774434, -0.7942727526097331792, -1.500000000000002220 ) ) ;
#52888 = EDGE_CURVE ( 'NONE', #29990, #45914, #11396, .T. ) ;
#52889 = CARTESIAN_POINT ( 'NONE',  ( -6.660000000000001030, -10.15233964170348457, 0.003711184059992174607 ) ) ;
#52890 = CARTESIAN_POINT ( 'NONE',  ( -45.54234093893470003, -24.40133493613049964, 9.663955038902802386 ) ) ;
#52891 = ORIENTED_EDGE ( 'NONE', *, *, #665, .F. ) ;
#52892 = DIRECTION ( 'NONE',  ( -3.469446951953614189E-15, 1.000000000000000000, 0.000000000000000000 ) ) ;
#52893 = AXIS2_PLACEMENT_3D ( 'NONE', #51760, #98408, #12681 ) ;
#52894 = B_SPLINE_CURVE_WITH_KNOTS ( 'NONE', 3,
 ( #67503, #74112, #83707, #6587, #45166, #83203, #4609, #74598 ),
 .UNSPECIFIED., .F., .F.,
 ( 4, 2, 2, 4 ),
 ( -0.001224873891641418489, -0.0002244903592271037251, 0.0007758931731872110386, 0.002776660238015837313 ),
 .UNSPECIFIED. ) ;
#52895 = B_SPLINE_CURVE_WITH_KNOTS ( 'NONE', 3,
 ( #86187, #16170, #86684, #10560 ),
 .UNSPECIFIED., .F., .F.,
 ( 4, 4 ),
 ( 0.4200858975343448876, 0.4290923288064604213 ),
 .UNSPECIFIED. ) ;
#52896 = EDGE_CURVE ( 'NONE', #86931, #89111, #62020, .T. ) ;
#52897 = CARTESIAN_POINT ( 'NONE',  ( 6.184520403203631389, -5.356774720514425603, -25.32021290018218451 ) ) ;
#52898 = CARTESIAN_POINT ( 'NONE',  ( -80.54557494822695674, -24.52399227489127043, 9.353111116836524630 ) ) ;
#52899 = CARTESIAN_POINT ( 'NONE',  ( -125.5798323200307891, -25.21791982601823534, 6.461802024446555492 ) ) ;
#52900 = CARTESIAN_POINT ( 'NONE',  ( -39.57598330014963040, -24.65952944569304250, 1.056160979905697017 ) ) ;
#52901 = DIRECTION ( 'NONE',  ( 1.000000000000000000, 3.773278334444166432E-23, 8.201307841325785021E-29 ) ) ;
#52902 = FACE_OUTER_BOUND ( 'NONE', #26244, .T. ) ;
#52903 = VECTOR ( 'NONE', #62010, 1000.000000000000000 ) ;
#52904 = DIRECTION ( 'NONE',  ( -0.000000000000000000, 1.000000000000000000, -0.000000000000000000 ) ) ;
#52906 = VECTOR ( 'NONE', #44189, 1000.000000000000114 ) ;
#52905 = DIRECTION ( 'NONE',  ( 1.000000000000000000, 3.773278334444166432E-23, 8.201307841325785021E-29 ) ) ;
#52907 = EDGE_LOOP ( 'NONE', ( #51909, #66567, #37582, #23450 ) ) ;
#52908 = VECTOR ( 'NONE', #6528, 1000.000000000000114 ) ;
#52909 = CARTESIAN_POINT ( 'NONE',  ( -3.766600276044322904, -19.90762401167813067, 11.49999999999998934 ) ) ;
#52910 = CARTESIAN_POINT ( 'NONE',  ( -69.20005239865344038, -25.31085673378436240, 5.363653916047343984 ) ) ;
#52911 = CARTESIAN_POINT ( 'NONE',  ( 3.180076745125948179, 5.965225279485592225, -28.87659520466657526 ) ) ;
#52912 = CIRCLE ( 'NONE', #78821, 4.080000000000000071 ) ;
#52913 = CARTESIAN_POINT ( 'NONE',  ( -35.62287095715005592, -29.50249982740957577, 7.747779886224967605 ) ) ;
#52914 = B_SPLINE_CURVE_WITH_KNOTS ( 'NONE', 3,
 ( #42185, #18814, #65528, #35054, #10211, #3610 ),
 .UNSPECIFIED., .F., .F.,
 ( 4, 2, 4 ),
 ( 0.000000000000000000, 0.001380764517854764532, 0.002761529035709529064 ),
 .UNSPECIFIED. ) ;
#52916 = EDGE_LOOP ( 'NONE', ( #17080, #26297, #22130, #15215 ) ) ;
#52915 = EDGE_CURVE ( 'NONE', #77171, #69148, #49980, .T. ) ;
#52917 = CARTESIAN_POINT ( 'NONE',  ( 22.02124265030973760, -6.143225279485574397, 18.45402280011862217 ) ) ;
#52918 = CARTESIAN_POINT ( 'NONE',  ( -61.62287095715004881, -23.47596703998600631, 11.44779298504227505 ) ) ;
#52919 = CARTESIAN_POINT ( 'NONE',  ( 12.55954966114946458, -15.69740789531843461, -1.500000000000002220 ) ) ;
#52920 = CARTESIAN_POINT ( 'NONE',  ( 5.245434476726341444, -20.39595507048906242, 11.49999999999999645 ) ) ;
#52921 = CARTESIAN_POINT ( 'NONE',  ( -32.52287095715006160, -24.65952944569304606, 1.056160979905690134 ) ) ;
#52922 = CARTESIAN_POINT ( 'NONE',  ( 19.10104996495751450, -11.12853483292915691, 11.49999999999998934 ) ) ;
#52923 = EDGE_CURVE ( 'NONE', #65066, #46259, #18717, .T. ) ;
#52924 = CARTESIAN_POINT ( 'NONE',  ( -18.81443736134900035, 8.205417114561466718, -1.500000000000002220 ) ) ;
#52925 = FACE_OUTER_BOUND ( 'NONE', #35368, .T. ) ;
#52926 = CARTESIAN_POINT ( 'NONE',  ( -60.49379600255042533, -24.52300882791528380, 0.6510814631126233820 ) ) ;
#52927 = EDGE_LOOP ( 'NONE', ( #99830, #41767, #68792, #95630 ) ) ;
#52928 = DIRECTION ( 'NONE',  ( -3.773278334453079030E-23, 0.9999999999976377785, 2.173523156925979128E-06 ) ) ;
#52929 = ORIENTED_EDGE ( 'NONE', *, *, #57370, .F. ) ;
#52930 = CARTESIAN_POINT ( 'NONE',  ( -89.40841769935769889, -25.27880950044345809, 5.947789066509453271 ) ) ;
#52931 = CARTESIAN_POINT ( 'NONE',  ( -67.62287095715005592, -24.64965695001468404, 8.947790433994184056 ) ) ;
#52932 = VERTEX_POINT ( 'NONE', #64718 ) ;
#52933 = B_SPLINE_CURVE_WITH_KNOTS ( 'NONE', 3,
 ( #71513, #40053, #38548, #69504, #30932, #39551 ),
 .UNSPECIFIED., .F., .F.,
 ( 4, 2, 4 ),
 ( 1.570755371633915156E-05, 0.001396183895866087753, 0.002776660238015836446 ),
 .UNSPECIFIED. ) ;
#52934 = ORIENTED_EDGE ( 'NONE', *, *, #59655, .T. ) ;
#52935 = DIRECTION ( 'NONE',  ( 0.06283980576413537855, 0.000000000000000000, 0.9980236263794188822 ) ) ;
#52936 = CARTESIAN_POINT ( 'NONE',  ( -49.64748826666535564, -25.06465475861797998, 7.411158395225631246 ) ) ;
#52937 = CARTESIAN_POINT ( 'NONE',  ( -89.62287095715002749, -23.73907113216990794, -1.053371485793227480 ) ) ;
#52938 = CARTESIAN_POINT ( 'NONE',  ( -4.647353109605855792, 20.10343637636090719, -1.500000000000002220 ) ) ;
#52939 = CARTESIAN_POINT ( 'NONE',  ( 0.6597851148675514255, -21.60297929554585394, 11.49999999999999645 ) ) ;
#52940 = VERTEX_POINT ( 'NONE', #50969 ) ;
#52941 = DIRECTION ( 'NONE',  ( -3.773278334444167608E-23, 1.000000000000000000, 0.000000000000000000 ) ) ;
#52942 = VECTOR ( 'NONE', #56069, 1000.000000000000114 ) ;
#52943 = LINE ( 'NONE', #60564, #35094 ) ;
#52944 = CARTESIAN_POINT ( 'NONE',  ( 22.01400519847025450, -3.885951517071169370, -1.500000000000002220 ) ) ;
#52945 = CARTESIAN_POINT ( 'NONE',  ( -93.52287095715006160, -24.64898659630368272, 1.056161002820827921 ) ) ;
#52946 = CARTESIAN_POINT ( 'NONE',  ( 0.7051282051282083962, -5.876774720514426953, 21.75000000000000000 ) ) ;
#52947 = EDGE_LOOP ( 'NONE', ( #73534, #86420, #35355, #25995 ) ) ;
#52948 = LINE ( 'NONE', #60068, #77637 ) ;
#52949 = CARTESIAN_POINT ( 'NONE',  ( -35.57399241795090461, -24.92592662359561118, 8.075495903017992916 ) ) ;
#52950 = AXIS2_PLACEMENT_3D ( 'NONE', #24129, #55099, #54106 ) ;
#52951 = CARTESIAN_POINT ( 'NONE',  ( -15.12424899162716230, 14.39509690008720177, 11.49999999999998934 ) ) ;
#52952 = ORIENTED_EDGE ( 'NONE', *, *, #35904, .F. ) ;
#52954 = ORIENTED_EDGE ( 'NONE', *, *, #86185, .F. ) ;
#52953 = CARTESIAN_POINT ( 'NONE',  ( -86.54787210963549171, -24.34968618360934300, 0.1864209137778916336 ) ) ;
#52955 = ORIENTED_EDGE ( 'NONE', *, *, #11216, .T. ) ;
#52956 = CARTESIAN_POINT ( 'NONE',  ( -109.5940830279356248, -23.73791477778912551, 11.05961554403169878 ) ) ;
#52957 = CARTESIAN_POINT ( 'NONE',  ( -11.89019930860364482, -17.45089671868802128, -1.500000000000002220 ) ) ;
#52958 = ORIENTED_EDGE ( 'NONE', *, *, #49029, .F. ) ;
#52959 = CARTESIAN_POINT ( 'NONE',  ( 29.73860345376319003, -1.682774720514426114, -1.272392034746785860 ) ) ;
#52960 = CARTESIAN_POINT ( 'NONE',  ( -99.61078991697702634, -25.26221256701134621, 6.818453477056792167 ) ) ;
#52961 = CARTESIAN_POINT ( 'NONE',  ( -17.45706314325883213, 13.02611496694466275, 11.49999999999998934 ) ) ;
#52962 = CARTESIAN_POINT ( 'NONE',  ( -19.80875734969026425, 5.965225279485572685, 31.02402280011862246 ) ) ;
#52963 = CARTESIAN_POINT ( 'NONE',  ( -30.57287095715006231, -23.47596703998576118, 11.44779287168131710 ) ) ;
#52964 = CARTESIAN_POINT ( 'NONE',  ( 0.2450472757604428842, -5.405843919193451086, -9.000000000000000000 ) ) ;
#52965 = CARTESIAN_POINT ( 'NONE',  ( 10.83000837110471082, 18.85367679709202804, -1.500000000000002220 ) ) ;
#52966 = CARTESIAN_POINT ( 'NONE',  ( -41.52287095715006870, -24.64898659630528144, 1.056161002820819261 ) ) ;
#52968 = VERTEX_POINT ( 'NONE', #72804 ) ;
#52967 = CARTESIAN_POINT ( 'NONE',  ( -16.35649155429130985, -15.18990082740072367, 11.49999999999999645 ) ) ;
#52969 = DIRECTION ( 'NONE',  ( 0.000000000000000000, -8.673617379884035472E-16, -1.000000000000000000 ) ) ;
#52970 = DIRECTION ( 'NONE',  ( -1.000000000000000000, -0.000000000000000000, -0.000000000000000000 ) ) ;
#52971 = CARTESIAN_POINT ( 'NONE',  ( -83.52287095715006160, -23.48786465467241769, 11.44779295918254469 ) ) ;
#52972 = ORIENTED_EDGE ( 'NONE', *, *, #26043, .F. ) ;
#52973 = AXIS2_PLACEMENT_3D ( 'NONE', #8698, #31521, #70091 ) ;
#52974 = ORIENTED_EDGE ( 'NONE', *, *, #63314, .T. ) ;
#52975 = ORIENTED_EDGE ( 'NONE', *, *, #68946, .F. ) ;
#52976 = CARTESIAN_POINT ( 'NONE',  ( 0.000000000000000000, 1.530000000000000027, 0.3849999999999992872 ) ) ;
#52977 = CARTESIAN_POINT ( 'NONE',  ( 18.56724428474754518, 10.22298014144217859, -1.500000000000002220 ) ) ;
#52978 = CARTESIAN_POINT ( 'NONE',  ( 8.971512145086528278, -9.528487854913501920, 6.500000000000001776 ) ) ;
#52979 = CARTESIAN_POINT ( 'NONE',  ( -79.70355613134685768, -25.27791930026442913, 7.365681066972862290 ) ) ;
#52980 = DIRECTION ( 'NONE',  ( 0.000000000000000000, 0.000000000000000000, -1.000000000000000000 ) ) ;
#52981 = AXIS2_PLACEMENT_3D ( 'NONE', #96588, #95594, #27087 ) ;
#52982 = CARTESIAN_POINT ( 'NONE',  ( 5.541369867593821219, -5.876774720514426065, 21.42815349816763160 ) ) ;
#52983 = CARTESIAN_POINT ( 'NONE',  ( -17.66094656686658482, 7.961706694365092041, 11.49999999999998934 ) ) ;
#52984 = EDGE_CURVE ( 'NONE', #54393, #68497, #83465, .T. ) ;
#52985 = CARTESIAN_POINT ( 'NONE',  ( -41.88978735995836189, -25.20650829394578096, 6.812666491500989352 ) ) ;
#52986 = VERTEX_POINT ( 'NONE', #10900 ) ;
#52987 = AXIS2_PLACEMENT_3D ( 'NONE', #21611, #69804, #45975 ) ;
#52988 = EDGE_CURVE ( 'NONE', #62489, #3631, #24443, .T. ) ;
#52989 = CARTESIAN_POINT ( 'NONE',  ( 12.19879910451502703, -15.15100395215988449, 11.49999999999999645 ) ) ;
#52990 = CARTESIAN_POINT ( 'NONE',  ( 1.351731822651893733, -3.882286141751412067, -8.999999999999998224 ) ) ;
#52991 = AXIS2_PLACEMENT_3D ( 'NONE', #64342, #3433, #80034 ) ;
#52992 = ORIENTED_EDGE ( 'NONE', *, *, #23077, .F. ) ;
#52993 = CARTESIAN_POINT ( 'NONE',  ( 3.248328688408994580, -5.876774720514406525, 18.75910638930973917 ) ) ;
#52994 = EDGE_CURVE ( 'NONE', #71801, #89948, #63305, .T. ) ;
#52995 = CARTESIAN_POINT ( 'NONE',  ( 3.769940963823357638, -5.876774720514403860, 18.16074422543206879 ) ) ;
#52996 = CARTESIAN_POINT ( 'NONE',  ( -44.55620429048338593, -23.47593901973091235, -1.443836447539011525 ) ) ;
#52997 = CIRCLE ( 'NONE', #47914, 1.150000000000003464 ) ;
#52998 = EDGE_CURVE ( 'NONE', #95938, #66032, #3311, .T. ) ;
#52999 = CARTESIAN_POINT ( 'NONE',  ( -63.95380932530888884, -23.47596703998600276, 11.44779298504227683 ) ) ;
#53000 = CARTESIAN_POINT ( 'NONE',  ( 10.60981200654714307, 16.52409317135366607, -1.500000000000002220 ) ) ;
#53001 = EDGE_CURVE ( 'NONE', #56546, #90808, #58444, .T. ) ;
#53002 = CARTESIAN_POINT ( 'NONE',  ( 23.50000000000000000, -0.9000000000000000222, -1.103411337323757957 ) ) ;
#53003 = ORIENTED_EDGE ( 'NONE', *, *, #29948, .F. ) ;
#53004 = CARTESIAN_POINT ( 'NONE',  ( 19.31049906410359895, -9.575588319827552652, 11.49999999999998934 ) ) ;
#53005 = CARTESIAN_POINT ( 'NONE',  ( 11.16000000000000014, -10.15233964170348457, 0.003711184059992174607 ) ) ;
#53006 = EDGE_CURVE ( 'NONE', #71460, #59162, #19000, .T. ) ;
#53007 = CARTESIAN_POINT ( 'NONE',  ( -115.6228709571500559, -23.47593901973091235, -1.443836447538997536 ) ) ;
#53008 = LINE ( 'NONE', #84932, #66958 ) ;
#53009 = CARTESIAN_POINT ( 'NONE',  ( -99.99551102217851906, -25.18439353279887527, 3.374614400146649373 ) ) ;
#53010 = CARTESIAN_POINT ( 'NONE',  ( -3.381418692465893105, -22.81955385325859709, -1.500000000000002220 ) ) ;
#53011 = APPROVAL_STATUS ( 'not_yet_approved' ) ;
#53012 = CARTESIAN_POINT ( 'NONE',  ( 10.45000000000000462, 1.999999999999998668, 18.24068255301867936 ) ) ;
#53013 = CARTESIAN_POINT ( 'NONE',  ( -62.62287095715004881, -24.65952944569304606, 1.056160979905693909 ) ) ;
#53014 = CARTESIAN_POINT ( 'NONE',  ( -11.96439459519798554, -16.23097265130270728, 11.49999999999999645 ) ) ;
#53015 = CARTESIAN_POINT ( 'NONE',  ( -109.0459178056501486, -25.10927576934983563, 3.663605367118155876 ) ) ;
#53016 = DIRECTION ( 'NONE',  ( -0.000000000000000000, 1.000000000000000000, -0.000000000000000000 ) ) ;
#53017 = CARTESIAN_POINT ( 'NONE',  ( -99.62287095715005592, -24.64965695001468404, 8.947790433994178727 ) ) ;
#53018 = DIRECTION ( 'NONE',  ( 0.000000000000000000, -1.000000000000000000, 0.000000000000000000 ) ) ;
#53019 = CARTESIAN_POINT ( 'NONE',  ( -110.5404475696186779, -25.18425585998923921, 3.309296991606290650 ) ) ;
#53020 = CARTESIAN_POINT ( 'NONE',  ( -1.769646468872753120, 19.80360307839763934, 11.49999999999998934 ) ) ;
#53021 = CARTESIAN_POINT ( 'NONE',  ( -41.55620429048340014, -23.48783264082478084, -1.443836473390071484 ) ) ;
#53022 = CARTESIAN_POINT ( 'NONE',  ( 6.953341435731974940, 18.52374150113109152, -1.500000000000002220 ) ) ;
#53023 = AXIS2_PLACEMENT_3D ( 'NONE', #11633, #34982, #80158 ) ;
#53024 = LINE ( 'NONE', #52517, #45939 ) ;
#53025 = B_SPLINE_CURVE_WITH_KNOTS ( 'NONE', 3,
 ( #1628, #32559, #23942, #62021 ),
 .UNSPECIFIED., .F., .F.,
 ( 4, 4 ),
 ( 0.000000000000000000, 0.0001002978970083175645 ),
 .UNSPECIFIED. ) ;
#53026 = CARTESIAN_POINT ( 'NONE',  ( -1.044792363895550302, -6.376774720514417183, 20.41272575174754422 ) ) ;
#53027 = CARTESIAN_POINT ( 'NONE',  ( -1.345681049247692940, -6.376774720514410077, 19.69174559449348294 ) ) ;
#53028 = CARTESIAN_POINT ( 'NONE',  ( -18.22997975830956108, -9.740667652671243459, 11.49999999999999645 ) ) ;
#53029 = AXIS2_PLACEMENT_3D ( 'NONE', #5307, #68214, #44886 ) ;
#53030 = LINE ( 'NONE', #69236, #40240 ) ;
#53031 = CARTESIAN_POINT ( 'NONE',  ( -0.02075734969026423599, 6.376774720514426953, -0.08597719988137648983 ) ) ;
#53032 = CARTESIAN_POINT ( 'NONE',  ( -24.90875734969025501, 3.316774720514426456, 26.43402280011862615 ) ) ;
#53033 = CARTESIAN_POINT ( 'NONE',  ( -16.51154719052397724, 15.62863258182435189, 11.49999999999999645 ) ) ;
#53034 = ORIENTED_EDGE ( 'NONE', *, *, #61512, .F. ) ;
#53035 = DIRECTION ( 'NONE',  ( 0.9890158633619159367, 0.1478094111296165969, 0.000000000000000000 ) ) ;
#53036 = LINE ( 'NONE', #62643, #16013 ) ;
#53037 = CARTESIAN_POINT ( 'NONE',  ( 16.36621611169882229, 11.82581248522330064, -1.500000000000002220 ) ) ;
#53038 = CARTESIAN_POINT ( 'NONE',  ( -63.64765489167466228, -23.73766607897669090, -1.055555164236456900 ) ) ;
#53039 = LINE ( 'NONE', #30175, #57721 ) ;
#53040 = ORIENTED_EDGE ( 'NONE', *, *, #16882, .T. ) ;
#53041 = CIRCLE ( 'NONE', #82149, 1.499999999999999556 ) ;
#53042 = ORIENTED_EDGE ( 'NONE', *, *, #22042, .T. ) ;
#53043 = CARTESIAN_POINT ( 'NONE',  ( -0.2112149364088803105, -6.376774720514410077, 19.49357334786886398 ) ) ;
#53044 = CARTESIAN_POINT ( 'NONE',  ( 19.82229641098322404, 11.46754112681587046, 11.49999999999998934 ) ) ;
#53045 = CARTESIAN_POINT ( 'NONE',  ( -50.58832339509404363, -25.27420565479429015, 3.304980239963009492 ) ) ;
#53046 = CARTESIAN_POINT ( 'NONE',  ( 21.43499300031224664, 3.042053824063517542, -1.500000000000002220 ) ) ;
#53047 = CARTESIAN_POINT ( 'NONE',  ( -118.6228709571500559, -29.50250243563736774, 8.947779886222134493 ) ) ;
#53048 = CARTESIAN_POINT ( 'NONE',  ( -10.24059822343757808, -6.376774720514426953, 22.08128695274315945 ) ) ;
#53049 = CARTESIAN_POINT ( 'NONE',  ( 19.90007246472742608, 6.374896562862660154, 11.49999999999999645 ) ) ;
#53050 = VERTEX_POINT ( 'NONE', #97621 ) ;
#53051 = CARTESIAN_POINT ( 'NONE',  ( -29.24636659181000198, -25.21267509515801564, 4.940287023516041209 ) ) ;
#53052 = CARTESIAN_POINT ( 'NONE',  ( 12.93620265873104991, 17.78788284566447331, 11.49999999999998934 ) ) ;
#53053 = ADVANCED_FACE ( 'NONE', ( #65709 ), #96622, .F. ) ;
#53054 = CIRCLE ( 'NONE', #43350, 6.594667762285749468 ) ;
#53055 = CARTESIAN_POINT ( 'NONE',  ( -105.5132737718367650, -24.40133493613049964, 9.663955038902797057 ) ) ;
#53056 = CARTESIAN_POINT ( 'NONE',  ( -41.82812249501711932, -25.29087254191939849, 3.843615201987044205 ) ) ;
#53057 = ORIENTED_EDGE ( 'NONE', *, *, #39252, .T. ) ;
#53058 = DIRECTION ( 'NONE',  ( -1.000000000000000000, -0.000000000000000000, -0.000000000000000000 ) ) ;
#53059 = EDGE_CURVE ( 'NONE', #66032, #27769, #98303, .T. ) ;
#53060 = CARTESIAN_POINT ( 'NONE',  ( -90.54437712527642645, -24.73531770709095312, 8.716586749053512051 ) ) ;
#53061 = ORIENTED_EDGE ( 'NONE', *, *, #86469, .F. ) ;
#53062 = CARTESIAN_POINT ( 'NONE',  ( -28.98875734969026041, 6.376774720514426953, 0.7300228001186309656 ) ) ;
#53063 = ORIENTED_EDGE ( 'NONE', *, *, #26995, .F. ) ;
#53064 = CIRCLE ( 'NONE', #20661, 4.080000000000000071 ) ;
#53065 = ORIENTED_EDGE ( 'NONE', *, *, #50462, .F. ) ;
#53066 = CARTESIAN_POINT ( 'NONE',  ( -32.52287095715006160, -24.64898659630528854, 1.056161002820817485 ) ) ;
#53067 = CARTESIAN_POINT ( 'NONE',  ( -101.6521089408578007, -25.10935970639156523, 3.606142542491853398 ) ) ;
#53068 = CARTESIAN_POINT ( 'NONE',  ( -57.49755803318443981, -24.34968618360933590, 0.1864209137778796155 ) ) ;
#53069 = B_SPLINE_CURVE_WITH_KNOTS ( 'NONE', 3,
 ( #41776, #49890, #34155, #26539, #57503, #80823 ),
 .UNSPECIFIED., .F., .F.,
 ( 4, 2, 4 ),
 ( 0.000000000000000000, 0.001380764517853252287, 0.002761529035706504574 ),
 .UNSPECIFIED. ) ;
#53070 = CARTESIAN_POINT ( 'NONE',  ( 20.11976772532220181, -3.360927329567881205, -1.500000000000002220 ) ) ;
#53071 = ORIENTED_EDGE ( 'NONE', *, *, #66764, .F. ) ;
#53072 = CARTESIAN_POINT ( 'NONE',  ( -3.004714864173751998, -5.876774720514410966, 19.63296556618507083 ) ) ;
#53073 = CARTESIAN_POINT ( 'NONE',  ( -61.22287095715005734, -23.47593901973090169, -1.443836447538997758 ) ) ;
#53074 = CARTESIAN_POINT ( 'NONE',  ( -98.58953762381671027, -24.65952944569304606, 1.056160979905695907 ) ) ;
#53075 = CARTESIAN_POINT ( 'NONE',  ( -91.52287095715006160, -23.94994826722564341, -0.6494450866342701412 ) ) ;
#53076 = ORIENTED_EDGE ( 'NONE', *, *, #47136, .T. ) ;
#53077 = PLANE ( 'NONE',  #90542 ) ;
#53078 = CARTESIAN_POINT ( 'NONE',  ( -85.62287095715007013, -25.00158670708909270, 2.256160236439165967 ) ) ;
#53079 = B_SPLINE_CURVE_WITH_KNOTS ( 'NONE', 3,
 ( #28282, #29780, #74940, #68350, #52128, #36396, #91669, #82565 ),
 .UNSPECIFIED., .F., .F.,
 ( 4, 2, 2, 4 ),
 ( 6.384118678607358824E-06, 0.002007151183507253651, 0.003007534715921578606, 0.004007918248335903995 ),
 .UNSPECIFIED. ) ;
#53080 = CARTESIAN_POINT ( 'NONE',  ( 17.70469293622815243, 10.90570606759641592, 11.49999999999998934 ) ) ;
#53081 = ORIENTED_EDGE ( 'NONE', *, *, #1248, .T. ) ;
#53083 = EDGE_CURVE ( 'NONE', #8583, #55708, #6304, .T. ) ;
#53082 = CC_DESIGN_DATE_AND_TIME_ASSIGNMENT ( #70867, #31287, ( #66951 ) ) ;
#53085 = VERTEX_POINT ( 'NONE', #10392 ) ;
#53084 = CARTESIAN_POINT ( 'NONE',  ( 4.613443512364428400, -6.376774720514411854, 19.38647409819875733 ) ) ;
#53086 = CARTESIAN_POINT ( 'NONE',  ( -44.52287095715006160, -23.47596703998600631, 11.44779298504229281 ) ) ;
#53087 = ORIENTED_EDGE ( 'NONE', *, *, #978, .T. ) ;
#53088 = EDGE_LOOP ( 'NONE', ( #99735, #41230, #59680, #16720 ) ) ;
#53089 = CARTESIAN_POINT ( 'NONE',  ( 31.62300803125484094, -5.234178280976530928, -3.660617518925037395 ) ) ;
#53090 = CARTESIAN_POINT ( 'NONE',  ( -92.62287095715005592, -23.48786465467241413, 11.44779295918254469 ) ) ;
#53091 =( REPRESENTATION_RELATIONSHIP ('NONE','NONE', #96270, #9419 ) REPRESENTATION_RELATIONSHIP_WITH_TRANSFORMATION ( #32790 )SHAPE_REPRESENTATION_RELATIONSHIP( ) );
#53092 = PLANE ( 'NONE',  #2726 ) ;
#53093 = CARTESIAN_POINT ( 'NONE',  ( -40.62287095715009144, -24.92604778743017491, 8.074972756849357225 ) ) ;
#53094 = CARTESIAN_POINT ( 'NONE',  ( -110.5228709571500758, -23.47593901973090524, -1.443836447538996204 ) ) ;
#53095 = CARTESIAN_POINT ( 'NONE',  ( -113.6228709571500559, -29.50248528299804818, 1.056150453629043584 ) ) ;
#53097 = ORIENTED_EDGE ( 'NONE', *, *, #66447, .T. ) ;
#53096 = CARTESIAN_POINT ( 'NONE',  ( -14.81638660137672225, 16.44347145309322045, 11.49999999999999645 ) ) ;
#53098 = CARTESIAN_POINT ( 'NONE',  ( 5.184553252003285984, -5.965225279485572685, -28.06387035751381731 ) ) ;
#53099 = CARTESIAN_POINT ( 'NONE',  ( 22.61563695565308407, -1.323143620866313208, 11.49999999999998934 ) ) ;
#53100 = AXIS2_PLACEMENT_3D ( 'NONE', #94263, #76525, #93260 ) ;
#53102 = VERTEX_POINT ( 'NONE', #20491 ) ;
#53101 = CARTESIAN_POINT ( 'NONE',  ( -27.83193219186368950, -24.81234328755879659, 7.598342972711060739 ) ) ;
#53103 = B_SPLINE_CURVE_WITH_KNOTS ( 'NONE', 3,
 ( #11684, #4595, #86437, #34040 ),
 .UNSPECIFIED., .F., .F.,
 ( 4, 4 ),
 ( 0.6692531030269918135, 0.6702538500677572841 ),
 .UNSPECIFIED. ) ;
#53104 = ORIENTED_EDGE ( 'NONE', *, *, #80833, .T. ) ;
#53105 = VECTOR ( 'NONE', #24410, 1000.000000000000114 ) ;
#53106 = CARTESIAN_POINT ( 'NONE',  ( -99.52287095715006160, -24.65952944569304961, 1.056160979905702346 ) ) ;
#53107 = CARTESIAN_POINT ( 'NONE',  ( 4.949566031639514918, 19.51814346981619863, 11.49999999999998934 ) ) ;
#53108 = CARTESIAN_POINT ( 'NONE',  ( 32.66876533700883556, 5.965225279485572685, -12.58926540598386445 ) ) ;
#53109 = EDGE_LOOP ( 'NONE', ( #71429, #16592, #91376, #24370 ) ) ;
#53110 = CARTESIAN_POINT ( 'NONE',  ( -10.40290173325841216, 5.356774720514425603, 27.45402280011861862 ) ) ;
#53111 = CARTESIAN_POINT ( 'NONE',  ( 19.81157572017019319, -10.35993776028809421, -1.500000000000002220 ) ) ;
#53112 = ORIENTED_EDGE ( 'NONE', *, *, #10282, .T. ) ;
#53113 = ORIENTED_EDGE ( 'NONE', *, *, #93615, .F. ) ;
#53114 = DIRECTION ( 'NONE',  ( -1.000000000000000000, -3.773278334444167608E-23, -8.201307833595939069E-29 ) ) ;
#53115 = CARTESIAN_POINT ( 'NONE',  ( -124.4728709571500360, -25.30558663486635851, 5.000950659935021747 ) ) ;
#53116 = ADVANCED_FACE ( 'NONE', ( #41350 ), #72304, .T. ) ;
#53117 = CARTESIAN_POINT ( 'NONE',  ( -51.62287095715005592, -29.50247984919015209, -1.443849546365058689 ) ) ;
#53118 = CARTESIAN_POINT ( 'NONE',  ( -101.5228709571500900, -24.66019654487200441, 8.947790411086119278 ) ) ;
#53119 = CIRCLE ( 'NONE', #17396, 251.4258649670780699 ) ;
#53120 = FACE_OUTER_BOUND ( 'NONE', #60931, .T. ) ;
#53121 = CARTESIAN_POINT ( 'NONE',  ( 3.994393897313025743, -19.14333888664780048, 11.49999999999998934 ) ) ;
#53122 = EDGE_CURVE ( 'NONE', #88443, #80901, #65641, .T. ) ;
#53123 = FACE_OUTER_BOUND ( 'NONE', #59729, .T. ) ;
#53124 = CARTESIAN_POINT ( 'NONE',  ( -19.15072323977689095, -9.709862252083167888, -1.500000000000002220 ) ) ;
#53125 = CARTESIAN_POINT ( 'NONE',  ( -2.532641601674031850, -6.376774720514410077, 19.55266968305501507 ) ) ;
#53126 = EDGE_CURVE ( 'NONE', #63165, #38340, #42634, .T. ) ;
#53127 = DIRECTION ( 'NONE',  ( -3.773278334444167608E-23, 1.000000000000000000, 0.000000000000000000 ) ) ;
#53128 = FACE_OUTER_BOUND ( 'NONE', #37311, .T. ) ;
#53129 = CARTESIAN_POINT ( 'NONE',  ( -4.124250913864588419, 22.51598698906299845, -1.500000000000002220 ) ) ;
#53130 = AXIS2_PLACEMENT_3D ( 'NONE', #64699, #89006, #96119 ) ;
#53131 = CALENDAR_DATE ( 2026, 9, 10 ) ;
#53132 = CARTESIAN_POINT ( 'NONE',  ( -96.59124853101694441, -24.15620529776628445, 10.23563542870660115 ) ) ;
#53133 = CARTESIAN_POINT ( 'NONE',  ( -108.5228709571501327, -23.73907113217652309, -1.053371485781582573 ) ) ;
#53134 = CARTESIAN_POINT ( 'NONE',  ( 1.593314845114734535, -19.89410510517485164, 11.49999999999999645 ) ) ;
#53135 = PLANE ( 'NONE',  #20889 ) ;
#53136 = CIRCLE ( 'NONE', #66119, 1.000000000000000000 ) ;
#53137 = CARTESIAN_POINT ( 'NONE',  ( -74.64369162555894377, -23.73791477778911840, 11.05961554403170588 ) ) ;
#53138 = CARTESIAN_POINT ( 'NONE',  ( -127.5228709571500332, -24.66019654487200441, 8.947790411086105067 ) ) ;
#53139 = ORIENTED_EDGE ( 'NONE', *, *, #76326, .F. ) ;
#53140 = EDGE_CURVE ( 'NONE', #60724, #100069, #61074, .T. ) ;
#53141 = CARTESIAN_POINT ( 'NONE',  ( -57.22287095715011418, -23.47593901973090524, -1.443836447538998202 ) ) ;
#53142 = CARTESIAN_POINT ( 'NONE',  ( 14.76093561896378326, -3.316774720514426456, -26.55548769130088260 ) ) ;
#53143 = CARTESIAN_POINT ( 'NONE',  ( -21.04499429308205549, 5.405531755741471045, 11.49999999999998934 ) ) ;
#53144 = DIRECTION ( 'NONE',  ( -3.773278334453079030E-23, 0.9999999999976377785, 2.173523156925979128E-06 ) ) ;
#53145 = CARTESIAN_POINT ( 'NONE',  ( 8.161054176536994831, -17.82452852192863091, -1.500000000000002220 ) ) ;
#53146 = DIRECTION ( 'NONE',  ( 0.000000000000000000, 0.000000000000000000, -1.000000000000000000 ) ) ;
#53147 = ORIENTED_EDGE ( 'NONE', *, *, #73256, .F. ) ;
#53148 = APPROVAL_DATE_TIME ( #5952, #64905 ) ;
#53149 = DIRECTION ( 'NONE',  ( -0.000000000000000000, 1.000000000000000000, -0.000000000000000000 ) ) ;
#53150 = CARTESIAN_POINT ( 'NONE',  ( 3.323502641304225236, -5.876774720514426065, 21.72931788002195219 ) ) ;
#53151 = CARTESIAN_POINT ( 'NONE',  ( -17.91610926057384034, -10.00117247862695358, 11.49999999999999645 ) ) ;
#53152 = CARTESIAN_POINT ( 'NONE',  ( -79.52287095715006160, -23.47596703998600631, 11.44779298504228571 ) ) ;
#53153 = CARTESIAN_POINT ( 'NONE',  ( -42.58953762381671737, -24.66019654487199375, 8.947790411086133489 ) ) ;
#53154 = VERTEX_POINT ( 'NONE', #69169 ) ;
#53155 =( NAMED_UNIT ( * ) PLANE_ANGLE_UNIT ( ) SI_UNIT ( $, .RADIAN. ) );
#53156 = CARTESIAN_POINT ( 'NONE',  ( -51.52287095715008292, -23.47593901973090169, -1.443836447538997092 ) ) ;
#53157 = CARTESIAN_POINT ( 'NONE',  ( 22.02124265030973760, -7.835183881457444599, 14.80402280011862359 ) ) ;
#53158 = PLANE ( 'NONE',  #90550 ) ;
#53159 = CARTESIAN_POINT ( 'NONE',  ( -104.6228709571500559, -23.47596703998600631, 11.44779298504227860 ) ) ;
#53160 = CARTESIAN_POINT ( 'NONE',  ( 22.81105451610979173, 8.475225279485572472, -17.31691820600746823 ) ) ;
#53161 = AXIS2_PLACEMENT_3D ( 'NONE', #82538, #50601, #81555 ) ;
#53162 = EDGE_CURVE ( 'NONE', #65082, #11869, #6764, .T. ) ;
#53163 = CARTESIAN_POINT ( 'NONE',  ( 7.103900956763240515, -21.94381868531750968, 11.49999999999999645 ) ) ;
#53164 = CARTESIAN_POINT ( 'NONE',  ( 4.317061085376620255, -22.40314112565372540, 11.49999999999998934 ) ) ;
#53165 = DIRECTION ( 'NONE',  ( 0.000000000000000000, 0.000000000000000000, 1.000000000000000000 ) ) ;
#53166 = B_SPLINE_SURFACE_WITH_KNOTS ( 'NONE', 3, 1, ( 
 ( #74450, #10554 ),
 ( #43513, #28273 ),
 ( #88189, #3953 ),
 ( #26281, #97780 ),
 ( #18659, #49634 ),
 ( #72467, #4454 ),
 ( #11547, #42523 ),
 ( #35406, #4942 ),
 ( #73460, #19654 ),
 ( #66858, #59231 ),
 ( #80564, #2961 ),
 ( #11059, #43015 ),
 ( #66363, #33894 ),
 ( #96295, #58241 ),
 ( #50127, #57259 ) ),
 .UNSPECIFIED., .F., .F., .F.,
 ( 4, 1, 1, 1, 1, 1, 1, 1, 1, 1, 1, 1, 4 ),
 ( 2, 2 ),
 ( 0.000000000000000000, 0.1041667992898099859, 0.1978560952899031111, 0.2832345117281489522, 0.3600126653135322652, 0.4338442080180774374, 0.5095057223304355620, 0.5870428909783852456, 0.6687538545127398315, 0.7511636688534701900, 0.8334676797015420080, 0.9158479811556836658, 1.000000000000000000 ),
 ( 0.000000000000000000, 1.000000000000000000 ),
 .UNSPECIFIED. ) ;
#53167 = CARTESIAN_POINT ( 'NONE',  ( -5.799455386767018439, -6.376774720514413630, 19.66076420632890276 ) ) ;
#53168 = DIRECTION ( 'NONE',  ( -0.000000000000000000, 1.000000000000000000, -0.000000000000000000 ) ) ;
#53169 = FACE_OUTER_BOUND ( 'NONE', #8367, .T. ) ;
#53170 = CARTESIAN_POINT ( 'NONE',  ( -99.60147378138974261, -25.31582203441881163, 4.950471085733717302 ) ) ;
#53171 = CARTESIAN_POINT ( 'NONE',  ( -3.478157889954244464, -21.63767827151469447, -1.500000000000002220 ) ) ;
#53172 = EDGE_CURVE ( 'NONE', #60950, #86083, #67695, .T. ) ;
#53173 = DIRECTION ( 'NONE',  ( -1.000000000000000000, -0.000000000000000000, -0.000000000000000000 ) ) ;
#53174 = CARTESIAN_POINT ( 'NONE',  ( -17.64648606763744354, 5.965225279485594001, -23.04404205923972526 ) ) ;
#53175 = LINE ( 'NONE', #85105, #47039 ) ;
#53176 = CARTESIAN_POINT ( 'NONE',  ( -78.55426290676015810, -23.96119346886880308, -0.6495511937832113558 ) ) ;
#53177 = DIRECTION ( 'NONE',  ( 0.000000000000000000, 1.000000000000000000, 0.000000000000000000 ) ) ;
#53178 = DIRECTION ( 'NONE',  ( -0.000000000000000000, 1.000000000000000000, -0.000000000000000000 ) ) ;
#53179 = ORIENTED_EDGE ( 'NONE', *, *, #96536, .F. ) ;
#53180 = CARTESIAN_POINT ( 'NONE',  ( -1.999887071766271784, 20.33596237858139233, 11.49999999999998934 ) ) ;
#53181 = ORIENTED_EDGE ( 'NONE', *, *, #56232, .T. ) ;
#53182 = VERTEX_POINT ( 'NONE', #5276 ) ;
#53183 = ORIENTED_EDGE ( 'NONE', *, *, #62408, .F. ) ;
#53184 = ORIENTED_EDGE ( 'NONE', *, *, #68213, .F. ) ;
#53185 = CARTESIAN_POINT ( 'NONE',  ( -18.27982475084466785, -14.08179083545084964, -1.500000000000002220 ) ) ;
#53186 = CARTESIAN_POINT ( 'NONE',  ( -95.52287095715006160, -25.00158670708909980, 2.256160236439166411 ) ) ;
#53187 = CARTESIAN_POINT ( 'NONE',  ( -10.81679630089563915, -17.07601267366916886, -1.500000000000002220 ) ) ;
#53188 = VERTEX_POINT ( 'NONE', #59580 ) ;
#53189 = CARTESIAN_POINT ( 'NONE',  ( -122.5228709571500900, -23.94994826722565406, -0.6494450866342689199 ) ) ;
#53190 = VECTOR ( 'NONE', #78053, 1000.000000000000114 ) ;
#53191 = DIRECTION ( 'NONE',  ( -3.773278334453079618E-23, 0.9999999999976377785, 2.173523156925979975E-06 ) ) ;
#53192 = DIRECTION ( 'NONE',  ( -3.773278334444167608E-23, 1.000000000000000000, 0.000000000000000000 ) ) ;
#53193 = CARTESIAN_POINT ( 'NONE',  ( -70.50645411744089586, -24.15503026093916006, -0.2815557561904372674 ) ) ;
#53195 = VERTEX_POINT ( 'NONE', #67196 ) ;
#53194 = CARTESIAN_POINT ( 'NONE',  ( 4.431377227695222132, -20.94745169971119481, 11.49999999999999645 ) ) ;
#53196 = CARTESIAN_POINT ( 'NONE',  ( -100.6228709571500559, -23.47593901973091235, -1.443836447539001089 ) ) ;
#53197 = DIRECTION ( 'NONE',  ( 0.000000000000000000, -1.000000000000000000, 0.000000000000000000 ) ) ;
#53198 = ORIENTED_EDGE ( 'NONE', *, *, #8486, .T. ) ;
#53199 = CARTESIAN_POINT ( 'NONE',  ( -20.55201672899488585, 2.666056886502145673, -1.500000000000002220 ) ) ;
#53200 = CIRCLE ( 'NONE', #9430, 129.7684398600581517 ) ;
#53201 = CC_DESIGN_PERSON_AND_ORGANIZATION_ASSIGNMENT ( #52005, #11937, ( #16510 ) ) ;
#53203 = ORIENTED_EDGE ( 'NONE', *, *, #32838, .F. ) ;
#53202 = CARTESIAN_POINT ( 'NONE',  ( -11.64875734969026233, 5.965225279485572685, 30.51402280011862089 ) ) ;
#53204 = CARTESIAN_POINT ( 'NONE',  ( -29.62287095715004881, -24.58457514626677209, 8.947790440257529454 ) ) ;
#53205 = ORIENTED_EDGE ( 'NONE', *, *, #32528, .T. ) ;
#53206 = CARTESIAN_POINT ( 'NONE',  ( 4.886128916861816052, -5.876774720514410077, 19.14085035285361514 ) ) ;
#53207 = AXIS2_PLACEMENT_3D ( 'NONE', #40905, #57154, #88093 ) ;
#53208 = LINE ( 'NONE', #913, #78889 ) ;
#53209 = CARTESIAN_POINT ( 'NONE',  ( -21.97012646571106842, -0.5360883523215664859, 11.49999999999999645 ) ) ;
#53210 = CARTESIAN_POINT ( 'NONE',  ( -91.62287095715004170, -24.65952944569304606, 1.056160979905700792 ) ) ;
#53211 = CARTESIAN_POINT ( 'NONE',  ( 14.20245820080859289, -17.52920931871068433, 11.49999999999998934 ) ) ;
#53212 = EDGE_CURVE ( 'NONE', #89486, #17142, #23552, .T. ) ;
#53213 = CARTESIAN_POINT ( 'NONE',  ( -15.18370147500227496, -14.46048895944246127, -1.500000000000002220 ) ) ;
#53214 = CARTESIAN_POINT ( 'NONE',  ( -109.3584176993576591, -25.28950181196791647, 4.206202504803813191 ) ) ;
#53215 = CARTESIAN_POINT ( 'NONE',  ( -30.64535912258471839, -23.53197991584894666, -1.479945482512690313 ) ) ;
#53216 = ORIENTED_EDGE ( 'NONE', *, *, #8558, .F. ) ;
#53217 = AXIS2_PLACEMENT_3D ( 'NONE', #21054, #52025, #9833 ) ;
#53218 = B_SPLINE_CURVE_WITH_KNOTS ( 'NONE', 3,
 ( #65291, #97203, #3380, #58647, #51041, #27202 ),
 .UNSPECIFIED., .F., .F.,
 ( 4, 2, 4 ),
 ( 6.391158118959991367E-06, 0.001387004593080780942, 0.002767618028042601996 ),
 .UNSPECIFIED. ) ;
#53219 = EDGE_LOOP ( 'NONE', ( #40976, #54222, #81918, #32077 ) ) ;
#53220 = VERTEX_POINT ( 'NONE', #14372 ) ;
#53221 = CARTESIAN_POINT ( 'NONE',  ( -44.52287095715007581, -24.66019654487199730, 8.947790411086117501 ) ) ;
#53222 = CARTESIAN_POINT ( 'NONE',  ( 20.98156868870745484, 4.911575462371418510, -1.500000000000002220 ) ) ;
#53223 = CARTESIAN_POINT ( 'NONE',  ( -50.37830952628071657, -25.31401921878212136, 5.197788989978542773 ) ) ;
#53224 = EDGE_LOOP ( 'NONE', ( #52759, #84401, #7398, #67325 ) ) ;
#53225 = CARTESIAN_POINT ( 'NONE',  ( -15.55823947972799282, -14.28038451723262270, -1.500000000000002220 ) ) ;
#53226 = CARTESIAN_POINT ( 'NONE',  ( -67.52287095715003318, -23.47593901973090169, -1.443836447538996870 ) ) ;
#53227 = CARTESIAN_POINT ( 'NONE',  ( -81.61611000704996854, -25.24685308744633261, 6.293942982122114671 ) ) ;
#53228 = DIRECTION ( 'NONE',  ( 0.000000000000000000, 1.000000000000000000, -8.673617379884035472E-16 ) ) ;
#53229 = CARTESIAN_POINT ( 'NONE',  ( 14.61581676225068449, -6.475225279485576912, -27.35847991880143226 ) ) ;
#53230 = CARTESIAN_POINT ( 'NONE',  ( -42.52287095715005449, -23.47593901973090169, -1.443836447538997092 ) ) ;
#53231 = CARTESIAN_POINT ( 'NONE',  ( -0.8134642310582372859, 22.17477653155656725, -1.500000000000002220 ) ) ;
#53232 = CARTESIAN_POINT ( 'NONE',  ( -34.62287095715007013, -23.47596703998600276, 11.44779298504227505 ) ) ;
#53233 = EDGE_CURVE ( 'NONE', #36594, #12687, #60771, .T. ) ;
#53234 = ORIENTED_EDGE ( 'NONE', *, *, #925, .F. ) ;
#53235 = DIRECTION ( 'NONE',  ( 3.469446951953615372E-15, -1.000000000000000000, 0.000000000000000000 ) ) ;
#53236 = DIRECTION ( 'NONE',  ( 0.000000000000000000, 0.000000000000000000, 1.000000000000000000 ) ) ;
#53237 = DIRECTION ( 'NONE',  ( -0.000000000000000000, -1.000000000000000000, -0.000000000000000000 ) ) ;
#53238 = DIRECTION ( 'NONE',  ( 0.000000000000000000, 1.000000000000000000, 0.000000000000000000 ) ) ;
#53239 = CARTESIAN_POINT ( 'NONE',  ( -18.83898130102433299, -4.906684326670742280, 11.49999999999998934 ) ) ;
#53240 = EDGE_CURVE ( 'NONE', #43365, #78758, #68921, .T. ) ;
#53241 = CARTESIAN_POINT ( 'NONE',  ( -21.18999663186871274, 2.814949255606389311, 11.49999999999998934 ) ) ;
#53242 = CARTESIAN_POINT ( 'NONE',  ( -62.60383260654986515, -23.73766607897669445, -1.055555164236454901 ) ) ;
#53243 = DIRECTION ( 'NONE',  ( 0.000000000000000000, -0.9999999999976377785, -2.173523156925979975E-06 ) ) ;
#53244 = ADVANCED_FACE ( 'NONE', ( #21978 ), #19036, .T. ) ;
#53245 = CARTESIAN_POINT ( 'NONE',  ( -79.62287095715009855, -23.73907113216991860, -1.053371485793228812 ) ) ;
#53246 = CARTESIAN_POINT ( 'NONE',  ( -33.62287095715005592, -24.64965695001467694, 8.947790433994189385 ) ) ;
#53247 = CARTESIAN_POINT ( 'NONE',  ( -2.225104987405961854, -22.55768739424384606, -1.500000000000002220 ) ) ;
#53248 = B_SPLINE_SURFACE_WITH_KNOTS ( 'NONE', 3, 3, ( 
 ( #76007, #84127, #37465, #16113 ),
 ( #85126, #29844, #39462, #69411 ),
 ( #23724, #62309, #93234, #61810 ),
 ( #15612, #84627, #77001, #99832 ),
 ( #91736, #8511, #77503, #898 ),
 ( #8005, #76501, #31853, #38953 ),
 ( #61313, #22710, #69908, #24230 ) ),
 .UNSPECIFIED., .F., .F., .F.,
 ( 4, 3, 4 ),
 ( 4, 4 ),
 ( 0.7945040050992244751, 0.8970133687736505657, 0.9995227324480766562 ),
 ( 0.6896692517579798842, 0.6910003734054406266 ),
 .UNSPECIFIED. ) ;
#53249 = EDGE_LOOP ( 'NONE', ( #82762, #35768, #13914, #31843, #82433, #90994, #89660 ) ) ;
#53250 = DIRECTION ( 'NONE',  ( 0.000000000000000000, 0.000000000000000000, 1.000000000000000000 ) ) ;
#53251 = DIRECTION ( 'NONE',  ( 3.773278334444166432E-23, -1.000000000000000000, 0.000000000000000000 ) ) ;
#53252 = CARTESIAN_POINT ( 'NONE',  ( -19.21288746854601115, 4.878285775029977955, 11.49999999999999645 ) ) ;
#53253 = FACE_OUTER_BOUND ( 'NONE', #87897, .T. ) ;
#53254 = ORIENTED_EDGE ( 'NONE', *, *, #69062, .F. ) ;
#53255 = EDGE_CURVE ( 'NONE', #33670, #52199, #31100, .T. ) ;
#53256 = CARTESIAN_POINT ( 'NONE',  ( -5.895658455092926076, -5.876774720514418071, 20.50445910983877340 ) ) ;
#53257 = CARTESIAN_POINT ( 'NONE',  ( -91.15361000704997707, -25.26877915520014639, 5.947789088310639904 ) ) ;
#53258 = CARTESIAN_POINT ( 'NONE',  ( 2.186256072416925544, -21.55203199515037582, -1.500000000000002220 ) ) ;
#53259 = CARTESIAN_POINT ( 'NONE',  ( -49.19632817692706084, -25.27518035636533966, 3.560433938396965647 ) ) ;
#53260 = AXIS2_PLACEMENT_3D ( 'NONE', #61497, #62493, #29525 ) ;
#53261 = CARTESIAN_POINT ( 'NONE',  ( 7.440116899146960172, 17.95454168335740874, -1.500000000000002220 ) ) ;
#53262 = CARTESIAN_POINT ( 'NONE',  ( -129.6228709571500133, -24.35013146730204525, 9.818937971375103047 ) ) ;
#53263 = CARTESIAN_POINT ( 'NONE',  ( -40.55620429048337883, -24.99156044556202261, 7.747789690856173195 ) ) ;
#53264 = CARTESIAN_POINT ( 'NONE',  ( -11.05534852661189937, -16.44151763790470966, 11.49999999999998934 ) ) ;
#53265 = VERTEX_POINT ( 'NONE', #8775 ) ;
#53266 = CARTESIAN_POINT ( 'NONE',  ( 5.353267490507026771, -19.58905154090721368, 11.49999999999999645 ) ) ;
#53267 = CARTESIAN_POINT ( 'NONE',  ( -80.58318732538134554, -24.83618233451450408, 1.606449574219532384 ) ) ;
#53268 = CARTESIAN_POINT ( 'NONE',  ( 33.29716795723528833, -4.396921096972350007, -11.57973373708315989 ) ) ;
#53269 = ORIENTED_EDGE ( 'NONE', *, *, #36573, .T. ) ;
#53270 = CARTESIAN_POINT ( 'NONE',  ( -102.5148950863152493, -24.15620529776628800, 10.23563542870660292 ) ) ;
#53271 = CARTESIAN_POINT ( 'NONE',  ( -78.62287095715005592, -29.50250243563736774, 8.947779886222141599 ) ) ;
#53272 = FACE_OUTER_BOUND ( 'NONE', #90505, .T. ) ;
#53273 = VECTOR ( 'NONE', #38288, 1000.000000000000000 ) ;
#53274 = FACE_OUTER_BOUND ( 'NONE', #7706, .T. ) ;
#53275 = FACE_OUTER_BOUND ( 'NONE', #364, .T. ) ;
#53276 = CARTESIAN_POINT ( 'NONE',  ( -14.83682921977595548, 13.52632505182701017, -1.500000000000002220 ) ) ;
#53277 = CARTESIAN_POINT ( 'NONE',  ( -85.52287095715009002, -23.47593901973090524, -1.443836447538996648 ) ) ;
#53278 = VERTEX_POINT ( 'NONE', #40227 ) ;
#53279 = CARTESIAN_POINT ( 'NONE',  ( -129.5562042904834072, -23.47593901973091235, -1.443836447538995760 ) ) ;
#53280 = B_SPLINE_CURVE_WITH_KNOTS ( 'NONE', 3,
 ( #86057, #100252, #70842, #1334, #32268, #18546 ),
 .UNSPECIFIED., .F., .F.,
 ( 4, 2, 4 ),
 ( 6.391158118973929294E-06, 0.001387004593080793302, 0.002767618028042612404 ),
 .UNSPECIFIED. ) ;
#53281 = CARTESIAN_POINT ( 'NONE',  ( 5.768980952343642166, -22.17701263744951490, 11.49999999999999645 ) ) ;
#53282 = CARTESIAN_POINT ( 'NONE',  ( -21.73129956901698989, 6.668506094012985663, -1.500000000000002220 ) ) ;
#53283 = CARTESIAN_POINT ( 'NONE',  ( 5.514125806255895004E-17, -29.50250786944455328, 11.44777956126000618 ) ) ;
#53284 = DIRECTION ( 'NONE',  ( -1.000000000000000000, 0.000000000000000000, 0.000000000000000000 ) ) ;
#53285 = CARTESIAN_POINT ( 'NONE',  ( -39.66885951848129821, -25.23677723931214700, 3.617518980680364038 ) ) ;
#53286 = CARTESIAN_POINT ( 'NONE',  ( -89.58953762381671027, -23.47593901973091235, -1.443836447539002865 ) ) ;
#53287 = CARTESIAN_POINT ( 'NONE',  ( -118.6228709571500559, -24.66019654487200086, 8.947790411086117501 ) ) ;
#53288 = AXIS2_PLACEMENT_3D ( 'NONE', #10950, #3848, #50025 ) ;
#53289 = EDGE_CURVE ( 'NONE', #53154, #90318, #53959, .T. ) ;
#53290 = DIRECTION ( 'NONE',  ( -1.333806637208504346E-15, 6.669033186042521139E-15, -1.000000000000000000 ) ) ;
#53291 = ORIENTED_EDGE ( 'NONE', *, *, #80942, .F. ) ;
#53292 = CARTESIAN_POINT ( 'NONE',  ( -19.47531982339030776, -5.969937916086089480, 11.49999999999998934 ) ) ;
#53293 = VERTEX_POINT ( 'NONE', #70170 ) ;
#53294 = CARTESIAN_POINT ( 'NONE',  ( 19.50756536182865020, -12.10693203178887423, -1.500000000000002220 ) ) ;
#53295 = DIRECTION ( 'NONE',  ( 1.000000000000000000, 0.000000000000000000, -0.000000000000000000 ) ) ;
#53296 = ORIENTED_EDGE ( 'NONE', *, *, #14202, .T. ) ;
#53297 = DIRECTION ( 'NONE',  ( 0.5630016722799275897, 7.885106708985486076E-16, -0.8264557562326038109 ) ) ;
#53298 = LINE ( 'NONE', #59407, #17747 ) ;
#53299 = B_SPLINE_CURVE_WITH_KNOTS ( 'NONE', 3,
 ( #62738, #23640, #62232, #7423 ),
 .UNSPECIFIED., .F., .F.,
 ( 4, 4 ),
 ( 0.9111506303623450043, 0.9201570616344605380 ),
 .UNSPECIFIED. ) ;
#53300 = CARTESIAN_POINT ( 'NONE',  ( -40.62287095715005592, -23.47593901973091235, -1.443836447539011525 ) ) ;
#53302 = VERTEX_POINT ( 'NONE', #38714 ) ;
#53301 = CARTESIAN_POINT ( 'NONE',  ( 3.248270302591931724, 20.98854991013365279, 11.49999999999999645 ) ) ;
#53303 = ORIENTED_EDGE ( 'NONE', *, *, #24387, .T. ) ;
#53304 = CARTESIAN_POINT ( 'NONE',  ( 12.10043277420606778, 18.60588626676543100, -1.500000000000002220 ) ) ;
#53305 = CARTESIAN_POINT ( 'NONE',  ( -19.87711886888390822, 5.503898473480427711, 11.49999999999998934 ) ) ;
#53306 = ADVANCED_FACE ( 'NONE', ( #2179 ), #43391, .T. ) ;
#53307 = VERTEX_POINT ( 'NONE', #655 ) ;
#53308 = ORIENTED_EDGE ( 'NONE', *, *, #9431, .F. ) ;
#53309 = CARTESIAN_POINT ( 'NONE',  ( -109.2582164645601779, -25.27682770776893051, 5.068133765414451375 ) ) ;
#53310 = B_SPLINE_CURVE_WITH_KNOTS ( 'NONE', 3,
 ( #81956, #74345, #75827, #21534, #6327, #89573, #27678, #5328, #28669, #60137, #66261, #91060, #20056, #67747, #36289, #37282, #4836, #12930, #59631 ),
 .UNSPECIFIED., .F., .F.,
 ( 4, 1, 1, 1, 1, 1, 1, 1, 1, 1, 1, 1, 1, 1, 1, 1, 4 ),
 ( 0.000000000000000000, 0.06867706841303471144, 0.1368709585090958913, 0.2061143571452998258, 0.2775381819697287922, 0.3497719775548993604, 0.4212508361555678538, 0.4929107569233706077, 0.5670265889927378344, 0.6066141532413346082, 0.6497039535189880199, 0.6973031504846840534, 0.7490856597091360980, 0.8048806474593088733, 0.8654850057023349974, 0.9302371271531362229, 1.000000000000000000 ),
 .UNSPECIFIED. ) ;
#53311 = CARTESIAN_POINT ( 'NONE',  ( -39.18285704424624782, -25.23459596353552215, 3.598380491417637383 ) ) ;
#53312 = VERTEX_POINT ( 'NONE', #15874 ) ;
#53313 = AXIS2_PLACEMENT_3D ( 'NONE', #2462, #47140, #40529 ) ;
#53314 = DIRECTION ( 'NONE',  ( -1.000000000000000000, -0.000000000000000000, -0.000000000000000000 ) ) ;
#53315 = ADVANCED_FACE ( 'NONE', ( #71681 ), #39211, .T. ) ;
#53316 = AXIS2_PLACEMENT_3D ( 'NONE', #44815, #67164, #13343 ) ;
#53317 = ORIENTED_EDGE ( 'NONE', *, *, #62519, .F. ) ;
#53318 = B_SPLINE_CURVE_WITH_KNOTS ( 'NONE', 3,
 ( #50339, #34615, #4161, #27503, #42249, #89890 ),
 .UNSPECIFIED., .F., .F.,
 ( 4, 2, 4 ),
 ( 1.570887131794333942E-05, 0.001396322306279758904, 0.002776935741241574537 ),
 .UNSPECIFIED. ) ;
#53319 = CARTESIAN_POINT ( 'NONE',  ( -127.4728709570019589, -25.30556169000782418, 4.803960565675224892 ) ) ;
#53320 = CARTESIAN_POINT ( 'NONE',  ( -106.5228709571500900, -23.47593901973090524, -1.443836447538996204 ) ) ;
#53321 = CARTESIAN_POINT ( 'NONE',  ( 20.34438994040483806, -4.565235006643893811, -1.500000000000002220 ) ) ;
#53322 = CARTESIAN_POINT ( 'NONE',  ( -3.058130702743298901, -21.54894043062209263, 11.49999999999999645 ) ) ;
#53323 = CARTESIAN_POINT ( 'NONE',  ( -51.91874251014689179, -25.22891536400416967, 6.366542672068985276 ) ) ;
#53324 = CARTESIAN_POINT ( 'NONE',  ( -78.55878950404671457, -23.73791477778911840, 11.05961554403170588 ) ) ;
#53325 = CARTESIAN_POINT ( 'NONE',  ( -12.88509029660790617, -18.40938060607246740, 11.49999999999998934 ) ) ;
#53326 = EDGE_CURVE ( 'NONE', #84514, #69684, #7767, .T. ) ;
#53327 = VECTOR ( 'NONE', #90131, 1000.000000000000000 ) ;
#53328 = ADVANCED_FACE ( 'NONE', ( #23984 ), #45054, .T. ) ;
#53329 = CARTESIAN_POINT ( 'NONE',  ( -10.58858228176428717, 5.965225279485594001, -27.03148018517017093 ) ) ;
#53330 = VERTEX_POINT ( 'NONE', #41742 ) ;
#53331 = CARTESIAN_POINT ( 'NONE',  ( -50.52287095715006870, -24.52323809116984776, 9.355190652339430812 ) ) ;
#53332 = CARTESIAN_POINT ( 'NONE',  ( -96.52287095715001897, -24.66019654487199730, 8.947790411086115725 ) ) ;
#53333 = ADVANCED_FACE ( 'NONE', ( #65093 ), #4668, .T. ) ;
#53334 = VERTEX_POINT ( 'NONE', #27508 ) ;
#53335 = AXIS2_PLACEMENT_3D ( 'NONE', #60653, #4366, #66780 ) ;
#53336 = ORIENTED_EDGE ( 'NONE', *, *, #77510, .T. ) ;
#53337 = CARTESIAN_POINT ( 'NONE',  ( -46.59984483897366658, -23.96169478059712432, 10.65365249895718414 ) ) ;
#53338 = EDGE_LOOP ( 'NONE', ( #70668, #88876, #77440, #55684 ) ) ;
#53339 = CARTESIAN_POINT ( 'NONE',  ( 21.32124590881793225, -1.116183810207903804, -1.500000000000002220 ) ) ;
#53340 = VERTEX_POINT ( 'NONE', #35118 ) ;
#53341 = CARTESIAN_POINT ( 'NONE',  ( -5.295558097854481616, 20.35707381486366785, 11.49999999999998934 ) ) ;
#53342 = CARTESIAN_POINT ( 'NONE',  ( -30.57663643993555525, -23.78769947764003234, -0.9707498849204322378 ) ) ;
#53343 = VECTOR ( 'NONE', #95842, 1000.000000000000000 ) ;
#53344 = CARTESIAN_POINT ( 'NONE',  ( -113.5228709571500332, -23.95044443724993144, 10.65354141964649415 ) ) ;
#53345 = B_SPLINE_CURVE_WITH_KNOTS ( 'NONE', 3,
 ( #94710, #25698, #26204, #2885, #48562, #25193 ),
 .UNSPECIFIED., .F., .F.,
 ( 4, 2, 4 ),
 ( 1.570887131794638196E-05, 0.001396322306279760422, 0.002776935741241574537 ),
 .UNSPECIFIED. ) ;
#53346 = DIRECTION ( 'NONE',  ( -3.773278334453079030E-23, 0.9999999999976377785, 2.173523156925979128E-06 ) ) ;
#53347 = CARTESIAN_POINT ( 'NONE',  ( 17.71009474140864981, 13.04663522181963309, -1.500000000000002220 ) ) ;
#53348 = CARTESIAN_POINT ( 'NONE',  ( -87.62602669543169043, -24.51314013834317151, 0.6176544820404251679 ) ) ;
#53349 = VERTEX_POINT ( 'NONE', #43235 ) ;
#53350 = CARTESIAN_POINT ( 'NONE',  ( -30.64751926837171325, -23.47596703998600631, 11.44779298504228038 ) ) ;
#53351 = EDGE_CURVE ( 'NONE', #20842, #81045, #2730, .T. ) ;
#53352 = CARTESIAN_POINT ( 'NONE',  ( -84.58830421338662120, -24.35071581493543391, 9.817618358456027039 ) ) ;
#53353 = CARTESIAN_POINT ( 'NONE',  ( -130.5728709571500588, -24.37807914296825729, 0.3010598746230642719 ) ) ;
#53354 = CARTESIAN_POINT ( 'NONE',  ( -10.29676400380902734, -22.20978366736605381, 10.97511746239722008 ) ) ;
#53355 = CARTESIAN_POINT ( 'NONE',  ( 17.78463046036513617, -11.72987588014745342, -1.500000000000002220 ) ) ;
#53356 = DIRECTION ( 'NONE',  ( 3.773278334444167608E-23, -1.000000000000000000, 0.000000000000000000 ) ) ;
#53357 = CARTESIAN_POINT ( 'NONE',  ( -107.5489731280372467, -24.66019654487199730, 8.947790411086115725 ) ) ;
#53358 = B_SPLINE_CURVE_WITH_KNOTS ( 'NONE', 3,
 ( #96429, #81705, #57888, #88826 ),
 .UNSPECIFIED., .F., .F.,
 ( 4, 4 ),
 ( 1.387778780781445676E-17, 0.0001000000000000028508 ),
 .UNSPECIFIED. ) ;
#53359 = ADVANCED_FACE ( 'NONE', ( #56469 ), #87394, .T. ) ;
#53360 = CARTESIAN_POINT ( 'NONE',  ( 10.34999999999998010, 27.69999999999999929, 2.100000000000000089 ) ) ;
#53361 = CARTESIAN_POINT ( 'NONE',  ( -33.53192614058710319, -24.51314013834315375, 0.6176544820404119562 ) ) ;
#53362 = CARTESIAN_POINT ( 'NONE',  ( -14.31525571501011207, 17.33968770572689166, -1.500000000000002220 ) ) ;
#53363 = EDGE_CURVE ( 'NONE', #59077, #68398, #78900, .T. ) ;
#53364 = CARTESIAN_POINT ( 'NONE',  ( -109.9084783329273023, -25.25626643526282322, 3.571638612575483318 ) ) ;
#53365 = EDGE_LOOP ( 'NONE', ( #96773, #38468, #40293, #36454, #71799 ) ) ;
#53366 = CARTESIAN_POINT ( 'NONE',  ( -99.05911678666235787, -25.18602439098982870, 6.775663951083587655 ) ) ;
#53367 = CARTESIAN_POINT ( 'NONE',  ( -18.74126595726828626, 5.813943427813767606, 11.49999999999999645 ) ) ;
#53368 = CARTESIAN_POINT ( 'NONE',  ( -28.62287095715003460, -23.80623360916731102, -0.6494981922848278577 ) ) ;
#53369 = PLANE ( 'NONE',  #9090 ) ;
#53370 = ORIENTED_EDGE ( 'NONE', *, *, #95374, .F. ) ;
#53371 = EDGE_CURVE ( 'NONE', #81742, #96474, #38124, .T. ) ;
#53372 = CARTESIAN_POINT ( 'NONE',  ( -88.51439832242913042, -23.96169478059713853, 10.65365249895717703 ) ) ;
#53373 = CARTESIAN_POINT ( 'NONE',  ( -125.2171600754302716, -25.33572514627022798, 6.311475924823946926 ) ) ;
#53374 = CARTESIAN_POINT ( 'NONE',  ( -89.90493557854645701, -25.06732983082694588, 7.447789526168958396 ) ) ;
#53376 = EDGE_CURVE ( 'NONE', #48796, #1553, #7334, .T. ) ;
#53375 = DIRECTION ( 'NONE',  ( -0.000000000000000000, 1.000000000000000000, -0.000000000000000000 ) ) ;
#53377 = CARTESIAN_POINT ( 'NONE',  ( -18.24397684793207830, 7.494555614300850266, -1.500000000000002220 ) ) ;
#53378 = EDGE_CURVE ( 'NONE', #7123, #24236, #80179, .T. ) ;
#53379 = VERTEX_POINT ( 'NONE', #36108 ) ;
#53380 = CARTESIAN_POINT ( 'NONE',  ( 10.74487964110493188, 6.376774720514429617, -24.99341878722455235 ) ) ;
#53381 = LINE ( 'NONE', #14294, #56113 ) ;
#53382 = CALENDAR_DATE ( 2026, 9, 10 ) ;
#53383 = EDGE_LOOP ( 'NONE', ( #27870, #86629, #39339, #19729 ) ) ;
#53384 = LINE ( 'NONE', #70100, #35438 ) ;
#53385 = CARTESIAN_POINT ( 'NONE',  ( -12.84880425037202656, 0.3587747205143964613, -26.59900746623529244 ) ) ;
#53386 = LINE ( 'NONE', #30532, #92841 ) ;
#53387 = CARTESIAN_POINT ( 'NONE',  ( -100.0332803147414324, -25.26638532029810946, 7.519340188766448385 ) ) ;
#53388 = CARTESIAN_POINT ( 'NONE',  ( -1.540913562699879114, -5.876774720514410966, 19.44316438561912008 ) ) ;
#53389 = VECTOR ( 'NONE', #29192, 1000.000000000000000 ) ;
#53390 = CARTESIAN_POINT ( 'NONE',  ( -69.88050735872322150, -25.31201612363421916, 5.413835025572902637 ) ) ;
#53391 = CARTESIAN_POINT ( 'NONE',  ( -112.5228709571500616, -24.64898659630529210, 1.056161002820831474 ) ) ;
#53392 = CARTESIAN_POINT ( 'NONE',  ( 13.87436705529610492, 14.39054836566213780, -1.500000000000002220 ) ) ;
#53393 = DIRECTION ( 'NONE',  ( 1.000000000000000000, -0.000000000000000000, 0.000000000000000000 ) ) ;
#53394 = CARTESIAN_POINT ( 'NONE',  ( -45.61117613609256694, -23.85049219812685450, 10.88485053497527133 ) ) ;
#53395 = ORIENTED_EDGE ( 'NONE', *, *, #52487, .F. ) ;
#53397 = CIRCLE ( 'NONE', #9643, 2.899999999999999467 ) ;
#53396 = B_SPLINE_CURVE_WITH_KNOTS ( 'NONE', 3,
 ( #78464, #77460, #70878, #7960, #69869, #63278 ),
 .UNSPECIFIED., .F., .F.,
 ( 4, 2, 4 ),
 ( 0.000000000000000000, 0.001380901958385396351, 0.002761803916770792702 ),
 .UNSPECIFIED. ) ;
#53398 = B_SPLINE_CURVE_WITH_KNOTS ( 'NONE', 3,
 ( #31728, #93609, #41344, #55076 ),
 .UNSPECIFIED., .F., .F.,
 ( 4, 4 ),
 ( 6.938893903907228378E-18, 9.999999999999591193E-05 ),
 .UNSPECIFIED. ) ;
#53399 = AXIS2_PLACEMENT_3D ( 'NONE', #45185, #30449, #98446 ) ;
#53400 = CARTESIAN_POINT ( 'NONE',  ( 7.395977348698951737, -5.299853574627441333, -25.64291752716363249 ) ) ;
#53401 = CARTESIAN_POINT ( 'NONE',  ( -65.05438548721848235, -5.356774720514425603, 27.45402280011862572 ) ) ;
#53402 = CARTESIAN_POINT ( 'NONE',  ( 20.13489193910630703, 2.682774720514426559, -22.92085183005112370 ) ) ;
#53403 = CARTESIAN_POINT ( 'NONE',  ( -81.58232796345568261, -24.65952944569304961, 1.056160979905703901 ) ) ;
#53404 = DIRECTION ( 'NONE',  ( -1.000000000000000000, -0.000000000000000000, -0.000000000000000000 ) ) ;
#53405 = CARTESIAN_POINT ( 'NONE',  ( -1.371775545366004545, -6.376774720514413630, 20.39230070883894186 ) ) ;
#53406 = AXIS2_PLACEMENT_3D ( 'NONE', #58578, #20494, #73794 ) ;
#53407 = CARTESIAN_POINT ( 'NONE',  ( 10.34999999999999254, 4.999999999999998224, 0.000000000000000000 ) ) ;
#53408 = FACE_OUTER_BOUND ( 'NONE', #24617, .T. ) ;
#53409 = ORIENTED_EDGE ( 'NONE', *, *, #75809, .T. ) ;
#53410 = CARTESIAN_POINT ( 'NONE',  ( -20.02346298389695534, -3.155783441878276196, 11.49999999999998934 ) ) ;
#53411 = CARTESIAN_POINT ( 'NONE',  ( -61.52287095715006870, -24.50216790748205398, 0.6166512839542451774 ) ) ;
#53412 = CARTESIAN_POINT ( 'NONE',  ( -49.62287095715004170, -23.96127896941632685, -0.6493128931037893681 ) ) ;
#53413 = CARTESIAN_POINT ( 'NONE',  ( -39.52287095715006870, -23.47593901973090524, -1.443836447538997092 ) ) ;
#53414 = ORIENTED_EDGE ( 'NONE', *, *, #80012, .F. ) ;
#53415 = CARTESIAN_POINT ( 'NONE',  ( -41.32836283488544638, 6.376774720514426953, 39.26872235229541985 ) ) ;
#53416 = CARTESIAN_POINT ( 'NONE',  ( -7.326845193947049140, -5.876774720514418071, 20.33046051580616265 ) ) ;
#53417 = CARTESIAN_POINT ( 'NONE',  ( 19.99232773509726258, 2.034096180923423702, -1.500000000000002220 ) ) ;
#53418 = CARTESIAN_POINT ( 'NONE',  ( 19.39439428382967634, -8.317090367284466268, 11.49999999999999645 ) ) ;
#53419 = CARTESIAN_POINT ( 'NONE',  ( -101.5228709571500332, -23.94994826722564696, -0.6494450866342716955 ) ) ;
#53420 = CARTESIAN_POINT ( 'NONE',  ( 20.57361055066190758, -8.084994430987380909, 11.49999999999998934 ) ) ;
#53421 = CARTESIAN_POINT ( 'NONE',  ( 20.53815866822273861, -0.6333348845813139283, 11.49999999999998934 ) ) ;
#53422 = CARTESIAN_POINT ( 'NONE',  ( -32.07722060962682775, -29.50250091417111520, 8.247779886223803203 ) ) ;
#53423 = B_SPLINE_CURVE_WITH_KNOTS ( 'NONE', 3,
 ( #44726, #28001, #59452, #75651 ),
 .UNSPECIFIED., .F., .F.,
 ( 4, 4 ),
 ( 0.2489393459054682345, 0.2499400929462335941 ),
 .UNSPECIFIED. ) ;
#53424 = EDGE_CURVE ( 'NONE', #24851, #42203, #58956, .T. ) ;
#53425 = CARTESIAN_POINT ( 'NONE',  ( -60.53568055955854277, -24.73486907724917572, 1.287355809206962576 ) ) ;
#53426 = ORIENTED_EDGE ( 'NONE', *, *, #98031, .T. ) ;
#53427 = LINE ( 'NONE', #59543, #15252 ) ;
#53428 = VERTEX_POINT ( 'NONE', #37605 ) ;
#53429 = CARTESIAN_POINT ( 'NONE',  ( -5.837039262820512775, -6.376774720514413630, 19.76512419871795245 ) ) ;
#53430 = B_SPLINE_SURFACE_WITH_KNOTS ( 'NONE', 3, 1, ( 
 ( #89527, #19010 ),
 ( #11407, #81420 ),
 ( #18513, #96150 ),
 ( #66220, #58584 ),
 ( #19510, #65226 ),
 ( #41360, #87536 ),
 ( #18016, #3809 ),
 ( #71818, #80416 ),
 ( #25630, #2307 ),
 ( #41873, #10910 ),
 ( #50471, #49487 ),
 ( #88535, #95144 ),
 ( #34746, #65719 ),
 ( #73313, #2810 ),
 ( #64218, #26637 ),
 ( #3320, #81915 ),
 ( #72313, #33747 ),
 ( #33238, #72817 ),
 ( #48979, #34251 ) ),
 .UNSPECIFIED., .F., .F., .F.,
 ( 4, 1, 1, 1, 1, 1, 1, 1, 1, 1, 1, 1, 1, 1, 1, 1, 4 ),
 ( 2, 2 ),
 ( 0.000000000000000000, 0.07126869258656032269, 0.1398117850281277164, 0.2064974320993705204, 0.2715352442755388784, 0.3360818306156446722, 0.4005283877476332743, 0.4649838426509124156, 0.5300503053616137938, 0.5944234089533948495, 0.6555827099825238813, 0.7148491056365311458, 0.7721150638705993607, 0.8289992113006462437, 0.8851221627752358101, 0.9420793532637975476, 1.000000000000000000 ),
 ( 0.000000000000000000, 1.000000000000000000 ),
 .UNSPECIFIED. ) ;
#53431 = CARTESIAN_POINT ( 'NONE',  ( -67.62287095715007013, -23.72773821059536559, 11.05748984161097681 ) ) ;
#53432 = ORIENTED_EDGE ( 'NONE', *, *, #67809, .T. ) ;
#53433 = EDGE_LOOP ( 'NONE', ( #6995, #35340, #56380, #35982 ) ) ;
#53434 = ORIENTED_EDGE ( 'NONE', *, *, #39104, .T. ) ;
#53435 = CARTESIAN_POINT ( 'NONE',  ( -80.88924702628075636, -25.29868576439400840, 4.592921234843194256 ) ) ;
#53436 = CARTESIAN_POINT ( 'NONE',  ( 8.971512145086501633, -1.000000000000000888, 1.914620439586549182E-15 ) ) ;
#53437 = CARTESIAN_POINT ( 'NONE',  ( 0.3908843598833069422, -6.376774720514420736, 20.63520656483649773 ) ) ;
#53438 = CARTESIAN_POINT ( 'NONE',  ( 16.46467569749531634, 12.45148609503053017, -1.500000000000002220 ) ) ;
#53439 = B_SPLINE_CURVE_WITH_KNOTS ( 'NONE', 3,
 ( #30526, #1089, #31024, #31524, #22396, #62490, #77183, #54880 ),
 .UNSPECIFIED., .F., .F.,
 ( 4, 2, 2, 4 ),
 ( 6.391158118973815792E-06, 0.002007136338672934825, 0.003007508928949912969, 0.004007881519226891114 ),
 .UNSPECIFIED. ) ;
#53440 = CARTESIAN_POINT ( 'NONE',  ( -10.14273968512601520, 19.10955606681249463, 11.49999999999999645 ) ) ;
#53441 = VERTEX_POINT ( 'NONE', #5651 ) ;
#53442 = LINE ( 'NONE', #47324, #6170 ) ;
#53443 = CARTESIAN_POINT ( 'NONE',  ( -57.62287095715004881, -23.72773821059535138, 11.05748984161097503 ) ) ;
#53444 = CARTESIAN_POINT ( 'NONE',  ( -22.37156870845955225, 0.5457896250522937809, 11.49999999999998934 ) ) ;
#53445 = EDGE_CURVE ( 'NONE', #58220, #80787, #39013, .T. ) ;
#53446 = ADVANCED_FACE ( 'NONE', ( #68554 ), #51339, .T. ) ;
#53447 = CARTESIAN_POINT ( 'NONE',  ( -80.15527233487838998, -25.27875081312351213, 7.057877889425411055 ) ) ;
#53448 = DIRECTION ( 'NONE',  ( 0.000000000000000000, 0.000000000000000000, 1.000000000000000000 ) ) ;
#53449 = ORIENTED_EDGE ( 'NONE', *, *, #15754, .F. ) ;
#53450 = CARTESIAN_POINT ( 'NONE',  ( 32.90449424769446551, -3.618459821963367240, -13.06102137676440300 ) ) ;
#53451 = CARTESIAN_POINT ( 'NONE',  ( -49.53128083207727173, -24.66019654487198665, 8.947790411086131712 ) ) ;
#53452 = EDGE_CURVE ( 'NONE', #53334, #31601, #89995, .T. ) ;
#53453 = CARTESIAN_POINT ( 'NONE',  ( -33.52287095715006160, -24.64898659630367206, 1.056161002820817485 ) ) ;
#53454 = CARTESIAN_POINT ( 'NONE',  ( 12.70736309587848645, -16.60074808024427284, -1.500000000000002220 ) ) ;
#53455 = VERTEX_POINT ( 'NONE', #21363 ) ;
#53456 = CIRCLE ( 'NONE', #72871, 0.2500000000000011102 ) ;
#53458 = ORIENTED_EDGE ( 'NONE', *, *, #47821, .F. ) ;
#53457 = CARTESIAN_POINT ( 'NONE',  ( -67.55938062934993127, -23.73791477778911840, 11.05961554403170766 ) ) ;
#53459 = ORIENTED_EDGE ( 'NONE', *, *, #74950, .T. ) ;
#53460 = CARTESIAN_POINT ( 'NONE',  ( -109.5961252891390956, -23.48786465467241769, 11.44779295918253759 ) ) ;
#53461 = CARTESIAN_POINT ( 'NONE',  ( -1.756177585742932479, 21.11346882147791959, -1.500000000000002220 ) ) ;
#53462 = ORIENTED_EDGE ( 'NONE', *, *, #73876, .F. ) ;
#53463 = CARTESIAN_POINT ( 'NONE',  ( -122.6228709571500417, -23.47596703998600631, 11.44779298504227860 ) ) ;
#53464 = DIRECTION ( 'NONE',  ( 0.000000000000000000, -0.9999999999976377785, -2.173523156925979975E-06 ) ) ;
#53465 = CARTESIAN_POINT ( 'NONE',  ( -5.167225684058948332, 21.16526716281445530, 11.49999999999998934 ) ) ;
#53466 = CARTESIAN_POINT ( 'NONE',  ( -37.92287095715006728, -23.47596703998600276, 11.44779298504227683 ) ) ;
#53467 = AXIS2_PLACEMENT_3D ( 'NONE', #87496, #24085, #33713 ) ;
#53468 = CARTESIAN_POINT ( 'NONE',  ( -35.62287095715005592, -24.99156045073392463, 7.747789690856161648 ) ) ;
#53469 = CARTESIAN_POINT ( 'NONE',  ( 7.479587785762670471, -6.376774720514417183, 20.73799387832858088 ) ) ;
#53470 = CARTESIAN_POINT ( 'NONE',  ( -9.754611696910345131, 19.53525426502628548, -1.500000000000002220 ) ) ;
#53471 = CARTESIAN_POINT ( 'NONE',  ( -71.44479781437794941, -25.31639555109142492, 5.279211600726748443 ) ) ;
#53473 = VERTEX_POINT ( 'NONE', #82280 ) ;
#53472 = CARTESIAN_POINT ( 'NONE',  ( 1.165341552704713513, 22.26021350444069213, 11.49999999999999645 ) ) ;
#53474 = DIRECTION ( 'NONE',  ( 2.216313064514630211E-15, -7.253388211138789781E-15, 1.000000000000000000 ) ) ;
#53475 = CARTESIAN_POINT ( 'NONE',  ( -74.52287095715007581, -24.64898659630528854, 1.056161002820824368 ) ) ;
#53476 = ADVANCED_FACE ( 'NONE', ( #52337 ), #37101, .F. ) ;
#53477 = CARTESIAN_POINT ( 'NONE',  ( 30.55234109742892912, -6.376774720514427841, 1.942002712049490487 ) ) ;
#53478 = ORIENTED_EDGE ( 'NONE', *, *, #39779, .T. ) ;
#53479 = ORIENTED_EDGE ( 'NONE', *, *, #28265, .T. ) ;
#53480 = ADVANCED_FACE ( 'NONE', ( #13256 ), #5158, .F. ) ;
#53481 = VECTOR ( 'NONE', #66181, 1000.000000000000114 ) ;
#53482 = ORIENTED_EDGE ( 'NONE', *, *, #32659, .F. ) ;
#53483 = VECTOR ( 'NONE', #31545, 1000.000000000000000 ) ;
#53484 = B_SPLINE_CURVE_WITH_KNOTS ( 'NONE', 3,
 ( #15239, #46196, #91864, #36575, #68044, #14733, #98464, #98969 ),
 .UNSPECIFIED., .F., .F.,
 ( 4, 2, 2, 4 ),
 ( 0.007591603542867194493, 0.008652426217380708440, 0.009713248891894220652, 0.01183489424092124681 ),
 .UNSPECIFIED. ) ;
#53485 = CARTESIAN_POINT ( 'NONE',  ( -4.141025641025640525, -5.876774720514418959, 20.67377804487179915 ) ) ;
#53486 = CARTESIAN_POINT ( 'NONE',  ( -16.84575021678815432, -12.90291372800108505, -1.500000000000002220 ) ) ;
#53487 = CARTESIAN_POINT ( 'NONE',  ( -94.63061204461861564, -24.15543982623907482, -0.2315651400026595141 ) ) ;
#53488 = CARTESIAN_POINT ( 'NONE',  ( -95.62287095715001328, -24.14406661707766943, 10.28769366152059206 ) ) ;
#53489 = EDGE_CURVE ( 'NONE', #42575, #35496, #81961, .T. ) ;
#53490 = PLANE ( 'NONE',  #48645 ) ;
#53491 = CARTESIAN_POINT ( 'NONE',  ( -28.32169924589829080, -5.965225279485592225, -8.244178532169447848 ) ) ;
#53492 = AXIS2_PLACEMENT_3D ( 'NONE', #77780, #30623, #61603 ) ;
#53493 = CARTESIAN_POINT ( 'NONE',  ( -37.62287095715004170, -24.35013146730202394, 9.818937971375111928 ) ) ;
#53494 = CARTESIAN_POINT ( 'NONE',  ( -70.04794951447323115, -25.31059997604261369, 5.351382493944067953 ) ) ;
#53495 = ORIENTED_EDGE ( 'NONE', *, *, #49336, .F. ) ;
#53496 = CARTESIAN_POINT ( 'NONE',  ( -1.307668758097810358, 19.38731951181482671, 11.49999999999999645 ) ) ;
#53497 = DIRECTION ( 'NONE',  ( 0.000000000000000000, -1.000000000000000000, 0.000000000000000000 ) ) ;
#53498 = VERTEX_POINT ( 'NONE', #60464 ) ;
#53499 = CARTESIAN_POINT ( 'NONE',  ( 2.884397429187188333, -5.876774720514407413, 18.67943752795919110 ) ) ;
#53500 = FACE_OUTER_BOUND ( 'NONE', #30249, .T. ) ;
#53502 = EDGE_CURVE ( 'NONE', #32461, #91753, #30555, .T. ) ;
#53501 = CARTESIAN_POINT ( 'NONE',  ( 26.73860345374794889, -5.356774720514430044, -3.777353070936031898 ) ) ;
#53503 = B_SPLINE_CURVE_WITH_KNOTS ( 'NONE', 3,
 ( #19400, #4191, #98512, #5675, #83293, #20891 ),
 .UNSPECIFIED., .F., .F.,
 ( 4, 2, 4 ),
 ( 0.000000000000000000, 0.001380901958385384858, 0.002761803916770769717 ),
 .UNSPECIFIED. ) ;
#53504 = CARTESIAN_POINT ( 'NONE',  ( -110.6228709571500843, -23.47596703998600631, 11.44779298504227860 ) ) ;
#53505 = CARTESIAN_POINT ( 'NONE',  ( -18.14765110722914798, -7.448729197826248871, 11.49999999999998934 ) ) ;
#53506 = CARTESIAN_POINT ( 'NONE',  ( -41.15947890742572923, -25.27806083308631102, 4.822226191762938541 ) ) ;
#53507 = ORIENTED_EDGE ( 'NONE', *, *, #76331, .T. ) ;
#53508 = CARTESIAN_POINT ( 'NONE',  ( 20.98369277809155165, -4.918611649023987731, -1.500000000000002220 ) ) ;
#53509 = CARTESIAN_POINT ( 'NONE',  ( -33.64272694203721414, -24.15620529776627379, 10.23563542870661536 ) ) ;
#53510 = DIRECTION ( 'NONE',  ( -0.06486421869277853025, 0.000000000000000000, 0.9978940991575085961 ) ) ;
#53511 = EDGE_CURVE ( 'NONE', #69928, #49051, #91382, .T. ) ;
#53512 = DIRECTION ( 'NONE',  ( 3.773278334444166432E-23, -1.000000000000000000, 0.000000000000000000 ) ) ;
#53513 = CARTESIAN_POINT ( 'NONE',  ( 19.44587849558928738, -12.39355811350142922, -1.500000000000002220 ) ) ;
#53514 = APPLICATION_PROTOCOL_DEFINITION ( 'international standard', 'config_control_design', 1994, #94551 ) ;
#53515 = CARTESIAN_POINT ( 'NONE',  ( -93.60099715520429697, -23.48783264082477018, -1.443836473390090580 ) ) ;
#53516 = DIRECTION ( 'NONE',  ( -3.773278334453079618E-23, 0.9999999999976377785, 2.173523156925979975E-06 ) ) ;
#53517 = CARTESIAN_POINT ( 'NONE',  ( 10.87751022112437482, 17.06716278085755079, 11.49999999999999645 ) ) ;
#53518 = CARTESIAN_POINT ( 'NONE',  ( -121.6252487271805904, -24.15620529776628445, 10.23563542870660115 ) ) ;
#53519 = CARTESIAN_POINT ( 'NONE',  ( -0.02075734969026423599, 3.316774720514426456, -0.08597719988137648983 ) ) ;
#53520 = CARTESIAN_POINT ( 'NONE',  ( -110.6079876523469920, -25.29823816284334015, 2.855977437720611523 ) ) ;
#53521 = CARTESIAN_POINT ( 'NONE',  ( 0.3910256410256383042, -6.376774720514408301, 19.19230769230768985 ) ) ;
#53522 = CARTESIAN_POINT ( 'NONE',  ( -111.1213521864704035, -25.18425657249500205, 3.637108438862380222 ) ) ;
#53523 = CARTESIAN_POINT ( 'NONE',  ( 14.98761344906185577, -13.09354923471379983, -1.500000000000002220 ) ) ;
#53524 = CARTESIAN_POINT ( 'NONE',  ( -6.660000000000001030, -10.77121780415746599, 1.154761385154455366 ) ) ;
#53525 = CARTESIAN_POINT ( 'NONE',  ( -18.77405512783484198, 6.205181830411797606, -1.500000000000002220 ) ) ;
#53526 = CARTESIAN_POINT ( 'NONE',  ( -56.58745316763238264, -24.34968618360933590, 0.1864209137778786995 ) ) ;
#53527 = CARTESIAN_POINT ( 'NONE',  ( -108.5562042904833930, -24.64898659630528854, 1.056161002820831474 ) ) ;
#53528 = CARTESIAN_POINT ( 'NONE',  ( 4.621320343559625066, 12.75000000000004974, 0.000000000000000000 ) ) ;
#53529 = CARTESIAN_POINT ( 'NONE',  ( -6.067718162532647064, 19.77315050736717694, 11.49999999999999645 ) ) ;
#53530 = CARTESIAN_POINT ( 'NONE',  ( -98.55620429048339304, -24.64898659630529210, 1.056161002820829253 ) ) ;
#53531 = VECTOR ( 'NONE', #74392, 1000.000000000000114 ) ;
#53532 = CARTESIAN_POINT ( 'NONE',  ( -106.5970357503859134, -23.48783264082477729, -1.443836473390085695 ) ) ;
#53533 = CARTESIAN_POINT ( 'NONE',  ( -4.508144621425604903, 22.28865971958312997, 11.49999999999999645 ) ) ;
#53534 = VERTEX_POINT ( 'NONE', #35933 ) ;
#53535 = CARTESIAN_POINT ( 'NONE',  ( -65.62287095715005592, -23.47596703998600631, 11.44779298504227683 ) ) ;
#53536 = CARTESIAN_POINT ( 'NONE',  ( 19.75748517575715368, 5.965225279485572685, 28.87153971905864580 ) ) ;
#53537 = CARTESIAN_POINT ( 'NONE',  ( 18.63370447891095694, 7.782165041754079304, -1.500000000000002220 ) ) ;
#53538 = DIRECTION ( 'NONE',  ( -0.6392559695863496705, 6.845827386180411947E-16, -0.7689940216596069522 ) ) ;
#53539 = CARTESIAN_POINT ( 'NONE',  ( -52.62287095715005592, -23.47593901973091235, -1.443836447539009749 ) ) ;
#53540 = ORIENTED_EDGE ( 'NONE', *, *, #100288, .F. ) ;
#53541 = VERTEX_POINT ( 'NONE', #57303 ) ;
#53542 = CARTESIAN_POINT ( 'NONE',  ( 0.2885822020289898759, -6.376774720514415407, 19.94806476610988710 ) ) ;
#53543 = CARTESIAN_POINT ( 'NONE',  ( -4.124250913864588419, 22.51598698906299845, -1.500000000000002220 ) ) ;
#53544 = CARTESIAN_POINT ( 'NONE',  ( -50.67443072449054853, -25.27420569099243153, 3.321634375823972807 ) ) ;
#53545 = VECTOR ( 'NONE', #89788, 1000.000000000000114 ) ;
#53546 = CARTESIAN_POINT ( 'NONE',  ( -1.126084586642228436, -21.63456646517454729, -1.500000000000002220 ) ) ;
#53547 = FACE_OUTER_BOUND ( 'NONE', #57194, .T. ) ;
#53548 = CARTESIAN_POINT ( 'NONE',  ( -34.56115368636444174, -23.73766607897670866, -1.055555164236443133 ) ) ;
#53549 = CARTESIAN_POINT ( 'NONE',  ( -15.06743543786183714, 14.52697759824333090, 11.49999999999999645 ) ) ;
#53550 = ORIENTED_EDGE ( 'NONE', *, *, #24836, .F. ) ;
#53551 = VECTOR ( 'NONE', #12835, 1000.000000000000000 ) ;
#53552 = DIRECTION ( 'NONE',  ( 0.000000000000000000, 0.000000000000000000, -1.000000000000000000 ) ) ;
#53553 = CARTESIAN_POINT ( 'NONE',  ( -7.037580251249667462, -20.86201633182841420, 11.49999999999998934 ) ) ;
#53554 = B_SPLINE_CURVE_WITH_KNOTS ( 'NONE', 3,
 ( #3077, #99750, #62228, #39376 ),
 .UNSPECIFIED., .F., .F.,
 ( 4, 4 ),
 ( 0.000000000000000000, 9.999999999998897304E-05 ),
 .UNSPECIFIED. ) ;
#53556 = CARTESIAN_POINT ( 'NONE',  ( 32.53135143123563466, 5.965225279485572685, 6.926385399448451885 ) ) ;
#53555 = AXIS2_PLACEMENT_3D ( 'NONE', #91662, #83044, #37886 ) ;
#53557 = CARTESIAN_POINT ( 'NONE',  ( -40.62732473945732181, -25.10925769753297132, 2.839336373176108097 ) ) ;
#53558 = ORIENTED_EDGE ( 'NONE', *, *, #40169, .F. ) ;
#53559 = LINE ( 'NONE', #7354, #60619 ) ;
#53560 = CARTESIAN_POINT ( 'NONE',  ( -109.8650237084402619, -25.29042187987247914, 5.784623108531866897 ) ) ;
#53561 = AXIS2_PLACEMENT_3D ( 'NONE', #94214, #2385, #70387 ) ;
#53562 = VERTEX_POINT ( 'NONE', #28319 ) ;
#53563 = CARTESIAN_POINT ( 'NONE',  ( -72.52211241193376168, -23.48786465467241058, 11.44779295918254824 ) ) ;
#53564 = EDGE_CURVE ( 'NONE', #23842, #34210, #88235, .T. ) ;
#53565 = ORIENTED_EDGE ( 'NONE', *, *, #51413, .T. ) ;
#53566 = EDGE_CURVE ( 'NONE', #75580, #54291, #66414, .T. ) ;
#53567 = ORIENTED_EDGE ( 'NONE', *, *, #983, .T. ) ;
#53568 = CARTESIAN_POINT ( 'NONE',  ( -106.6228709571500559, -23.48783264082479150, -1.443836473390060382 ) ) ;
#53569 = CARTESIAN_POINT ( 'NONE',  ( -117.6228709571500559, -24.64965695001469115, 8.947790433994175174 ) ) ;
#53570 = CARTESIAN_POINT ( 'NONE',  ( -4.141439336867657417, -6.376774720514418959, 20.56083401959468304 ) ) ;
#53571 = CARTESIAN_POINT ( 'NONE',  ( 9.418145840992488971, -18.15903486995133065, -1.500000000000002220 ) ) ;
#53572 = EDGE_CURVE ( 'NONE', #77786, #11989, #11165, .T. ) ;
#53573 = ORIENTED_EDGE ( 'NONE', *, *, #91098, .F. ) ;
#53574 = CARTESIAN_POINT ( 'NONE',  ( -3.054691362729579751, -5.876774720514412742, 19.78730719034165375 ) ) ;
#53575 = DIRECTION ( 'NONE',  ( 0.09824042138329590335, -4.470611911092166224E-17, 0.9951627101165079203 ) ) ;
#53576 = CARTESIAN_POINT ( 'NONE',  ( 9.150000000000000355, -5.876774720514426953, -15.70000000000000284 ) ) ;
#53577 = CARTESIAN_POINT ( 'NONE',  ( -0.5504121640580519337, 22.28327991085032878, 11.49999999999998934 ) ) ;
#53578 = ADVANCED_FACE ( 'NONE', ( #82110 ), #73013, .F. ) ;
#53579 = DIRECTION ( 'NONE',  ( 0.000000000000000000, 0.9999999999976377785, 2.173523156925979975E-06 ) ) ;
#53580 = CARTESIAN_POINT ( 'NONE',  ( 16.30000000000000071, 0.000000000000000000, 0.000000000000000000 ) ) ;
#53581 = EDGE_LOOP ( 'NONE', ( #33630, #43604, #17542, #50799, #86134, #4489, #47075, #27645 ) ) ;
#53582 = CARTESIAN_POINT ( 'NONE',  ( -29.72101455834852146, -25.16604849282684953, 3.657981149200824067 ) ) ;
#53583 = CARTESIAN_POINT ( 'NONE',  ( -28.79021057664958505, -25.26248001664178489, 7.906027797108415633 ) ) ;
#53584 = CARTESIAN_POINT ( 'NONE',  ( 20.60118427460899326, -2.865472796819775958, 11.49999999999998934 ) ) ;
#53585 = VERTEX_POINT ( 'NONE', #49681 ) ;
#53587 = ORIENTED_EDGE ( 'NONE', *, *, #25437, .T. ) ;
#53586 = DIRECTION ( 'NONE',  ( -3.773278334453079618E-23, 0.9999999999976377785, 2.173523156925979975E-06 ) ) ;
#53589 = EDGE_CURVE ( 'NONE', #73517, #65188, #81440, .T. ) ;
#53588 = CARTESIAN_POINT ( 'NONE',  ( -50.45832920465950622, -25.12217862368817833, 7.100425717848583673 ) ) ;
#53590 = VERTEX_POINT ( 'NONE', #12086 ) ;
#53591 = EDGE_LOOP ( 'NONE', ( #85147, #32755, #51475, #98685 ) ) ;
#53592 = CARTESIAN_POINT ( 'NONE',  ( -6.499999999999992895, 2.239999999999997105, 2.100000000000000977 ) ) ;
#53593 = PLANE ( 'NONE',  #60986 ) ;
#53594 = CARTESIAN_POINT ( 'NONE',  ( 8.160000000000000142, -0.4583917923827244278, 5.886156785137588443 ) ) ;
#53595 = LINE ( 'NONE', #785, #48570 ) ;
#53596 = CARTESIAN_POINT ( 'NONE',  ( -92.52216712986863456, -23.48786465467241413, 11.44779295918254469 ) ) ;
#53597 = CARTESIAN_POINT ( 'NONE',  ( -73.52287095715007581, -24.66019654487199730, 8.947790411086121054 ) ) ;
#53599 = ORIENTED_EDGE ( 'NONE', *, *, #61934, .F. ) ;
#53598 = CARTESIAN_POINT ( 'NONE',  ( -18.17467834739497690, 12.62983929299386965, 11.49999999999999645 ) ) ;
#53600 = B_SPLINE_CURVE_WITH_KNOTS ( 'NONE', 3,
 ( #81614, #34443, #19201, #27327 ),
 .UNSPECIFIED., .F., .F.,
 ( 4, 4 ),
 ( 0.000000000000000000, 9.999999999997510880E-05 ),
 .UNSPECIFIED. ) ;
#53601 = DIRECTION ( 'NONE',  ( -1.000000000000000000, 0.000000000000000000, -7.994117400814786717E-16 ) ) ;
#53602 = CARTESIAN_POINT ( 'NONE',  ( -4.753580043990282888, 22.13494492317406070, -1.500000000000002220 ) ) ;
#53603 = B_SPLINE_CURVE_WITH_KNOTS ( 'NONE', 3,
 ( #46275, #595, #78700, #77202 ),
 .UNSPECIFIED., .F., .F.,
 ( 4, 4 ),
 ( 0.4290738132432640461, 0.4300745602840295723 ),
 .UNSPECIFIED. ) ;
#53605 = VERTEX_POINT ( 'NONE', #57788 ) ;
#53604 = CARTESIAN_POINT ( 'NONE',  ( -28.04500620809958633, -24.83830431419368168, 7.554707623994477927 ) ) ;
#53606 = VERTEX_POINT ( 'NONE', #10598 ) ;
#53607 = CARTESIAN_POINT ( 'NONE',  ( -57.52287095715005449, -23.47596703998600631, 11.44779298504228926 ) ) ;
#53608 = AXIS2_PLACEMENT_3D ( 'NONE', #36726, #42858, #91003 ) ;
#53609 = CARTESIAN_POINT ( 'NONE',  ( 10.61947033613929214, 17.11087026910869469, 11.49999999999998934 ) ) ;
#53610 = CARTESIAN_POINT ( 'NONE',  ( -80.62287095715007013, -25.00158670708909625, 2.256160236439165967 ) ) ;
#53611 = ORIENTED_EDGE ( 'NONE', *, *, #54512, .F. ) ;
#53612 = DIRECTION ( 'NONE',  ( 0.03244919754393515293, 0.000000000000000000, -0.9994733861282923959 ) ) ;
#53613 = CARTESIAN_POINT ( 'NONE',  ( -22.12323335113916301, -3.008119206214963981, -1.500000000000002220 ) ) ;
#53614 = ORIENTED_EDGE ( 'NONE', *, *, #96654, .T. ) ;
#53615 = ORIENTED_EDGE ( 'NONE', *, *, #34681, .T. ) ;
#53616 = DIRECTION ( 'NONE',  ( -0.000000000000000000, -0.000000000000000000, -1.000000000000000000 ) ) ;
#53617 = CARTESIAN_POINT ( 'NONE',  ( -81.17863363258938136, -25.06437624333259251, 7.413012740375775955 ) ) ;
#53618 = CARTESIAN_POINT ( 'NONE',  ( 31.64143112576189765, 0.3587747205144265483, 14.03360796525321774 ) ) ;
#53619 = EDGE_CURVE ( 'NONE', #76243, #22224, #89727, .T. ) ;
#53620 = PLANE ( 'NONE',  #40057 ) ;
#53621 = CARTESIAN_POINT ( 'NONE',  ( -80.52287095715006160, -24.99156044556202616, 7.747789690856173195 ) ) ;
#53622 = AXIS2_PLACEMENT_3D ( 'NONE', #82916, #74321, #91532 ) ;
#53623 = CARTESIAN_POINT ( 'NONE',  ( 16.94836550497923966, -9.742303593519430649, 11.49999999999998934 ) ) ;
#53624 = FACE_OUTER_BOUND ( 'NONE', #13284, .T. ) ;
#53625 = AXIS2_PLACEMENT_3D ( 'NONE', #95372, #48721, #80149 ) ;
#53626 = CARTESIAN_POINT ( 'NONE',  ( -21.39523464106120088, -1.845724655749456433, -1.500000000000002220 ) ) ;
#53627 = CARTESIAN_POINT ( 'NONE',  ( -25.54641640974780259, -24.92775264709239735, 4.381685759940232572 ) ) ;
#53628 = CARTESIAN_POINT ( 'NONE',  ( -99.52287095715006160, -24.64898659630529565, 1.056161002820829697 ) ) ;
#53629 = FACE_OUTER_BOUND ( 'NONE', #43211, .T. ) ;
#53630 = EDGE_CURVE ( 'NONE', #53265, #53605, #50172, .T. ) ;
#53631 = CARTESIAN_POINT ( 'NONE',  ( 5.898633191892585614, -22.09092271590295198, -1.500000000000002220 ) ) ;
#53632 = CALENDAR_DATE ( 2026, 9, 10 ) ;
#53633 = FACE_OUTER_BOUND ( 'NONE', #84512, .T. ) ;
#53634 = DIRECTION ( 'NONE',  ( -3.773278334453079618E-23, 0.9999999999976377785, 2.173523156925978705E-06 ) ) ;
#53635 = CARTESIAN_POINT ( 'NONE',  ( -17.55682386033230102, 9.526633247210019917, 11.49999999999999645 ) ) ;
#53636 = DIRECTION ( 'NONE',  ( -1.000000000000000000, -0.000000000000000000, -0.000000000000000000 ) ) ;
#53637 = CARTESIAN_POINT ( 'NONE',  ( -63.52287095715006160, -29.50247984919015209, -1.443849546365056913 ) ) ;
#53638 = DIRECTION ( 'NONE',  ( 0.000000000000000000, 0.000000000000000000, 1.000000000000000000 ) ) ;
#53639 = CARTESIAN_POINT ( 'NONE',  ( 0.000000000000000000, 1.826774720514426464, 0.000000000000000000 ) ) ;
#53640 = EDGE_LOOP ( 'NONE', ( #81563, #12979, #67378, #24912 ) ) ;
#53641 = FACE_OUTER_BOUND ( 'NONE', #99351, .T. ) ;
#53642 = CARTESIAN_POINT ( 'NONE',  ( -26.91814428177455909, 5.965225279485572685, 29.98490496616818746 ) ) ;
#53643 = CARTESIAN_POINT ( 'NONE',  ( 12.24854465327799424, 17.96525243877979605, 11.49999999999998934 ) ) ;
#53644 = CARTESIAN_POINT ( 'NONE',  ( -117.5562042904833930, -23.48783264082479150, -1.443836473390057717 ) ) ;
#53645 = CARTESIAN_POINT ( 'NONE',  ( -17.52035102510334141, -8.822347199899118309, -1.500000000000002220 ) ) ;
#53646 = CARTESIAN_POINT ( 'NONE',  ( -85.52287095715009002, -24.15516710230293995, 10.28746687063725673 ) ) ;
#53647 = PLANE ( 'NONE',  #71020 ) ;
#53648 = COORDINATED_UNIVERSAL_TIME_OFFSET ( 0, 0, .AHEAD. ) ;
#53649 = CARTESIAN_POINT ( 'NONE',  ( -91.52216439397189163, -23.48786465467241413, 11.44779295918254469 ) ) ;
#53650 = CARTESIAN_POINT ( 'NONE',  ( 3.323502641304225236, -6.376774720514426065, 21.72931788002195219 ) ) ;
#53651 = CARTESIAN_POINT ( 'NONE',  ( 10.70087849588422380, -17.49211976490306597, 11.49999999999999645 ) ) ;
#53652 = CARTESIAN_POINT ( 'NONE',  ( 30.61643171304413613, 3.316774720514426456, 27.37433008668288181 ) ) ;
#53653 = DIRECTION ( 'NONE',  ( 0.000000000000000000, 0.000000000000000000, 1.000000000000000000 ) ) ;
#53654 = ORIENTED_EDGE ( 'NONE', *, *, #44099, .F. ) ;
#53655 =( NAMED_UNIT ( * ) SI_UNIT ( $, .STERADIAN. ) SOLID_ANGLE_UNIT ( ) );
#53656 = CARTESIAN_POINT ( 'NONE',  ( -109.5689024885030136, -25.30516380716661473, 4.853503604351335987 ) ) ;
#53657 = CARTESIAN_POINT ( 'NONE',  ( -39.74201634257447324, -25.18430928084150722, 3.555062059022910503 ) ) ;
#53658 = CARTESIAN_POINT ( 'NONE',  ( -108.6228709571500701, -23.48783264082478794, -1.443836473390060604 ) ) ;
#53659 = DIRECTION ( 'NONE',  ( -3.491481338843133355E-15, 1.000000000000000000, -2.352173255807804438E-16 ) ) ;
#53660 = CARTESIAN_POINT ( 'NONE',  ( -123.5228709571500616, -23.47596703998600631, 11.44779298504227860 ) ) ;
#53661 = CARTESIAN_POINT ( 'NONE',  ( -119.6228709571501412, -23.73907113216991860, -1.053371485793221707 ) ) ;
#53662 = EDGE_CURVE ( 'NONE', #5623, #42138, #33357, .T. ) ;
#53663 = CARTESIAN_POINT ( 'NONE',  ( -20.21456430084473155, -11.12997698910670152, 11.49999999999999645 ) ) ;
#53664 = CARTESIAN_POINT ( 'NONE',  ( 13.80103769381473811, 18.14473668730428813, 11.49999999999998934 ) ) ;
#53665 = CARTESIAN_POINT ( 'NONE',  ( 4.518205171808153509, -5.876774720514407413, 19.05004583296150500 ) ) ;
#53666 = LINE ( 'NONE', #29810, #59352 ) ;
#53667 = CARTESIAN_POINT ( 'NONE',  ( -86.52287095715007581, -23.72773821059536914, 11.05748984161097503 ) ) ;
#53668 = CARTESIAN_POINT ( 'NONE',  ( -13.02831144489870319, 18.26546089674541307, 11.49999999999999645 ) ) ;
#53669 = CARTESIAN_POINT ( 'NONE',  ( -94.62287095715005592, -23.48786465467241769, 11.44779295918254114 ) ) ;
#53670 = LINE ( 'NONE', #24200, #28711 ) ;
#53671 = AXIS2_PLACEMENT_3D ( 'NONE', #1468, #99516, #62882 ) ;
#53672 = CARTESIAN_POINT ( 'NONE',  ( -21.90371867972833542, 1.011951690471867060, 11.49999999999998934 ) ) ;
#53673 = CARTESIAN_POINT ( 'NONE',  ( -5.596556251055551101, -6.376774720514413630, 19.35667676486397681 ) ) ;
#53674 = DIRECTION ( 'NONE',  ( -0.7689940216596069522, -5.365801633547210331E-16, 0.6392559695863496705 ) ) ;
#53675 = LINE ( 'NONE', #68392, #35738 ) ;
#53676 = CARTESIAN_POINT ( 'NONE',  ( -78.64223654750129811, -23.73766607897670511, -1.055555164236459342 ) ) ;
#53677 = DIRECTION ( 'NONE',  ( -3.773278334453080206E-23, 0.9999999999976377785, 2.173523156925979975E-06 ) ) ;
#53678 = VERTEX_POINT ( 'NONE', #74004 ) ;
#53679 = EDGE_CURVE ( 'NONE', #24333, #84073, #76559, .T. ) ;
#53680 = CARTESIAN_POINT ( 'NONE',  ( -13.28352777634190396, 15.58691228024164310, -1.500000000000002220 ) ) ;
#53681 = ORIENTED_EDGE ( 'NONE', *, *, #14856, .T. ) ;
#53682 = ORIENTED_EDGE ( 'NONE', *, *, #90154, .F. ) ;
#53683 = ORIENTED_EDGE ( 'NONE', *, *, #49385, .F. ) ;
#53684 = ORIENTED_EDGE ( 'NONE', *, *, #49399, .F. ) ;
#53685 = CARTESIAN_POINT ( 'NONE',  ( -18.27982475084466785, -14.08179083545084964, 11.49999999999998934 ) ) ;
#53686 = CARTESIAN_POINT ( 'NONE',  ( -61.51536558186042214, -23.73766607897670156, -1.055555164236459342 ) ) ;
#53687 = CARTESIAN_POINT ( 'NONE',  ( -19.34540493331696354, 6.066486871809979142, -1.500000000000002220 ) ) ;
#53688 = EDGE_CURVE ( 'NONE', #86907, #94697, #53600, .T. ) ;
#53689 = ORIENTED_EDGE ( 'NONE', *, *, #52029, .F. ) ;
#53690 = CARTESIAN_POINT ( 'NONE',  ( -122.5228709571500758, -24.50216790748203977, 0.6166512839542626079 ) ) ;
#53691 = CARTESIAN_POINT ( 'NONE',  ( -87.62287095715008434, -23.96177878511309345, 10.65340807706329862 ) ) ;
#53692 = EDGE_CURVE ( 'NONE', #67691, #67908, #43874, .T. ) ;
#53694 = LINE ( 'NONE', #29839, #39976 ) ;
#53693 = AXIS2_PLACEMENT_3D ( 'NONE', #72349, #73836, #20048 ) ;
#53695 = CARTESIAN_POINT ( 'NONE',  ( -70.65896196779819149, -23.48783264082477018, -1.443836473390095021 ) ) ;
#53697 = EDGE_LOOP ( 'NONE', ( #66522, #97035, #13207, #6270 ) ) ;
#53696 = CARTESIAN_POINT ( 'NONE',  ( -21.38522110535750542, 1.317000383210971792, 11.49999999999999645 ) ) ;
#53698 = CARTESIAN_POINT ( 'NONE',  ( -113.6228709571500559, -24.64898659630368627, 1.056161002820831474 ) ) ;
#53699 = DIRECTION ( 'NONE',  ( -1.334402673828313093E-16, -0.000000000000000000, -1.000000000000000000 ) ) ;
#53700 = EDGE_CURVE ( 'NONE', #74034, #30069, #7361, .T. ) ;
#53701 = ORIENTED_EDGE ( 'NONE', *, *, #80354, .F. ) ;
#53702 = ADVANCED_FACE ( 'NONE', ( #69380 ), #15088, .F. ) ;
#53703 = CARTESIAN_POINT ( 'NONE',  ( 20.67342648114324533, -1.018679444107209342, 11.49999999999998934 ) ) ;
#53704 = VERTEX_POINT ( 'NONE', #14079 ) ;
#53706 = ORIENTED_EDGE ( 'NONE', *, *, #88650, .T. ) ;
#53705 = CARTESIAN_POINT ( 'NONE',  ( -123.6228709571501270, -24.34917612406838217, 0.1852690917426666195 ) ) ;
#53707 = CARTESIAN_POINT ( 'NONE',  ( -68.52287095715006160, -29.50250786944525672, 11.44777988621623699 ) ) ;
#53708 = ORIENTED_EDGE ( 'NONE', *, *, #60213, .F. ) ;
#53709 = VERTEX_POINT ( 'NONE', #37435 ) ;
#53710 = CARTESIAN_POINT ( 'NONE',  ( 4.468667172983064262, -5.876774720514399419, 18.40700896291420463 ) ) ;
#53711 = ADVANCED_FACE ( 'NONE', ( #30308 ), #45554, .T. ) ;
#53712 = CARTESIAN_POINT ( 'NONE',  ( -76.52287095715011844, -23.73934037231757088, 11.05740245334328975 ) ) ;
#53713 = CARTESIAN_POINT ( 'NONE',  ( -10.95654650054425794, 19.06054500580150446, 11.49999999999999645 ) ) ;
#53714 = LINE ( 'NONE', #45595, #23623 ) ;
#53715 = CARTESIAN_POINT ( 'NONE',  ( -0.2110286175373513040, -22.56517410205234597, -1.500000000000002220 ) ) ;
#53716 = CARTESIAN_POINT ( 'NONE',  ( -20.44905293368100985, -4.654758753755802836, 11.49999999999998934 ) ) ;
#53717 = CARTESIAN_POINT ( 'NONE',  ( 0.8635838190919263857, -3.990505948720459717, 8.999999999999994671 ) ) ;
#53718 = CARTESIAN_POINT ( 'NONE',  ( 5.920986267150416538, -6.376774720514422512, 21.32549308339960348 ) ) ;
#53719 = ORIENTED_EDGE ( 'NONE', *, *, #85917, .F. ) ;
#53720 = VERTEX_POINT ( 'NONE', #53669 ) ;
#53721 = ORIENTED_EDGE ( 'NONE', *, *, #52297, .T. ) ;
#53722 = CARTESIAN_POINT ( 'NONE',  ( -36.62287095715007013, -23.73907113216990084, -1.053371485793234363 ) ) ;
#53723 = CARTESIAN_POINT ( 'NONE',  ( -7.189238790567602067, -20.27908067168375794, -1.500000000000002220 ) ) ;
#53724 = DIRECTION ( 'NONE',  ( 0.000000000000000000, -1.000000000000000000, 0.000000000000000000 ) ) ;
#53725 = VERTEX_POINT ( 'NONE', #36429 ) ;
#53726 = CARTESIAN_POINT ( 'NONE',  ( 5.126256225908648823, -20.47799061884807870, -1.500000000000002220 ) ) ;
#53727 = CARTESIAN_POINT ( 'NONE',  ( 33.69795529655567634, -0.6647747205144264315, 20.86760796525322093 ) ) ;
#53728 = CARTESIAN_POINT ( 'NONE',  ( -129.9395376238166762, -23.47593901973090524, -1.443836447538995982 ) ) ;
#53729 = CARTESIAN_POINT ( 'NONE',  ( -64.58953762381672448, -23.48783264082478084, -1.443836473390069042 ) ) ;
#53730 = CARTESIAN_POINT ( 'NONE',  ( -118.6228709571500559, -23.47593901973091235, -1.443836447538997536 ) ) ;
#53731 = LINE ( 'NONE', #83158, #87583 ) ;
#53732 = CARTESIAN_POINT ( 'NONE',  ( -4.315754209668272168, 21.71352930684897942, -1.500000000000002220 ) ) ;
#53733 = B_SPLINE_CURVE_WITH_KNOTS ( 'NONE', 3,
 ( #93932, #41675, #72618, #3115 ),
 .UNSPECIFIED., .F., .F.,
 ( 4, 4 ),
 ( 0.000000000000000000, 0.0001000000000000098033 ),
 .UNSPECIFIED. ) ;
#53734 = CARTESIAN_POINT ( 'NONE',  ( -71.52210976968737555, -23.48783264082477018, -1.443836473390092578 ) ) ;
#53735 = EDGE_CURVE ( 'NONE', #12600, #85772, #60894, .T. ) ;
#53736 = ORIENTED_EDGE ( 'NONE', *, *, #65667, .F. ) ;
#53737 = CARTESIAN_POINT ( 'NONE',  ( -51.60144572864662393, -25.24860078279246167, 5.335378098060613361 ) ) ;
#53738 = DIRECTION ( 'NONE',  ( -3.773278334453079618E-23, 0.9999999999976377785, 2.173523156925979975E-06 ) ) ;
#53739 = CARTESIAN_POINT ( 'NONE',  ( -126.5215136065718298, -23.96119346886880663, -0.6495511937832031402 ) ) ;
#53740 = EDGE_CURVE ( 'NONE', #69290, #100338, #91210, .T. ) ;
#53741 = CARTESIAN_POINT ( 'NONE',  ( 8.160000000000000142, 0.1579206558577708475, 5.788828319098143105 ) ) ;
#53742 = CARTESIAN_POINT ( 'NONE',  ( 19.04819733361787470, -3.913502273677552878, 11.49999999999998934 ) ) ;
#53743 = CARTESIAN_POINT ( 'NONE',  ( 16.24497012180664868, 13.92215130028523973, 11.49999999999998934 ) ) ;
#53744 = FACE_OUTER_BOUND ( 'NONE', #36456, .T. ) ;
#53745 = CARTESIAN_POINT ( 'NONE',  ( -106.5895376238167387, -23.48783264082479150, -1.443836473390060382 ) ) ;
#53746 = VECTOR ( 'NONE', #31787, 1000.000000000000114 ) ;
#53747 = CARTESIAN_POINT ( 'NONE',  ( -109.9161100070499515, -25.05712135967894838, 7.447789548357302891 ) ) ;
#53748 = CARTESIAN_POINT ( 'NONE',  ( -44.52287095715006160, -23.47596703998600631, 11.44779298504229281 ) ) ;
#53749 = CARTESIAN_POINT ( 'NONE',  ( 22.47986593085892437, -3.190245585651162230, -1.500000000000002220 ) ) ;
#53750 = B_SPLINE_CURVE_WITH_KNOTS ( 'NONE', 3,
 ( #62680, #762, #39319, #25090, #77371, #17486 ),
 .UNSPECIFIED., .F., .F.,
 ( 4, 2, 4 ),
 ( 1.570887131795109485E-05, 0.001396322306279764325, 0.002776935741241577573 ),
 .UNSPECIFIED. ) ;
#53751 = EDGE_CURVE ( 'NONE', #62185, #65047, #49813, .T. ) ;
#53752 = CARTESIAN_POINT ( 'NONE',  ( -98.59947353796640357, -23.48783264082476308, -1.443836473390089914 ) ) ;
#53753 = CARTESIAN_POINT ( 'NONE',  ( -57.62287095715004881, -23.48786465467241058, 11.44779295918254824 ) ) ;
#53754 = CARTESIAN_POINT ( 'NONE',  ( 10.49454761162020588, -16.79419365751139637, 11.49999999999999645 ) ) ;
#53755 = FACE_OUTER_BOUND ( 'NONE', #87138, .T. ) ;
#53756 = ORIENTED_EDGE ( 'NONE', *, *, #99470, .F. ) ;
#53757 = EDGE_CURVE ( 'NONE', #16349, #94877, #99386, .T. ) ;
#53758 = CARTESIAN_POINT ( 'NONE',  ( -53.62287095715008434, -23.95044443724990657, 10.65354141964650125 ) ) ;
#53759 = DIRECTION ( 'NONE',  ( 0.000000000000000000, -0.9999999999976377785, -2.173523156925979128E-06 ) ) ;
#53760 = CARTESIAN_POINT ( 'NONE',  ( 21.02075834227166951, -5.193550065563941942, -1.500000000000002220 ) ) ;
#53761 = DIRECTION ( 'NONE',  ( 0.000000000000000000, 0.000000000000000000, -1.000000000000000000 ) ) ;
#53762 = CARTESIAN_POINT ( 'NONE',  ( 19.02374887324148389, -3.781047496429098764, -1.500000000000002220 ) ) ;
#53763 = CARTESIAN_POINT ( 'NONE',  ( -7.999999999999996447, -5.876774720514426953, 17.50000000000000000 ) ) ;
#53764 = CARTESIAN_POINT ( 'NONE',  ( 30.93860345374796594, -0.6647747205144264315, 19.84760796525321780 ) ) ;
#53765 = CARTESIAN_POINT ( 'NONE',  ( -0.3680779360730609406, 19.82951397037014729, -1.500000000000002220 ) ) ;
#53766 = CIRCLE ( 'NONE', #76405, 1.050000000000000488 ) ;
#53767 = VERTEX_POINT ( 'NONE', #59787 ) ;
#53768 = LOCAL_TIME ( 0, 54, 15.00000000000000000, #82067 ) ;
#53769 = CARTESIAN_POINT ( 'NONE',  ( 19.83649001621966335, 4.521578618930774951, 11.49999999999999645 ) ) ;
#53770 = DIRECTION ( 'NONE',  ( 3.773278334444166432E-23, -1.000000000000000000, 0.000000000000000000 ) ) ;
#53771 = APPROVAL ( #1713, 'UNSPECIFIED' ) ;
#53772 = CARTESIAN_POINT ( 'NONE',  ( 33.63305001869471056, -3.481148584080995700, -11.52139411009015291 ) ) ;
#53773 = EDGE_LOOP ( 'NONE', ( #79718, #72534, #24072, #78224 ) ) ;
#53774 = CARTESIAN_POINT ( 'NONE',  ( -102.6269066921069850, -24.35071581493543391, 9.817618358456027039 ) ) ;
#53775 = CARTESIAN_POINT ( 'NONE',  ( -92.62287095715005592, -29.50248528299804818, 1.056150453629040253 ) ) ;
#53776 = DIRECTION ( 'NONE',  ( -0.000000000000000000, 1.000000000000000000, -0.000000000000000000 ) ) ;
#53777 = CARTESIAN_POINT ( 'NONE',  ( -40.55012497585009612, -24.15602025860895097, 10.28564288303536856 ) ) ;
#53778 = FACE_OUTER_BOUND ( 'NONE', #49354, .T. ) ;
#53779 = CARTESIAN_POINT ( 'NONE',  ( -9.072532997253766496, -17.89392090870456542, 11.49999999999998934 ) ) ;
#53780 = CARTESIAN_POINT ( 'NONE',  ( -120.5562042904833930, -25.00182538069145721, 7.747789668545100206 ) ) ;
#53781 = VERTEX_POINT ( 'NONE', #13079 ) ;
#53782 = CARTESIAN_POINT ( 'NONE',  ( -97.26334014122947735, -23.56000036390796737, 11.50200000000000067 ) ) ;
#53783 = CARTESIAN_POINT ( 'NONE',  ( -6.237877366497927234, -22.00199818733190327, 11.49999999999999645 ) ) ;
#53784 = CARTESIAN_POINT ( 'NONE',  ( -17.66434017299383896, 14.31182286555179139, 11.49999999999998934 ) ) ;
#53785 = ORIENTED_EDGE ( 'NONE', *, *, #86604, .F. ) ;
#53786 = DIRECTION ( 'NONE',  ( 0.000000000000000000, -0.000000000000000000, -1.000000000000000000 ) ) ;
#53787 = DIRECTION ( 'NONE',  ( 1.000000000000000000, 0.000000000000000000, 0.000000000000000000 ) ) ;
#53788 = CARTESIAN_POINT ( 'NONE',  ( -38.49806573675382282, -24.15620529776627379, 10.23563542870660825 ) ) ;
#53789 = FACE_OUTER_BOUND ( 'NONE', #70166, .T. ) ;
#53790 = CARTESIAN_POINT ( 'NONE',  ( -128.5213301548511708, -24.66019654487200441, 8.947790411086112172 ) ) ;
#53791 = AXIS2_PLACEMENT_3D ( 'NONE', #99731, #22116, #91632 ) ;
#53792 = CARTESIAN_POINT ( 'NONE',  ( -84.52287095715006160, -24.64898659630528854, 1.056161002820826145 ) ) ;
#53793 = VERTEX_POINT ( 'NONE', #99801 ) ;
#53794 = CARTESIAN_POINT ( 'NONE',  ( 19.78452974690265975, -4.759501717958375622, 11.49999999999998934 ) ) ;
#53795 = ORIENTED_EDGE ( 'NONE', *, *, #67075, .F. ) ;
#53796 = EDGE_CURVE ( 'NONE', #72922, #73446, #75473, .T. ) ;
#53797 = CARTESIAN_POINT ( 'NONE',  ( 9.898807498884217182, 20.75630955806377287, -1.500000000000002220 ) ) ;
#53798 = CARTESIAN_POINT ( 'NONE',  ( -37.52287095715006870, -24.65952944569304250, 1.056160979905691910 ) ) ;
#53799 = VERTEX_POINT ( 'NONE', #90719 ) ;
#53800 = CARTESIAN_POINT ( 'NONE',  ( -38.62287095715005592, -24.64898659630528144, 1.056161002820819261 ) ) ;
#53801 = CARTESIAN_POINT ( 'NONE',  ( -77.63398783460891650, -24.15620529776628800, 10.23563542870659937 ) ) ;
#53802 = CARTESIAN_POINT ( 'NONE',  ( -20.27875734969026311, -7.835183881457444599, 24.00402280011862288 ) ) ;
#53804 = ORIENTED_EDGE ( 'NONE', *, *, #52348, .T. ) ;
#53803 = CARTESIAN_POINT ( 'NONE',  ( 4.979423480801214552, 20.69870207611912605, 11.49999999999999645 ) ) ;
#53805 = EDGE_CURVE ( 'NONE', #61182, #41839, #41359, .T. ) ;
#53806 = ORIENTED_EDGE ( 'NONE', *, *, #26561, .T. ) ;
#53807 = CARTESIAN_POINT ( 'NONE',  ( 19.10802705166043580, 11.29804532628753044, 11.49999999999998934 ) ) ;
#53808 = AXIS2_PLACEMENT_3D ( 'NONE', #13689, #36534, #98423 ) ;
#53809 = ADVANCED_FACE ( 'NONE', ( #84600 ), #83090, .F. ) ;
#53810 = CARTESIAN_POINT ( 'NONE',  ( 4.765357849511589805, 20.07956653139741121, -1.500000000000002220 ) ) ;
#53811 = EDGE_LOOP ( 'NONE', ( #58376, #38653, #58234, #15621 ) ) ;
#53812 = ORIENTED_EDGE ( 'NONE', *, *, #69436, .F. ) ;
#53813 = CARTESIAN_POINT ( 'NONE',  ( -109.7388188129343831, -25.31627439868620399, 5.649347606066585037 ) ) ;
#53814 = CARTESIAN_POINT ( 'NONE',  ( 3.323502641304225236, -5.876774720514426065, 21.72931788002195219 ) ) ;
#53815 = EDGE_LOOP ( 'NONE', ( #46914, #41380, #92492, #35457 ) ) ;
#53816 = B_SPLINE_CURVE_WITH_KNOTS ( 'NONE', 3,
 ( #18299, #50752, #25406, #72594, #96421, #12169, #94915, #41648 ),
 .UNSPECIFIED., .F., .F.,
 ( 4, 2, 2, 4 ),
 ( -0.001224554619866357556, -0.0002241820295893757250, 0.0007761905606876061056, 0.002776935741241574971 ),
 .UNSPECIFIED. ) ;
#53817 = CARTESIAN_POINT ( 'NONE',  ( -91.55174515373460054, -24.15543982623907482, -0.2315651400026614848 ) ) ;
#53818 = ORIENTED_EDGE ( 'NONE', *, *, #99578, .T. ) ;
#53819 = CARTESIAN_POINT ( 'NONE',  ( -35.62287095715004881, -23.48783264082477729, -1.443836473390072372 ) ) ;
#53820 = CARTESIAN_POINT ( 'NONE',  ( -88.55620429048337883, -24.66019654487199730, 8.947790411086126383 ) ) ;
#53821 = CARTESIAN_POINT ( 'NONE',  ( -12.81329989551134751, 16.42372500408851366, -1.500000000000002220 ) ) ;
#53822 = ADVANCED_FACE ( 'NONE', ( #53169 ), #51667, .T. ) ;
#53823 = CARTESIAN_POINT ( 'NONE',  ( 9.899741330608472722, -19.37759744025533593, 11.49999999999999645 ) ) ;
#53824 = CARTESIAN_POINT ( 'NONE',  ( -102.6228709571500985, -24.35013146730205236, 9.818937971375103047 ) ) ;
#53825 = LOCAL_TIME ( 0, 54, 15.00000000000000000, #56650 ) ;
#53826 = CARTESIAN_POINT ( 'NONE',  ( -78.59205417243056502, -24.15620529776628445, 10.23563542870660292 ) ) ;
#53827 = CARTESIAN_POINT ( 'NONE',  ( 22.29217321540274099, 2.676729263222305644, 11.49999999999998934 ) ) ;
#53828 = CARTESIAN_POINT ( 'NONE',  ( -118.5922148814283332, -23.73791477778912551, 11.05961554403169878 ) ) ;
#53829 = ORIENTED_EDGE ( 'NONE', *, *, #52203, .F. ) ;
#53830 = LINE ( 'NONE', #14744, #98725 ) ;
#53831 = AXIS2_PLACEMENT_3D ( 'NONE', #3980, #35429, #97807 ) ;
#53832 = CARTESIAN_POINT ( 'NONE',  ( -57.62287095715003460, -24.65952944569304606, 1.056160979905696573 ) ) ;
#53833 = LOCAL_TIME ( 0, 54, 15.00000000000000000, #50887 ) ;
#53834 = ORIENTED_EDGE ( 'NONE', *, *, #23185, .T. ) ;
#53835 = ORIENTED_EDGE ( 'NONE', *, *, #41255, .T. ) ;
#53836 = B_SPLINE_CURVE_WITH_KNOTS ( 'NONE', 3,
 ( #39971, #33354, #64343, #62835, #56720, #80035 ),
 .UNSPECIFIED., .F., .F.,
 ( 4, 2, 4 ),
 ( 0.000000000000000000, 0.001380764517854765182, 0.002761529035709530365 ),
 .UNSPECIFIED. ) ;
#53837 = ORIENTED_EDGE ( 'NONE', *, *, #10527, .T. ) ;
#53838 = CARTESIAN_POINT ( 'NONE',  ( -21.04715019690976874, -3.721878931196799467, -1.500000000000002220 ) ) ;
#53839 = ORIENTED_EDGE ( 'NONE', *, *, #89628, .T. ) ;
#53840 = CARTESIAN_POINT ( 'NONE',  ( 18.24537196375281312, 10.48796402029766739, 11.49999999999998934 ) ) ;
#53841 = CARTESIAN_POINT ( 'NONE',  ( -30.51841394749799719, -23.78320206874146692, -0.9707498849204322378 ) ) ;
#53842 = CARTESIAN_POINT ( 'NONE',  ( -111.3646597888658079, -25.28962345428254466, 4.196480316672507094 ) ) ;
#53843 = LINE ( 'NONE', #21368, #80601 ) ;
#53844 = CARTESIAN_POINT ( 'NONE',  ( 13.70243205411677145, -17.22335469805116048, -1.500000000000002220 ) ) ;
#53845 = DIRECTION ( 'NONE',  ( 1.000000000000000000, 3.773278334444166432E-23, 8.201307841325785021E-29 ) ) ;
#53846 = ORIENTED_EDGE ( 'NONE', *, *, #43413, .T. ) ;
#53847 = LINE ( 'NONE', #78153, #51875 ) ;
#53848 = CARTESIAN_POINT ( 'NONE',  ( -107.6228709571500701, -23.47593901973091235, -1.443836447538999312 ) ) ;
#53849 = ADVANCED_FACE ( 'NONE', ( #92210 ), #22683, .F. ) ;
#53850 = CARTESIAN_POINT ( 'NONE',  ( 31.69086887328960245, -3.760767191028114631, 29.45064099519496992 ) ) ;
#53851 = CARTESIAN_POINT ( 'NONE',  ( -130.5728709571500588, -24.47827083238277623, 0.5637492489085987879 ) ) ;
#53852 = CARTESIAN_POINT ( 'NONE',  ( -10.24009726630766792, -23.09230492046942373, 8.909134979017293787 ) ) ;
#53853 = CARTESIAN_POINT ( 'NONE',  ( 18.63368790978032763, -10.32677859091227113, 11.49999999999998934 ) ) ;
#53854 = CARTESIAN_POINT ( 'NONE',  ( -31.24388727629349205, -25.15755375362809332, 2.812131853976373108 ) ) ;
#53855 = DIRECTION ( 'NONE',  ( -1.000000000000000000, -0.000000000000000000, -0.000000000000000000 ) ) ;
#53856 = EDGE_CURVE ( 'NONE', #76588, #69379, #75495, .T. ) ;
#53857 = CARTESIAN_POINT ( 'NONE',  ( -109.5228709571500616, -29.50250243563736774, 8.947779886222136270 ) ) ;
#53858 = PLANE ( 'NONE',  #96213 ) ;
#53859 = CARTESIAN_POINT ( 'NONE',  ( 20.54305097139451064, 9.177977666691313985, -1.500000000000002220 ) ) ;
#53860 = EDGE_CURVE ( 'NONE', #47188, #25509, #30378, .T. ) ;
#53861 = VECTOR ( 'NONE', #71326, 1000.000000000000114 ) ;
#53862 = CARTESIAN_POINT ( 'NONE',  ( 0.02224039135773590858, 0.3828044741864786715, 0.3828044741864790046 ) ) ;
#53863 = ORIENTED_EDGE ( 'NONE', *, *, #75191, .T. ) ;
#53864 = CARTESIAN_POINT ( 'NONE',  ( -51.46125951134513343, -25.28644161259768453, 5.846423438430858432 ) ) ;
#53865 = CARTESIAN_POINT ( 'NONE',  ( 2.166912399371504705, 19.51343182558466793, 11.49999999999999645 ) ) ;
#53866 = CARTESIAN_POINT ( 'NONE',  ( -28.62287095715006302, -23.33147402473456822, -1.443835808584760683 ) ) ;
#53867 = CARTESIAN_POINT ( 'NONE',  ( -100.6228709571500843, -23.84081130438200802, 10.88220057463249191 ) ) ;
#53868 = ORIENTED_EDGE ( 'NONE', *, *, #79834, .T. ) ;
#53869 = CARTESIAN_POINT ( 'NONE',  ( -88.59844203645263860, -23.73791477778912196, 11.05961554403170588 ) ) ;
#53870 = CARTESIAN_POINT ( 'NONE',  ( -127.4728709572982268, -25.40561138053049461, 5.197941002177326908 ) ) ;
#53871 = CARTESIAN_POINT ( 'NONE',  ( -90.93238060386713073, -25.32379766982192848, 4.367815445636563432 ) ) ;
#53872 = CARTESIAN_POINT ( 'NONE',  ( -14.12090166725071327, 13.77431136191591143, 11.49999999999998934 ) ) ;
#53873 = ORIENTED_EDGE ( 'NONE', *, *, #30517, .F. ) ;
#53874 = VECTOR ( 'NONE', #39394, 1000.000000000000000 ) ;
#53875 = CARTESIAN_POINT ( 'NONE',  ( 8.422997646657599091, 6.376774720514429617, -25.04887774224060237 ) ) ;
#53876 = CARTESIAN_POINT ( 'NONE',  ( -38.62287095715005592, -23.48783264082477373, -1.443836473390072594 ) ) ;
#53877 = EDGE_CURVE ( 'NONE', #53050, #36610, #32003, .T. ) ;
#53878 = ADVANCED_FACE ( 'NONE', ( #32507 ), #6991, .T. ) ;
#53879 = DATE_AND_TIME ( #53382, #62005 ) ;
#53880 = EDGE_LOOP ( 'NONE', ( #81331, #49312, #8345, #5768 ) ) ;
#53881 = CARTESIAN_POINT ( 'NONE',  ( -124.5228709571500900, -24.33927499327855770, 9.819080762295802955 ) ) ;
#53882 = CARTESIAN_POINT ( 'NONE',  ( -107.6228709571500701, -23.73907113216991860, -1.053371485793223261 ) ) ;
#53883 = CARTESIAN_POINT ( 'NONE',  ( 31.79364159983995464, -6.475225279485573360, -11.59305536555894278 ) ) ;
#53884 = CARTESIAN_POINT ( 'NONE',  ( -66.52287095715004739, -23.94994826722564696, -0.6494450866342730277 ) ) ;
#53885 = CARTESIAN_POINT ( 'NONE',  ( -67.62287095715005592, -23.72747288104442021, -1.053458166803662666 ) ) ;
#53886 = CARTESIAN_POINT ( 'NONE',  ( -123.9228709571500531, -23.47593901973090524, -1.443836447538996426 ) ) ;
#53887 = DIRECTION ( 'NONE',  ( 0.000000000000000000, 1.000000000000000000, 0.000000000000000000 ) ) ;
#53888 = CARTESIAN_POINT ( 'NONE',  ( 12.72590371223024697, 15.41468647733915809, -1.500000000000002220 ) ) ;
#53889 = CARTESIAN_POINT ( 'NONE',  ( -100.0924861708260636, -25.27532869707566832, 2.869718512938838728 ) ) ;
#53890 = CARTESIAN_POINT ( 'NONE',  ( -51.62026654418801996, -25.30014445700734882, 4.382141121099416559 ) ) ;
#53891 = ORIENTED_EDGE ( 'NONE', *, *, #22037, .F. ) ;
#53892 = ADVANCED_FACE ( 'NONE', ( #86289 ), #54, .F. ) ;
#53893 = EDGE_CURVE ( 'NONE', #70110, #29423, #12212, .T. ) ;
#53894 = AXIS2_PLACEMENT_3D ( 'NONE', #84543, #21633, #22133 ) ;
#53896 = CARTESIAN_POINT ( 'NONE',  ( -119.5556275160544004, -23.96119346886881019, -0.6495511937832018079 ) ) ;
#53895 = CC_DESIGN_SECURITY_CLASSIFICATION ( #16578, ( #100422 ) ) ;
#53897 = CARTESIAN_POINT ( 'NONE',  ( -110.1380102904055178, -25.18430157207432529, 3.309553953209654065 ) ) ;
#53898 = CARTESIAN_POINT ( 'NONE',  ( 29.73860345376319003, 5.356471260711259674, 19.84760796525321780 ) ) ;
#53899 = CARTESIAN_POINT ( 'NONE',  ( -106.6228709571500559, -23.48786465467241769, 11.44779295918253759 ) ) ;
#53900 = FACE_OUTER_BOUND ( 'NONE', #43373, .T. ) ;
#53901 = CARTESIAN_POINT ( 'NONE',  ( -83.60404438967992746, -23.48783264082477018, -1.443836473390093911 ) ) ;
#53902 = B_SPLINE_CURVE_WITH_KNOTS ( 'NONE', 3,
 ( #90869, #21340, #19846, #67548 ),
 .UNSPECIFIED., .F., .F.,
 ( 4, 4 ),
 ( 0.000000000000000000, 0.0001000000000000306200 ),
 .UNSPECIFIED. ) ;
#53903 = CARTESIAN_POINT ( 'NONE',  ( -66.62287095715005592, -29.50248528299804818, 1.056150453629036701 ) ) ;
#53904 = VECTOR ( 'NONE', #22637, 1000.000000000000000 ) ;
#53905 = CARTESIAN_POINT ( 'NONE',  ( -55.62287095715004170, -24.99156045073392463, 7.747789690856161648 ) ) ;
#53906 = ORIENTED_EDGE ( 'NONE', *, *, #27935, .T. ) ;
#53907 = CARTESIAN_POINT ( 'NONE',  ( 3.949161919925879172, -19.86910077469890723, -1.500000000000002220 ) ) ;
#53908 = VECTOR ( 'NONE', #17522, 1000.000000000000114 ) ;
#53909 = ADVANCED_FACE ( 'NONE', ( #57371, #11659 ), #29645, .T. ) ;
#53910 = CARTESIAN_POINT ( 'NONE',  ( -61.52287095715005449, -23.72747288104469732, -1.053458166803227458 ) ) ;
#53911 = DIRECTION ( 'NONE',  ( 1.000000000000000000, 3.773278334444167608E-23, 8.201307833595939069E-29 ) ) ;
#53912 = CARTESIAN_POINT ( 'NONE',  ( -4.993225604111835914, -5.965225279485592225, -29.11654937215278593 ) ) ;
#53913 = ORIENTED_EDGE ( 'NONE', *, *, #78278, .T. ) ;
#53914 = DIRECTION ( 'NONE',  ( 0.000000000000000000, 2.173523156925980399E-06, -0.9999999999976378895 ) ) ;
#53915 = CARTESIAN_POINT ( 'NONE',  ( 20.11291949428234105, -1.170665973999911902, -1.500000000000002220 ) ) ;
#53916 = CARTESIAN_POINT ( 'NONE',  ( 20.91448408463407205, 2.778442817847782020, 11.49999999999999645 ) ) ;
#53917 = LINE ( 'NONE', #47690, #27118 ) ;
#53918 = CARTESIAN_POINT ( 'NONE',  ( 21.13397978930849064, -6.478279476769641221, 11.49999999999998934 ) ) ;
#53919 = ADVANCED_FACE ( 'NONE', ( #35010 ), #14243, .T. ) ;
#53920 = CARTESIAN_POINT ( 'NONE',  ( 19.85418835109896563, -5.301297255791479479, 11.49999999999998934 ) ) ;
#53921 = DIRECTION ( 'NONE',  ( -0.06975647374412546897, -0.9975640502598241977, 4.700301109882544451E-17 ) ) ;
#53922 = VECTOR ( 'NONE', #43137, 1000.000000000000114 ) ;
#53923 = CARTESIAN_POINT ( 'NONE',  ( -60.52202397238360732, -23.48783264082477018, -1.443836473390097908 ) ) ;
#53924 = ORIENTED_EDGE ( 'NONE', *, *, #83125, .F. ) ;
#53925 = PLANE ( 'NONE',  #41193 ) ;
#53926 = ORIENTED_EDGE ( 'NONE', *, *, #1955, .T. ) ;
#53927 = EDGE_CURVE ( 'NONE', #20446, #80744, #7051, .T. ) ;
#53928 = CARTESIAN_POINT ( 'NONE',  ( -51.62287095715005592, -23.47593901973091235, -1.443836447539009749 ) ) ;
#53929 = CARTESIAN_POINT ( 'NONE',  ( -67.62287095715001328, -24.33927499327853639, 9.819080762295815390 ) ) ;
#53930 = ORIENTED_EDGE ( 'NONE', *, *, #50523, .F. ) ;
#53931 = EDGE_LOOP ( 'NONE', ( #8406, #60909, #36373, #28371 ) ) ;
#53932 = VERTEX_POINT ( 'NONE', #68456 ) ;
#53933 = DIRECTION ( 'NONE',  ( 1.000000000000000000, 3.773278334444167608E-23, 8.201307833595939069E-29 ) ) ;
#53934 = FACE_OUTER_BOUND ( 'NONE', #25511, .T. ) ;
#53935 = CARTESIAN_POINT ( 'NONE',  ( -68.65188857983726223, -23.48786465467241058, 11.44779295918254824 ) ) ;
#53936 = CARTESIAN_POINT ( 'NONE',  ( -10.67548511050313209, -17.69376651829569269, -1.500000000000002220 ) ) ;
#53937 = EDGE_CURVE ( 'NONE', #65105, #35590, #91774, .T. ) ;
#53938 = CARTESIAN_POINT ( 'NONE',  ( -11.89702471719568244, -18.04982639819725776, 11.49999999999999645 ) ) ;
#53939 = VERTEX_POINT ( 'NONE', #14658 ) ;
#53940 = AXIS2_PLACEMENT_3D ( 'NONE', #51929, #37688, #92462 ) ;
#53941 = DIRECTION ( 'NONE',  ( -3.773278334453079618E-23, 0.9999999999976377785, 2.173523156925979552E-06 ) ) ;
#53942 = CARTESIAN_POINT ( 'NONE',  ( 4.784292611718075072, 6.376774720514426953, -25.54547254883186014 ) ) ;
#53943 = CARTESIAN_POINT ( 'NONE',  ( -11.68221627493902126, 19.09626523228051553, 11.49999999999998934 ) ) ;
#53944 = ADVANCED_FACE ( 'NONE', ( #38002 ), #60361, .F. ) ;
#53945 = CARTESIAN_POINT ( 'NONE',  ( -79.95270946814521551, -25.27875063563014635, 6.976216295041854920 ) ) ;
#53946 = CARTESIAN_POINT ( 'NONE',  ( -53.52287095715008292, -23.94994826722564696, -0.6494450866342736939 ) ) ;
#53947 = ORIENTED_EDGE ( 'NONE', *, *, #58868, .F. ) ;
#53948 = CARTESIAN_POINT ( 'NONE',  ( -99.53084541754070358, -25.27941189621985885, 4.062821213280528809 ) ) ;
#53949 = CARTESIAN_POINT ( 'NONE',  ( -35.57119075587628032, -25.00182538069146787, 7.747789668545037145 ) ) ;
#53950 = AXIS2_PLACEMENT_3D ( 'NONE', #72227, #4211, #35165 ) ;
#53951 = DIRECTION ( 'NONE',  ( 3.773278334444166432E-23, -1.000000000000000000, 0.000000000000000000 ) ) ;
#53952 = CARTESIAN_POINT ( 'NONE',  ( 16.15719879640481338, -13.26386290209467944, -1.500000000000002220 ) ) ;
#53953 = ORIENTED_EDGE ( 'NONE', *, *, #4906, .T. ) ;
#53954 = CARTESIAN_POINT ( 'NONE',  ( -98.62287095715005592, -24.64898659630529210, 1.056161002820829697 ) ) ;
#53955 = EDGE_LOOP ( 'NONE', ( #37195, #92932, #50441, #78682 ) ) ;
#53956 = CARTESIAN_POINT ( 'NONE',  ( -109.5521097922329261, -24.35071581493543391, 9.817618358456025263 ) ) ;
#53957 = CARTESIAN_POINT ( 'NONE',  ( -19.38594737788604405, 8.525550480899875438, -1.500000000000002220 ) ) ;
#53958 = ORIENTED_EDGE ( 'NONE', *, *, #44609, .F. ) ;
#53959 = LINE ( 'NONE', #54956, #52701 ) ;
#53960 = CARTESIAN_POINT ( 'NONE',  ( 31.27206728860909024, -4.132774720514318822, -3.930752063305056332 ) ) ;
#53961 = CARTESIAN_POINT ( 'NONE',  ( -3.523925741820590929, 21.50064390955241578, 11.49999999999998934 ) ) ;
#53962 = DIRECTION ( 'NONE',  ( 0.000000000000000000, -2.173523156925980399E-06, 0.9999999999976378895 ) ) ;
#53963 = CARTESIAN_POINT ( 'NONE',  ( -127.4728709571500360, -25.30558663486607429, 5.000950657679038791 ) ) ;
#53964 = CARTESIAN_POINT ( 'NONE',  ( -80.22287095715005023, -23.47593901973090169, -1.443836447538997092 ) ) ;
#53965 = CARTESIAN_POINT ( 'NONE',  ( 19.23208339725441007, -10.27600428404867827, -1.500000000000002220 ) ) ;
#53966 = CARTESIAN_POINT ( 'NONE',  ( -71.22803624472236095, -25.31639477183338727, 4.920688597080680182 ) ) ;
#53967 = ORIENTED_EDGE ( 'NONE', *, *, #79106, .F. ) ;
#53968 = CARTESIAN_POINT ( 'NONE',  ( -41.62287095715005592, -24.33832256527048088, 0.1851278514138586795 ) ) ;
#53969 = CARTESIAN_POINT ( 'NONE',  ( -81.52287095715006160, -29.50250243563736774, 8.947779886222141599 ) ) ;
#53970 = CARTESIAN_POINT ( 'NONE',  ( 32.65112488154859705, -3.727967435732443047, -2.714891177973568492 ) ) ;
#53971 = ORIENTED_EDGE ( 'NONE', *, *, #50774, .T. ) ;
#53972 = EDGE_LOOP ( 'NONE', ( #23331, #80164, #70289, #63383 ) ) ;
#53973 = VECTOR ( 'NONE', #56770, 1000.000000000000000 ) ;
#53974 = ADVANCED_FACE ( 'NONE', ( #43624 ), #52731, .T. ) ;
#53975 = ORIENTED_EDGE ( 'NONE', *, *, #77430, .T. ) ;
#53976 = LOCAL_TIME ( 0, 54, 15.00000000000000000, #15062 ) ;
#53977 = CARTESIAN_POINT ( 'NONE',  ( -126.5228709571500616, -23.47596703998600631, 11.44779298504227683 ) ) ;
#53978 = CARTESIAN_POINT ( 'NONE',  ( -17.78888362263414535, -11.56919986243916654, 11.49999999999998934 ) ) ;
#53979 = CARTESIAN_POINT ( 'NONE',  ( -94.51280176992308668, -24.15543982623907482, -0.2315651400026595141 ) ) ;
#53980 = CARTESIAN_POINT ( 'NONE',  ( -79.25918010276897974, -25.03138170620638192, 6.969965952212820781 ) ) ;
#53981 = CARTESIAN_POINT ( 'NONE',  ( -99.62287095715005592, -24.64898659630367916, 1.056161002820829697 ) ) ;
#53982 = CARTESIAN_POINT ( 'NONE',  ( 6.420673076923079314, -5.876774720514427841, 21.83974358974358765 ) ) ;
#53984 = CARTESIAN_POINT ( 'NONE',  ( -15.38109395195050233, 11.78095549196778258, -1.500000000000002220 ) ) ;
#53983 = VECTOR ( 'NONE', #81710, 1000.000000000000000 ) ;
#53985 = CARTESIAN_POINT ( 'NONE',  ( -39.03228499389064154, -25.11539320593059443, 2.804431443241629740 ) ) ;
#53986 = ORIENTED_EDGE ( 'NONE', *, *, #50918, .T. ) ;
#53987 = CARTESIAN_POINT ( 'NONE',  ( 16.42231304340664266, 10.40281881132301045, 11.49999999999999645 ) ) ;
#53988 = DIRECTION ( 'NONE',  ( 3.773278334444166432E-23, -1.000000000000000000, 0.000000000000000000 ) ) ;
#53989 = VECTOR ( 'NONE', #18764, 1000.000000000000114 ) ;
#53990 = CARTESIAN_POINT ( 'NONE',  ( -56.62287095715005592, -29.50248528299804818, 1.056150453629034924 ) ) ;
#53991 = ORIENTED_EDGE ( 'NONE', *, *, #3104, .F. ) ;
#53992 = CARTESIAN_POINT ( 'NONE',  ( 6.573941812937369455, 1.185825954564562440E-17, -0.2639660507643281639 ) ) ;
#53993 = DIRECTION ( 'NONE',  ( 1.000000000000000000, 3.773278334444167608E-23, 8.201307833595939069E-29 ) ) ;
#53994 = CARTESIAN_POINT ( 'NONE',  ( -31.62287095715005236, -29.50248528299804818, 1.056150453629029817 ) ) ;
#53995 = CARTESIAN_POINT ( 'NONE',  ( -101.1673844919198899, -25.22725712084274008, 3.624116959731904952 ) ) ;
#53996 = CARTESIAN_POINT ( 'NONE',  ( -6.723608784814384620, 18.44229941887336821, -1.500000000000002220 ) ) ;
#53997 = B_SPLINE_SURFACE_WITH_KNOTS ( 'NONE', 3, 1, ( 
 ( #24270, #62347 ),
 ( #54738, #31888 ),
 ( #16152, #85166 ),
 ( #32385, #47123 ),
 ( #100367, #30884 ),
 ( #78036, #55243 ) ),
 .UNSPECIFIED., .F., .F., .F.,
 ( 4, 1, 1, 4 ),
 ( 2, 2 ),
 ( 0.3456157426780491759, 0.5751927948816943914, 0.7454075661435733968, 0.9439799182910603159 ),
 ( 0.000000000000000000, 1.000000000000000000 ),
 .UNSPECIFIED. ) ;
#53998 = CARTESIAN_POINT ( 'NONE',  ( 12.92500000000000426, 0.000000000000000000, 0.000000000000000000 ) ) ;
#53999 = ORIENTED_EDGE ( 'NONE', *, *, #62372, .F. ) ;
#54000 = CARTESIAN_POINT ( 'NONE',  ( 15.64208908530913256, 14.88810259432246852, 11.49999999999998934 ) ) ;
#54001 = PLANE ( 'NONE',  #17197 ) ;
#54002 = CARTESIAN_POINT ( 'NONE',  ( -130.5728709571500588, -23.56000036390797092, -1.497999999999531040 ) ) ;
#54003 = CARTESIAN_POINT ( 'NONE',  ( 22.81105451610979173, -1.477225279485574028, -18.46691820600746681 ) ) ;
#54004 = CARTESIAN_POINT ( 'NONE',  ( 13.09964176094197441, 18.96253433080681106, -1.500000000000002220 ) ) ;
#54005 = EDGE_CURVE ( 'NONE', #51171, #61052, #86090, .T. ) ;
#54006 = APPROVAL_ROLE ( '' ) ;
#54007 = DIRECTION ( 'NONE',  ( -3.773278334453079618E-23, 0.9999999999976377785, 2.173523156925979975E-06 ) ) ;
#54008 = CARTESIAN_POINT ( 'NONE',  ( 4.016587897052070311, -6.376774720514426065, 21.44459449800855921 ) ) ;
#54009 = LINE ( 'NONE', #31650, #31667 ) ;
#54010 = CARTESIAN_POINT ( 'NONE',  ( -64.62287095715005592, -23.48786465467241413, 11.44779295918254824 ) ) ;
#54011 = FACE_OUTER_BOUND ( 'NONE', #90006, .T. ) ;
#54012 = LINE ( 'NONE', #92552, #32645 ) ;
#54013 = CARTESIAN_POINT ( 'NONE',  ( -114.6244179104245688, -24.51419770103159124, 9.386484678747160970 ) ) ;
#54014 = CARTESIAN_POINT ( 'NONE',  ( 7.614665684681447111, -18.39110272641453037, -1.500000000000002220 ) ) ;
#54015 = VECTOR ( 'NONE', #32483, 1000.000000000000000 ) ;
#54017 = ADVANCED_FACE ( 'NONE', ( #20761 ), #76051, .T. ) ;
#54016 = CARTESIAN_POINT ( 'NONE',  ( 2.100208336950355914, 0.000000000000000000, 0.000000000000000000 ) ) ;
#54018 = CARTESIAN_POINT ( 'NONE',  ( 9.171884637996585710, -17.55225146786146695, -1.500000000000002220 ) ) ;
#54019 = EDGE_CURVE ( 'NONE', #50012, #60701, #33977, .T. ) ;
#54020 = CARTESIAN_POINT ( 'NONE',  ( -56.60507748122925165, -23.73766607897670511, -1.055555164236459342 ) ) ;
#54021 = EDGE_CURVE ( 'NONE', #24252, #503, #27891, .T. ) ;
#54022 = VECTOR ( 'NONE', #58148, 1000.000000000000000 ) ;
#54024 = ADVANCED_FACE ( 'NONE', ( #83671 ), #44122, .T. ) ;
#54023 = UNCERTAINTY_MEASURE_WITH_UNIT (LENGTH_MEASURE( 1.000000000000000082E-05 ), #16563, 'distance_accuracy_value', 'NONE');
#54025 = CARTESIAN_POINT ( 'NONE',  ( 282.9764569301858046, 0.3587747205144265483, 20.79159422840526616 ) ) ;
#54026 = DIRECTION ( 'NONE',  ( -3.773278334453079618E-23, 0.9999999999976377785, 2.173523156925979975E-06 ) ) ;
#54027 = CARTESIAN_POINT ( 'NONE',  ( -5.954758479537505700, 19.85987847461844424, 11.49999999999999645 ) ) ;
#54028 = CARTESIAN_POINT ( 'NONE',  ( -7.627782137226129855, -6.376774720514413630, 20.04377961306771994 ) ) ;
#54029 = CARTESIAN_POINT ( 'NONE',  ( -49.68170153635294639, -25.31439325082426706, 5.417898099858684091 ) ) ;
#54030 = CARTESIAN_POINT ( 'NONE',  ( 15.01325480956343483, 17.08929600257393489, 11.49999999999999645 ) ) ;
#54031 = VERTEX_POINT ( 'NONE', #67462 ) ;
#54032 = PLANE ( 'NONE',  #38149 ) ;
#54033 = CARTESIAN_POINT ( 'NONE',  ( -52.62287095715004170, -23.47596703998600276, 11.44779298504227505 ) ) ;
#54034 = CARTESIAN_POINT ( 'NONE',  ( 20.15506735835773000, -1.303320585059813741, -1.500000000000002220 ) ) ;
#54035 = ADVANCED_FACE ( 'NONE', ( #82176 ), #52329, .T. ) ;
#54036 = CARTESIAN_POINT ( 'NONE',  ( -29.81175120719462512, -25.25636103033882307, 4.942810967025194735 ) ) ;
#54037 = CARTESIAN_POINT ( 'NONE',  ( -95.62287095715007013, -24.14321612903115621, -0.2833117244521696776 ) ) ;
#54038 = ORIENTED_EDGE ( 'NONE', *, *, #63686, .F. ) ;
#54039 = ORIENTED_EDGE ( 'NONE', *, *, #51542, .F. ) ;
#54040 = AXIS2_PLACEMENT_3D ( 'NONE', #78283, #70687, #9277 ) ;
#54041 = EDGE_CURVE ( 'NONE', #56729, #48981, #15521, .T. ) ;
#54042 = CARTESIAN_POINT ( 'NONE',  ( -33.52287095715006160, -24.64965694238574656, 8.947790433994207149 ) ) ;
#54043 = CARTESIAN_POINT ( 'NONE',  ( 22.59171682324826236, -3.780823453261925593, -1.500000000000002220 ) ) ;
#54044 = CARTESIAN_POINT ( 'NONE',  ( -51.04387771620785941, -25.18439694560420250, 3.499820392625150767 ) ) ;
#54045 = CARTESIAN_POINT ( 'NONE',  ( 10.55456386191721663, 18.89434267519128596, -1.500000000000002220 ) ) ;
#54046 = DIRECTION ( 'NONE',  ( -0.000000000000000000, -0.000000000000000000, -1.000000000000000000 ) ) ;
#54047 = FACE_OUTER_BOUND ( 'NONE', #69789, .T. ) ;
#54048 = CARTESIAN_POINT ( 'NONE',  ( -8.544475976622297964, 19.10969517993760292, 11.49999999999999645 ) ) ;
#54049 = EDGE_LOOP ( 'NONE', ( #69161, #63734, #8496, #93242, #9988, #63423, #61752, #14095, #66281, #37407, #26249, #4003, #2205, #29724, #32562 ) ) ;
#54050 = CARTESIAN_POINT ( 'NONE',  ( -69.15592802969443653, -25.24754373336818603, 5.438241903594629001 ) ) ;
#54051 = CARTESIAN_POINT ( 'NONE',  ( -17.76638496452178018, -13.01238552544781335, -1.500000000000002220 ) ) ;
#54052 = EDGE_CURVE ( 'NONE', #8388, #74863, #22756, .T. ) ;
#54053 = DIRECTION ( 'NONE',  ( -3.773278334453079618E-23, 0.9999999999976377785, 2.173523156925979975E-06 ) ) ;
#54054 = CARTESIAN_POINT ( 'NONE',  ( -30.47287095715008576, -23.47593902499770380, -1.441415665115638456 ) ) ;
#54055 = VECTOR ( 'NONE', #81475, 1000.000000000000000 ) ;
#54056 = VERTEX_POINT ( 'NONE', #53741 ) ;
#54057 = CARTESIAN_POINT ( 'NONE',  ( 4.912344403463128728, -6.376774720514408301, 19.26008510998990886 ) ) ;
#54058 = CARTESIAN_POINT ( 'NONE',  ( -122.6228709571501128, -23.95044443724993144, 10.65354141964649948 ) ) ;
#54059 = VERTEX_POINT ( 'NONE', #47126 ) ;
#54060 = CARTESIAN_POINT ( 'NONE',  ( -72.54966452413839306, -24.15620529776627734, 10.23563542870660825 ) ) ;
#54061 = ORIENTED_EDGE ( 'NONE', *, *, #80626, .F. ) ;
#54062 = AXIS2_PLACEMENT_3D ( 'NONE', #62589, #56988, #58485 ) ;
#54063 = VERTEX_POINT ( 'NONE', #23767 ) ;
#54064 = CARTESIAN_POINT ( 'NONE',  ( -71.50227123732281598, -24.35071581493543391, 9.817618358456021710 ) ) ;
#54065 = DIRECTION ( 'NONE',  ( 0.000000000000000000, -3.740001113483016365E-15, -1.000000000000000000 ) ) ;
#54066 = CARTESIAN_POINT ( 'NONE',  ( -4.440151687742864617, -5.876774720514411854, 19.67013632031035897 ) ) ;
#54067 = CARTESIAN_POINT ( 'NONE',  ( 17.75789855128238770, 10.12834119215567164, -1.500000000000002220 ) ) ;
#54068 = EDGE_CURVE ( 'NONE', #85746, #15522, #61848, .T. ) ;
#54069 = VERTEX_POINT ( 'NONE', #30384 ) ;
#54070 = CARTESIAN_POINT ( 'NONE',  ( -99.29687923781919778, -25.25133594952260552, 6.149712203147405631 ) ) ;
#54071 = CARTESIAN_POINT ( 'NONE',  ( -10.31943567505730996, 5.151096386430394247, 28.35664311630200984 ) ) ;
#54072 = CARTESIAN_POINT ( 'NONE',  ( -29.49875734969026198, -0.3587747205144265483, 10.11402280011862587 ) ) ;
#54073 = CARTESIAN_POINT ( 'NONE',  ( 15.07672925556244969, 16.42598562245719407, 11.49999999999998934 ) ) ;
#54074 = ADVANCED_FACE ( 'NONE', ( #55246 ), #63366, .F. ) ;
#54075 = CARTESIAN_POINT ( 'NONE',  ( -4.147110899021980934, -6.376774720514418959, 20.45311193189268906 ) ) ;
#54076 = CARTESIAN_POINT ( 'NONE',  ( -88.62287095715011276, -24.51387760970723662, 9.387446482453407626 ) ) ;
#54077 = ORIENTED_EDGE ( 'NONE', *, *, #83125, .T. ) ;
#54078 = ADVANCED_FACE ( 'NONE', ( #77048 ), #86172, .F. ) ;
#54079 = PLANE ( 'NONE',  #40363 ) ;
#54080 = CARTESIAN_POINT ( 'NONE',  ( -39.52287095715006160, -24.35013146730202749, 9.818937971375113705 ) ) ;
#54081 = CARTESIAN_POINT ( 'NONE',  ( -18.54028579900546703, -9.471972883075929772, 11.49999999999998934 ) ) ;
#54082 = EDGE_LOOP ( 'NONE', ( #95883, #29395 ) ) ;
#54084 = ORIENTED_EDGE ( 'NONE', *, *, #49391, .F. ) ;
#54083 = CARTESIAN_POINT ( 'NONE',  ( 4.372949846226492632, -6.376774720514404748, 18.80635842184136308 ) ) ;
#54085 = B_SPLINE_SURFACE_WITH_KNOTS ( 'NONE', 3, 3, ( 
 ( #85167, #86670, #15655, #85673 ),
 ( #16153, #47124, #55244, #78037 ),
 ( #8550, #78543, #39504, #939 ),
 ( #86170, #39998, #32386, #24761 ),
 ( #17158, #48124, #79053, #9546 ),
 ( #40509, #51113, #35882, #80059 ),
 ( #19648, #97283, #10544, #49628 ) ),
 .UNSPECIFIED., .F., .F., .F.,
 ( 4, 3, 4 ),
 ( 4, 4 ),
 ( 0.0004766839783834679817, 0.1029713700210900945, 0.2054660560637967259 ),
 ( 0.9297305048046913267, 0.9311722053073241412 ),
 .UNSPECIFIED. ) ;
#54086 = CARTESIAN_POINT ( 'NONE',  ( -98.52287095715010423, -23.96177878511310055, 10.65340807706329507 ) ) ;
#54087 = ORIENTED_EDGE ( 'NONE', *, *, #12820, .F. ) ;
#54088 = ORIENTED_EDGE ( 'NONE', *, *, #17753, .T. ) ;
#54089 = DIRECTION ( 'NONE',  ( -1.000000000000000000, -0.000000000000000000, -0.000000000000000000 ) ) ;
#54090 = CARTESIAN_POINT ( 'NONE',  ( -121.6228709571500417, -23.48786465467241769, 11.44779295918253759 ) ) ;
#54091 = CARTESIAN_POINT ( 'NONE',  ( 5.659515148826130826, -3.316774720513238517, -27.47062408975114067 ) ) ;
#54092 = CARTESIAN_POINT ( 'NONE',  ( -40.62287095715004881, -24.63345952396255356, 9.038047939301508293 ) ) ;
#54093 = CARTESIAN_POINT ( 'NONE',  ( -92.58398631988276861, -24.66019654487200441, 8.947790411086112172 ) ) ;
#54094 = DIRECTION ( 'NONE',  ( -0.000000000000000000, 0.000000000000000000, -1.000000000000000000 ) ) ;
#54096 = EDGE_LOOP ( 'NONE', ( #56386, #81388, #60727, #44989 ) ) ;
#54095 = CARTESIAN_POINT ( 'NONE',  ( 8.998109643811913472, -20.30750954041392120, 11.49999999999999645 ) ) ;
#54097 = LINE ( 'NONE', #45978, #76431 ) ;
#54098 = ORIENTED_EDGE ( 'NONE', *, *, #73745, .F. ) ;
#54099 = VECTOR ( 'NONE', #68927, 1000.000000000000114 ) ;
#54100 = CARTESIAN_POINT ( 'NONE',  ( 22.15051849217804403, -4.756829024181505439, -1.500000000000002220 ) ) ;
#54102 = ORIENTED_EDGE ( 'NONE', *, *, #84043, .F. ) ;
#54101 = CARTESIAN_POINT ( 'NONE',  ( -115.5222181624795041, -23.48786465467241769, 11.44779295918253581 ) ) ;
#54103 = B_SPLINE_CURVE_WITH_KNOTS ( 'NONE', 3,
 ( #19838, #36081, #28456, #34591, #26967, #50318 ),
 .UNSPECIFIED., .F., .F.,
 ( 4, 2, 4 ),
 ( 1.570887131794333942E-05, 0.001396322306279758904, 0.002776935741241574537 ),
 .UNSPECIFIED. ) ;
#54104 = VECTOR ( 'NONE', #64871, 1000.000000000000000 ) ;
#54105 = EDGE_LOOP ( 'NONE', ( #30053, #79980, #68411, #27334, #10286, #1640, #81638, #20613, #86253, #22400 ) ) ;
#54106 = DIRECTION ( 'NONE',  ( 0.000000000000000000, 0.000000000000000000, -1.000000000000000000 ) ) ;
#54107 = B_SPLINE_CURVE_WITH_KNOTS ( 'NONE', 3,
 ( #63411, #24814, #46167, #94329 ),
 .UNSPECIFIED., .F., .F.,
 ( 4, 4 ),
 ( 0.008760056121740519147, 0.009760803162505871794 ),
 .UNSPECIFIED. ) ;
#54108 = CARTESIAN_POINT ( 'NONE',  ( -12.53166870608491479, 15.75175023352509385, -1.500000000000002220 ) ) ;
#54109 = CARTESIAN_POINT ( 'NONE',  ( -121.6228709571500417, -29.50247984919015209, -1.443849546365046699 ) ) ;
#54110 = ORIENTED_EDGE ( 'NONE', *, *, #37404, .T. ) ;
#54111 = DIRECTION ( 'NONE',  ( -1.000000000000000000, -3.773278334444167608E-23, -8.201307833595939069E-29 ) ) ;
#54112 = CARTESIAN_POINT ( 'NONE',  ( 21.65046080595755740, -5.567969076317650590, -1.500000000000002220 ) ) ;
#54113 = VECTOR ( 'NONE', #79994, 1000.000000000000000 ) ;
#54114 = ORIENTED_EDGE ( 'NONE', *, *, #89045, .F. ) ;
#54115 = VERTEX_POINT ( 'NONE', #100373 ) ;
#54116 = DIRECTION ( 'NONE',  ( -3.773278334453079618E-23, 0.9999999999976377785, 2.173523156925979552E-06 ) ) ;
#54117 = CARTESIAN_POINT ( 'NONE',  ( -94.50572660452756679, -24.66019654487199730, 8.947790411086121054 ) ) ;
#54118 = CARTESIAN_POINT ( 'NONE',  ( 30.45304879119406039, -1.477225279485574028, -10.07140455160086390 ) ) ;
#54119 = CARTESIAN_POINT ( 'NONE',  ( -116.5228709571500474, -24.50321055353805377, 9.387540953477515160 ) ) ;
#54120 = FACE_BOUND ( 'NONE', #12833, .T. ) ;
#54121 = CARTESIAN_POINT ( 'NONE',  ( 15.80261042061247068, 11.49252619723154112, 11.49999999999998934 ) ) ;
#54122 = CARTESIAN_POINT ( 'NONE',  ( 32.98733314340959311, 0.3587747205144265483, 2.074222136288530027 ) ) ;
#54123 = CARTESIAN_POINT ( 'NONE',  ( -0.9917595143200197416, 21.46465604038169772, -1.500000000000002220 ) ) ;
#54124 = CARTESIAN_POINT ( 'NONE',  ( -36.55620429048339304, -23.47593901973091235, -1.443836447539011525 ) ) ;
#54125 = DIRECTION ( 'NONE',  ( 0.000000000000000000, 0.000000000000000000, 1.000000000000000000 ) ) ;
#54126 = FACE_BOUND ( 'NONE', #54049, .T. ) ;
#54127 = CARTESIAN_POINT ( 'NONE',  ( 0.000000000000000000, -6.943225279485572443, 0.000000000000000000 ) ) ;
#54128 = CARTESIAN_POINT ( 'NONE',  ( 11.15996004898972771, 19.99216496293481882, -1.500000000000002220 ) ) ;
#54129 = APPROVAL_ROLE ( '' ) ;
#54130 = FACE_OUTER_BOUND ( 'NONE', #78726, .T. ) ;
#54131 = DIRECTION ( 'NONE',  ( 0.9921023176230513441, 0.000000000000000000, -0.1254312216594016538 ) ) ;
#54132 = CARTESIAN_POINT ( 'NONE',  ( -19.63739455291241498, 3.909132673056371132, 11.49999999999999645 ) ) ;
#54133 = CARTESIAN_POINT ( 'NONE',  ( -79.16633218095056179, -25.31594453621216090, 5.138964353779805094 ) ) ;
#54134 = DIRECTION ( 'NONE',  ( 1.000000000000000000, 3.773278334444166432E-23, 8.201307841325785021E-29 ) ) ;
#54135 = ADVANCED_FACE ( 'NONE', ( #70961 ), #46627, .T. ) ;
#54136 = EDGE_CURVE ( 'NONE', #62785, #74167, #5049, .T. ) ;
#54137 = CARTESIAN_POINT ( 'NONE',  ( -29.49975734969026320, -6.475225279485573360, 25.41160796525322141 ) ) ;
#54138 = DIRECTION ( 'NONE',  ( 0.000000000000000000, 0.000000000000000000, 1.000000000000000000 ) ) ;
#54139 = VERTEX_POINT ( 'NONE', #62867 ) ;
#54140 = B_SPLINE_CURVE_WITH_KNOTS ( 'NONE', 3,
 ( #40768, #95558, #92178, #71729 ),
 .UNSPECIFIED., .F., .F.,
 ( 4, 4 ),
 ( 0.000000000000000000, 0.0001000000000000028644 ),
 .UNSPECIFIED. ) ;
#54141 = CARTESIAN_POINT ( 'NONE',  ( -120.5228709571500616, -29.50250243563736774, 8.947779886222134493 ) ) ;
#54142 = DIRECTION ( 'NONE',  ( -3.773278334453079618E-23, 0.9999999999976377785, 2.173523156925979975E-06 ) ) ;
#54143 = EDGE_CURVE ( 'NONE', #30481, #78412, #30081, .T. ) ;
#54144 = CARTESIAN_POINT ( 'NONE',  ( -18.02536786162489335, -12.12045427182966861, 11.49999999999998934 ) ) ;
#54145 = CARTESIAN_POINT ( 'NONE',  ( -88.62287095715004170, -23.47596703998600631, 11.44779298504227860 ) ) ;
#54146 = CARTESIAN_POINT ( 'NONE',  ( -19.61951575358169819, -0.1233725505697131491, -1.500000000000002220 ) ) ;
#54147 = EDGE_CURVE ( 'NONE', #96665, #29762, #3808, .T. ) ;
#54148 = CARTESIAN_POINT ( 'NONE',  ( -85.52287095715006160, -23.48786465467241058, 11.44779295918254292 ) ) ;
#54149 = EDGE_CURVE ( 'NONE', #74171, #53302, #33889, .T. ) ;
#54150 = CARTESIAN_POINT ( 'NONE',  ( -109.4462232385598099, -25.31698038172532605, 4.635298210512930339 ) ) ;
#54151 = DATE_TIME_ROLE ( 'classification_date' ) ;
#54152 = CARTESIAN_POINT ( 'NONE',  ( -91.55809090141561057, -23.73791477778912196, 11.05961554403170410 ) ) ;
#54153 = CARTESIAN_POINT ( 'NONE',  ( 2.989331223418256744, -6.376774720514424288, 21.46569930292093886 ) ) ;
#54154 = CARTESIAN_POINT ( 'NONE',  ( 18.67943556539783856, 8.552475402716291697, 11.49999999999999645 ) ) ;
#54155 = CARTESIAN_POINT ( 'NONE',  ( -39.15087641650215744, -25.31438038583802808, 4.798588888368600536 ) ) ;
#54156 = DIRECTION ( 'NONE',  ( 1.000000000000000000, 0.000000000000000000, 0.000000000000000000 ) ) ;
#54157 = ORIENTED_EDGE ( 'NONE', *, *, #88043, .T. ) ;
#54158 = CARTESIAN_POINT ( 'NONE',  ( -83.62287095715007013, -23.47596703998600631, 11.44779298504227860 ) ) ;
#54159 = DIRECTION ( 'NONE',  ( 0.000000000000000000, -1.000000000000000000, 0.000000000000000000 ) ) ;
#54160 = LINE ( 'NONE', #46533, #54916 ) ;
#54161 = CARTESIAN_POINT ( 'NONE',  ( 15.10689886641524105, -3.536627728863115827, -27.28884555219614327 ) ) ;
#54162 = EDGE_CURVE ( 'NONE', #22234, #64167, #50614, .T. ) ;
#54163 = CARTESIAN_POINT ( 'NONE',  ( -25.81215951358583993, -24.61459805061084793, 6.831252646531839723 ) ) ;
#54164 = AXIS2_PLACEMENT_3D ( 'NONE', #16713, #47681, #79110 ) ;
#54165 = CARTESIAN_POINT ( 'NONE',  ( 32.24176898385614720, 6.243294140736224129, 2.116998906223433341 ) ) ;
#54166 = B_SPLINE_CURVE_WITH_KNOTS ( 'NONE', 3,
 ( #73612, #71617, #87839, #25932 ),
 .UNSPECIFIED., .F., .F.,
 ( 4, 4 ),
 ( 0.000000000000000000, 0.0001000000000000028644 ),
 .UNSPECIFIED. ) ;
#54167 = EDGE_CURVE ( 'NONE', #30443, #73380, #73455, .T. ) ;
#54168 = CARTESIAN_POINT ( 'NONE',  ( -22.63574357292403860, -4.499050354539342322, 11.49999999999999645 ) ) ;
#54169 = CARTESIAN_POINT ( 'NONE',  ( -18.69919181139871966, -13.08804974640095686, -1.500000000000002220 ) ) ;
#54170 = CARTESIAN_POINT ( 'NONE',  ( 4.328803674008796065, -5.876774720514407413, 18.75671216747623049 ) ) ;
#54171 = VECTOR ( 'NONE', #93585, 1000.000000000000000 ) ;
#54172 = DIRECTION ( 'NONE',  ( -3.773278334453079618E-23, 0.9999999999976377785, 2.173523156925979975E-06 ) ) ;
#54173 = CARTESIAN_POINT ( 'NONE',  ( -64.52287095715006160, -23.47593901973090169, -1.443836447538996870 ) ) ;
#54174 = CARTESIAN_POINT ( 'NONE',  ( 11.36419782745769069, 19.35538867594532775, 11.49999999999999645 ) ) ;
#54175 = ORIENTED_EDGE ( 'NONE', *, *, #60074, .T. ) ;
#54176 = DIRECTION ( 'NONE',  ( -3.773278334453080206E-23, 0.9999999999976377785, 2.173523156925979975E-06 ) ) ;
#54177 = CARTESIAN_POINT ( 'NONE',  ( -43.60020673645048817, -23.96119346886880663, -0.6495511937831988103 ) ) ;
#54178 = CARTESIAN_POINT ( 'NONE',  ( -16.24880213243413607, 14.73142910551002238, 11.49999999999998934 ) ) ;
#54179 = CARTESIAN_POINT ( 'NONE',  ( -5.706951327759631099, -6.376774720514413630, 19.48569229636961353 ) ) ;
#54180 = CARTESIAN_POINT ( 'NONE',  ( -87.50495267027400814, -24.51419770103156281, 9.386484678747175181 ) ) ;
#54181 = CARTESIAN_POINT ( 'NONE',  ( -104.5103228290961681, -24.65952944569304606, 1.056160979905702346 ) ) ;
#54182 = CARTESIAN_POINT ( 'NONE',  ( 12.40597316965629560, 5.152774720514427642, -26.28458722401733993 ) ) ;
#54183 = DIRECTION ( 'NONE',  ( -3.773278334453080206E-23, 0.9999999999976377785, 2.173523156925979975E-06 ) ) ;
#54184 = VERTEX_POINT ( 'NONE', #50122 ) ;
#54185 = CARTESIAN_POINT ( 'NONE',  ( -15.50425215161893355, 13.37805140191733777, 11.49999999999998934 ) ) ;
#54186 = EDGE_LOOP ( 'NONE', ( #84032, #94747, #39206, #93733 ) ) ;
#54187 = ORIENTED_EDGE ( 'NONE', *, *, #15907, .T. ) ;
#54188 = ORIENTED_EDGE ( 'NONE', *, *, #39354, .T. ) ;
#54189 = EDGE_LOOP ( 'NONE', ( #95587, #67924, #54088, #71203 ) ) ;
#54190 = CARTESIAN_POINT ( 'NONE',  ( -22.67921066581790868, 4.291001918001082771, -1.500000000000002220 ) ) ;
#54191 = DIRECTION ( 'NONE',  ( 0.000000000000000000, 0.9999999999976377785, 2.173523156925979128E-06 ) ) ;
#54192 = CARTESIAN_POINT ( 'NONE',  ( -6.898722100468609675, -19.10483383855023476, -1.500000000000002220 ) ) ;
#54193 = EDGE_LOOP ( 'NONE', ( #65566, #6028, #26113, #68755 ) ) ;
#54194 = CARTESIAN_POINT ( 'NONE',  ( -30.64751926837171325, -23.47596703998600631, 11.44779298504228038 ) ) ;
#54195 = CARTESIAN_POINT ( 'NONE',  ( -92.63717942627289403, -23.73766607897671221, -1.055555164236430477 ) ) ;
#54196 = EDGE_CURVE ( 'NONE', #38068, #46271, #36493, .T. ) ;
#54197 = CARTESIAN_POINT ( 'NONE',  ( -101.3873120667114733, -25.20683408230442879, 6.626510787099375577 ) ) ;
#54198 = CARTESIAN_POINT ( 'NONE',  ( -70.52205928114219091, -23.48783264082477018, -1.443836473390095021 ) ) ;
#54200 = ORIENTED_EDGE ( 'NONE', *, *, #90669, .T. ) ;
#54199 = CARTESIAN_POINT ( 'NONE',  ( -14.25192491085926072, -16.12266454619898326, 11.49999999999999645 ) ) ;
#54201 = CARTESIAN_POINT ( 'NONE',  ( -75.50251933352205924, -24.40034930558991277, 0.3402023900116102895 ) ) ;
#54202 = CARTESIAN_POINT ( 'NONE',  ( 15.38791554121727678, 3.579805417253320687, -28.27843079449247199 ) ) ;
#54203 = ORIENTED_EDGE ( 'NONE', *, *, #70286, .T. ) ;
#54204 = CARTESIAN_POINT ( 'NONE',  ( 17.59156710592704442, 10.99281682905060897, 11.49999999999998934 ) ) ;
#54205 = ADVANCED_FACE ( 'NONE', ( #71464 ), #87679, .F. ) ;
#54206 = ORIENTED_EDGE ( 'NONE', *, *, #33154, .T. ) ;
#54208 = ORIENTED_EDGE ( 'NONE', *, *, #70046, .T. ) ;
#54207 = DIRECTION ( 'NONE',  ( 0.8219392559241306406, -0.5637660281018075370, 0.08114015731558719968 ) ) ;
#54209 = FACE_OUTER_BOUND ( 'NONE', #84458, .T. ) ;
#54210 = CARTESIAN_POINT ( 'NONE',  ( -53.52287095715006870, -23.96127896941631263, -0.6493128931038055773 ) ) ;
#54211 = ORIENTED_EDGE ( 'NONE', *, *, #26294, .T. ) ;
#54212 = ORIENTED_EDGE ( 'NONE', *, *, #2398, .T. ) ;
#54213 = CARTESIAN_POINT ( 'NONE',  ( 4.856316114246853388, -5.876774720514406525, 19.03119074624055074 ) ) ;
#54214 = PLANE ( 'NONE',  #17335 ) ;
#54215 = CARTESIAN_POINT ( 'NONE',  ( -124.5228709571500616, -23.48786465467241769, 11.44779295918253759 ) ) ;
#54216 = CARTESIAN_POINT ( 'NONE',  ( 18.54397492014093984, 11.73900455106235086, 11.49999999999999645 ) ) ;
#54217 = DIRECTION ( 'NONE',  ( 0.000000000000000000, 0.000000000000000000, 1.000000000000000000 ) ) ;
#54218 = CARTESIAN_POINT ( 'NONE',  ( 4.940617368476682536, -22.01678987175928981, 11.49999999999998934 ) ) ;
#54219 = CARTESIAN_POINT ( 'NONE',  ( -5.413507703253908510, 20.27406835261982465, -1.500000000000002220 ) ) ;
#54220 = CARTESIAN_POINT ( 'NONE',  ( 0.1645010273463760886, 0.3687607960183654776, 1.417169167140628794 ) ) ;
#54221 = LINE ( 'NONE', #85146, #10327 ) ;
#54222 = ORIENTED_EDGE ( 'NONE', *, *, #20805, .F. ) ;
#54223 = VERTEX_POINT ( 'NONE', #11054 ) ;
#54224 = FACE_OUTER_BOUND ( 'NONE', #42994, .T. ) ;
#54225 = VECTOR ( 'NONE', #96819, 1000.000000000000000 ) ;
#54226 = CARTESIAN_POINT ( 'NONE',  ( -15.45034113870702441, -14.97902827799142500, -1.500000000000002220 ) ) ;
#54227 = CARTESIAN_POINT ( 'NONE',  ( -57.52287095715005449, -24.64898659630528854, 1.056161002820822592 ) ) ;
#54228 = VERTEX_POINT ( 'NONE', #33382 ) ;
#54229 = CARTESIAN_POINT ( 'NONE',  ( 3.428800225705347149, -20.88102749682517612, 11.49999999999998934 ) ) ;
#54230 = LINE ( 'NONE', #45610, #14141 ) ;
#54231 = CARTESIAN_POINT ( 'NONE',  ( -61.66815417520224685, -25.03722704563418944, 7.590184509431679771 ) ) ;
#54232 = CARTESIAN_POINT ( 'NONE',  ( -64.62287095715005592, -23.47593901973091235, -1.443836447539007972 ) ) ;
#54233 = CARTESIAN_POINT ( 'NONE',  ( -52.22287095715005023, -23.47593901973090169, -1.443836447538997758 ) ) ;
#54234 = CARTESIAN_POINT ( 'NONE',  ( -101.5228709571500758, -24.65952944569304606, 1.056160979905702346 ) ) ;
#54235 = CARTESIAN_POINT ( 'NONE',  ( 13.35222405703702186, 17.66689192352044913, -1.500000000000002220 ) ) ;
#54236 = CARTESIAN_POINT ( 'NONE',  ( -71.56490542036905822, -23.48783264082477018, -1.443836473390092578 ) ) ;
#54237 = AXIS2_PLACEMENT_3D ( 'NONE', #26730, #51071, #33839 ) ;
#54238 = VERTEX_POINT ( 'NONE', #41507 ) ;
#54239 = DIRECTION ( 'NONE',  ( -1.000000000000000000, -3.491481338843133355E-15, -2.352173255807796056E-16 ) ) ;
#54240 = FACE_OUTER_BOUND ( 'NONE', #23465, .T. ) ;
#54241 = CARTESIAN_POINT ( 'NONE',  ( -126.5905539433028792, -23.73766607897670156, -1.055555164236450016 ) ) ;
#54242 = CARTESIAN_POINT ( 'NONE',  ( -76.52287095715007581, -23.47593901973090169, -1.443836447538996648 ) ) ;
#54243 = DIRECTION ( 'NONE',  ( 0.000000000000000000, 0.000000000000000000, 1.000000000000000000 ) ) ;
#54244 = CARTESIAN_POINT ( 'NONE',  ( 17.65527434030279252, -8.155491144718855168, -1.500000000000002220 ) ) ;
#54245 = CARTESIAN_POINT ( 'NONE',  ( -21.04715019690976874, -3.721878931196799467, 11.49999999999998934 ) ) ;
#54246 = DIRECTION ( 'NONE',  ( -0.1875268396392987258, 0.000000000000000000, -0.9822594791677485837 ) ) ;
#54247 = B_SPLINE_CURVE_WITH_KNOTS ( 'NONE', 3,
 ( #27090, #34211, #26086, #63676, #94596, #25077, #48938, #2766 ),
 .UNSPECIFIED., .F., .F.,
 ( 4, 2, 2, 4 ),
 ( -0.001240666984355838021, -0.0002401179793394964124, 0.0007604310256768451962, 0.002761529035709528630 ),
 .UNSPECIFIED. ) ;
#54248 = CARTESIAN_POINT ( 'NONE',  ( -7.641025641025638748, -5.876774720514426953, 21.75000000000001066 ) ) ;
#54249 = LINE ( 'NONE', #44627, #37327 ) ;
#54250 = CARTESIAN_POINT ( 'NONE',  ( -44.52287095715006870, -24.33927499327855060, 9.819080762295804732 ) ) ;
#54251 = CARTESIAN_POINT ( 'NONE',  ( 2.290073164716609710, 22.57640404599860418, -1.500000000000002220 ) ) ;
#54252 = CARTESIAN_POINT ( 'NONE',  ( -124.5228709571500616, -23.48786465467241769, 11.44779295918253759 ) ) ;
#54253 = CARTESIAN_POINT ( 'NONE',  ( -127.6228709571500559, -24.51283580621365843, 0.6167428607019918019 ) ) ;
#54254 = CARTESIAN_POINT ( 'NONE',  ( -0.2410636032128395945, 19.88167143085883737, 11.49999999999999645 ) ) ;
#54255 = ADVANCED_FACE ( 'NONE', ( #27281 ), #99316, .T. ) ;
#54256 = CARTESIAN_POINT ( 'NONE',  ( 8.809764260727238394, -0.02602732333167948400, 3.697389739420775534 ) ) ;
#54257 = ORIENTED_EDGE ( 'NONE', *, *, #31541, .T. ) ;
#54258 = DIRECTION ( 'NONE',  ( 0.000000000000000000, 0.9999999999976377785, 2.173523156925979975E-06 ) ) ;
#54259 = LINE ( 'NONE', #70476, #11801 ) ;
#54260 = EDGE_CURVE ( 'NONE', #46797, #87999, #21909, .T. ) ;
#54261 = CARTESIAN_POINT ( 'NONE',  ( -68.52287095715004739, -23.73907113216989373, -1.053371485793255014 ) ) ;
#54262 = CARTESIAN_POINT ( 'NONE',  ( 10.55456386191721663, 18.89434267519128596, 11.49999999999998934 ) ) ;
#54263 = CARTESIAN_POINT ( 'NONE',  ( -56.57854487595048454, -24.66019654487199375, 8.947790411086122830 ) ) ;
#54264 = CARTESIAN_POINT ( 'NONE',  ( -9.780116039169133302, 16.78644576961053048, -1.500000000000002220 ) ) ;
#54265 = EDGE_CURVE ( 'NONE', #17321, #26032, #1953, .T. ) ;
#54266 = CARTESIAN_POINT ( 'NONE',  ( 282.9764569301858046, 0.6647747205144264315, 20.79159422840526616 ) ) ;
#54267 = CARTESIAN_POINT ( 'NONE',  ( -19.80875734969026425, -5.965225279485572685, 30.51402280011862089 ) ) ;
#54268 = CARTESIAN_POINT ( 'NONE',  ( 8.478510716907816658, 17.93336729499101523, -1.500000000000002220 ) ) ;
#54269 = EDGE_LOOP ( 'NONE', ( #9777, #64795, #61959, #49363 ) ) ;
#54270 = EDGE_CURVE ( 'NONE', #33481, #82250, #67345, .T. ) ;
#54271 = AXIS2_PLACEMENT_3D ( 'NONE', #43269, #39015, #21392 ) ;
#54272 = CARTESIAN_POINT ( 'NONE',  ( 13.49383759531269433, -15.17088004136028090, 11.49999999999999645 ) ) ;
#54273 = DIRECTION ( 'NONE',  ( -3.773278334444167608E-23, 1.000000000000000000, 0.000000000000000000 ) ) ;
#54274 = EDGE_CURVE ( 'NONE', #19368, #71172, #89692, .T. ) ;
#54275 = PLANE ( 'NONE',  #57782 ) ;
#54276 = ORIENTED_EDGE ( 'NONE', *, *, #4027, .F. ) ;
#54277 = B_SPLINE_SURFACE_WITH_KNOTS ( 'NONE', 3, 3, ( 
 ( #23927, #47280, #9202, #34927 ),
 ( #70609, #65904, #71119, #55906 ),
 ( #40671, #1609, #32547, #1102 ),
 ( #63519, #96820, #94442, #24928 ),
 ( #86829, #79214, #9714, #33056 ),
 ( #64034, #94948, #97812, #37426 ),
 ( #20186, #99310, #28307, #75964 ) ),
 .UNSPECIFIED., .F., .F., .F.,
 ( 4, 3, 4 ),
 ( 4, 4 ),
 ( 0.7945040050992238090, 0.8970133687736496775, 0.9995227324480754350 ),
 ( 0.1395294536136304497, 0.1406065942234439314 ),
 .UNSPECIFIED. ) ;
#54278 = CARTESIAN_POINT ( 'NONE',  ( -30.61275986115374437, -24.37728322581795481, 9.960208392924579712 ) ) ;
#54279 = PLANE ( 'NONE',  #55819 ) ;
#54280 = CARTESIAN_POINT ( 'NONE',  ( -49.13746579462012676, -25.25214525603300331, 5.391919962994458970 ) ) ;
#54281 = CARTESIAN_POINT ( 'NONE',  ( -40.67673042091735880, -23.48786465467240347, 11.44779295918255180 ) ) ;
#54282 = CARTESIAN_POINT ( 'NONE',  ( -0.6227173540047638012, -6.376774720514413630, 19.48351902941045211 ) ) ;
#54283 = CARTESIAN_POINT ( 'NONE',  ( 8.649182803842551337, -18.14983140373652404, -1.500000000000002220 ) ) ;
#54284 = CARTESIAN_POINT ( 'NONE',  ( -129.5228709571499905, -23.48783264082477729, -1.443836473390079700 ) ) ;
#54285 = ORIENTED_EDGE ( 'NONE', *, *, #48887, .T. ) ;
#54286 = B_SPLINE_CURVE_WITH_KNOTS ( 'NONE', 3,
 ( #77848, #68395, #45564, #22193, #86477, #75984 ),
 .UNSPECIFIED., .F., .F.,
 ( 4, 2, 4 ),
 ( 1.570887131794795405E-05, 0.001396322306279761940, 0.002776935741241575838 ),
 .UNSPECIFIED. ) ;
#54287 = CARTESIAN_POINT ( 'NONE',  ( -36.52287095715009002, -24.33832256527048088, 0.1851278514138557096 ) ) ;
#54288 = ADVANCED_FACE ( 'NONE', ( #82550 ), #4936, .T. ) ;
#54289 = CARTESIAN_POINT ( 'NONE',  ( -12.24191887126339751, 19.33842681661653984, 11.49999999999999645 ) ) ;
#54290 = CARTESIAN_POINT ( 'NONE',  ( -9.076218414377828836, -20.82814578352222767, -1.500000000000002220 ) ) ;
#54291 = VERTEX_POINT ( 'NONE', #12041 ) ;
#54292 = CARTESIAN_POINT ( 'NONE',  ( -45.52287095715006160, -24.92579138211019085, 1.929029949965659130 ) ) ;
#54293 = DIRECTION ( 'NONE',  ( 1.000000000000000000, 3.773278334444167020E-23, 8.201307838832447938E-29 ) ) ;
#54294 = CARTESIAN_POINT ( 'NONE',  ( -64.62287095715005592, -29.50250786944525672, 11.44777988621623876 ) ) ;
#54295 = DIRECTION ( 'NONE',  ( 0.000000000000000000, -0.000000000000000000, -1.000000000000000000 ) ) ;
#54296 = VECTOR ( 'NONE', #79218, 1000.000000000000000 ) ;
#54297 = CARTESIAN_POINT ( 'NONE',  ( -128.5895400625830405, -24.51419770103157703, 9.386484678747171628 ) ) ;
#54298 = LINE ( 'NONE', #85226, #11238 ) ;
#54299 = ORIENTED_EDGE ( 'NONE', *, *, #59473, .F. ) ;
#54300 = CARTESIAN_POINT ( 'NONE',  ( 19.51578053514377586, 5.923290232019536639, 11.49999999999998934 ) ) ;
#54301 = VERTEX_POINT ( 'NONE', #74445 ) ;
#54302 = CARTESIAN_POINT ( 'NONE',  ( -22.87025945403008365, 2.249016246415321163, -1.500000000000002220 ) ) ;
#54303 = CARTESIAN_POINT ( 'NONE',  ( -54.55345688732126774, -23.96169478059712787, 10.65365249895718947 ) ) ;
#54304 = VECTOR ( 'NONE', #74273, 1000.000000000000000 ) ;
#54305 = ORIENTED_EDGE ( 'NONE', *, *, #55124, .F. ) ;
#54306 = DIRECTION ( 'NONE',  ( -0.9978940991575084851, 0.000000000000000000, -0.06486421869277853025 ) ) ;
#54307 = VECTOR ( 'NONE', #750, 1000.000000000000000 ) ;
#54308 = CARTESIAN_POINT ( 'NONE',  ( -81.41734784726033070, -25.22106677559741783, 6.517144941221712173 ) ) ;
#54309 = CARTESIAN_POINT ( 'NONE',  ( -51.50747100937991263, -23.96169478059712787, 10.65365249895718236 ) ) ;
#54311 = ORIENTED_EDGE ( 'NONE', *, *, #32480, .F. ) ;
#54310 = CARTESIAN_POINT ( 'NONE',  ( 12.11089201280794470, -17.53110042540249225, 11.49999999999999645 ) ) ;
#54312 = ORIENTED_EDGE ( 'NONE', *, *, #37860, .T. ) ;
#54313 = CARTESIAN_POINT ( 'NONE',  ( -4.330935931041660858, -21.79039167146679290, -1.500000000000002220 ) ) ;
#54314 = CARTESIAN_POINT ( 'NONE',  ( 19.88596897151998633, -5.565664080715476913, -1.500000000000002220 ) ) ;
#54315 = ORIENTED_EDGE ( 'NONE', *, *, #13513, .F. ) ;
#54316 = ORIENTED_EDGE ( 'NONE', *, *, #93792, .T. ) ;
#54317 = CARTESIAN_POINT ( 'NONE',  ( -109.6203743360497214, -25.27682868748497569, 5.518883987748085751 ) ) ;
#54318 = EDGE_CURVE ( 'NONE', #50083, #27752, #97774, .T. ) ;
#54319 = CARTESIAN_POINT ( 'NONE',  ( -95.52214753415771042, -23.48786465467241058, 11.44779295918254469 ) ) ;
#54320 = VERTEX_POINT ( 'NONE', #187 ) ;
#54321 = CARTESIAN_POINT ( 'NONE',  ( -49.31664351742390551, -25.23350000577289620, 6.415014328141102062 ) ) ;
#54322 = ORIENTED_EDGE ( 'NONE', *, *, #41188, .T. ) ;
#54323 = CARTESIAN_POINT ( 'NONE',  ( -76.62287095715007013, -29.50250243563736774, 8.947779886222141599 ) ) ;
#54324 = CARTESIAN_POINT ( 'NONE',  ( -116.5228709571500616, -23.47596703998600631, 11.44779298504227860 ) ) ;
#54325 = CARTESIAN_POINT ( 'NONE',  ( -6.767879454864726974, -19.68250801024624508, -1.500000000000002220 ) ) ;
#54327 = ADVANCED_FACE ( 'NONE', ( #15402 ), #46362, .T. ) ;
#54326 = CARTESIAN_POINT ( 'NONE',  ( 20.45693200876408469, 7.529271608661172621, 11.49999999999999645 ) ) ;
#54328 = PLANE ( 'NONE',  #43139 ) ;
#54329 = CARTESIAN_POINT ( 'NONE',  ( -78.63378921853097836, -24.15620529776628445, 10.23563542870660292 ) ) ;
#54330 = CARTESIAN_POINT ( 'NONE',  ( -21.13723655771239152, -7.639886366525781014, -1.500000000000002220 ) ) ;
#54331 = CARTESIAN_POINT ( 'NONE',  ( -38.65668546529683880, -23.73766607897670511, -1.055555164236442689 ) ) ;
#54332 = FACE_OUTER_BOUND ( 'NONE', #87742, .T. ) ;
#54333 = CARTESIAN_POINT ( 'NONE',  ( 4.585161930874343206, -5.876774720514427841, 21.47592444013076118 ) ) ;
#54334 = VECTOR ( 'NONE', #40667, 1000.000000000000000 ) ;
#54335 = VERTEX_POINT ( 'NONE', #31129 ) ;
#54336 = ORIENTED_EDGE ( 'NONE', *, *, #60037, .T. ) ;
#54337 = B_SPLINE_CURVE_WITH_KNOTS ( 'NONE', 3,
 ( #2123, #57416, #56914, #66036, #26454, #40676 ),
 .UNSPECIFIED., .F., .F.,
 ( 4, 2, 4 ),
 ( 0.000000000000000000, 0.001380901958385388545, 0.002761803916770777089 ),
 .UNSPECIFIED. ) ;
#54338 = APPROVAL ( #3977, 'UNKNOWN' ) ;
#54339 = EDGE_LOOP ( 'NONE', ( #58395, #25846, #55809, #23395 ) ) ;
#54340 = CARTESIAN_POINT ( 'NONE',  ( -1.376967878889499897, 21.29249089469206524, -1.500000000000002220 ) ) ;
#54341 = VERTEX_POINT ( 'NONE', #43010 ) ;
#54342 = CARTESIAN_POINT ( 'NONE',  ( -13.78326148797977169, 15.88460234914768421, 11.49999999999998934 ) ) ;
#54343 = CARTESIAN_POINT ( 'NONE',  ( -30.60821039366259200, -24.48911842944947992, 0.5642940035406466270 ) ) ;
#54344 = CARTESIAN_POINT ( 'NONE',  ( -111.0291780393114323, -25.22779283739988188, 3.542651572262693005 ) ) ;
#54345 = FACE_OUTER_BOUND ( 'NONE', #84004, .T. ) ;
#54346 = CARTESIAN_POINT ( 'NONE',  ( -1.948345350117603125, -21.87844622001750139, -1.500000000000002220 ) ) ;
#54347 = CARTESIAN_POINT ( 'NONE',  ( -0.1490770655183830395, -21.12008023607310037, -1.443836447538997536 ) ) ;
#54348 = ORIENTED_EDGE ( 'NONE', *, *, #97795, .F. ) ;
#54349 = PLANE ( 'NONE',  #54906 ) ;
#54350 = CARTESIAN_POINT ( 'NONE',  ( -121.5228709571500616, -24.64898659630529565, 1.056161002820833028 ) ) ;
#54351 = CARTESIAN_POINT ( 'NONE',  ( 0.5783248939474509021, 20.82821387695577187, 11.49999999999999645 ) ) ;
#54352 = CARTESIAN_POINT ( 'NONE',  ( 9.278253834636473130, -5.876774720514426953, 18.21871304725684482 ) ) ;
#54353 = FACE_OUTER_BOUND ( 'NONE', #84356, .T. ) ;
#54354 = CARTESIAN_POINT ( 'NONE',  ( -0.1051205485391842609, -21.68913189117569473, 10.47594215909544779 ) ) ;
#54355 = CARTESIAN_POINT ( 'NONE',  ( 17.02398533174402218, 12.79255474601471043, 11.49999999999998934 ) ) ;
#54356 = CARTESIAN_POINT ( 'NONE',  ( -29.49875734969026198, -5.965225279485572685, 7.870022800118625206 ) ) ;
#54357 = CARTESIAN_POINT ( 'NONE',  ( -107.5875550465913904, -24.51419770103157703, 9.386484678747169852 ) ) ;
#54358 = AXIS2_PLACEMENT_3D ( 'NONE', #26457, #49304, #4117 ) ;
#54359 = CARTESIAN_POINT ( 'NONE',  ( 15.97264540888995299, -3.316774720514426456, -27.93485543958162864 ) ) ;
#54360 = CARTESIAN_POINT ( 'NONE',  ( -5.486124437288584232, -5.876774720514417183, 19.74568812963598319 ) ) ;
#54361 = CARTESIAN_POINT ( 'NONE',  ( -22.50818191331092777, 0.9639279967183422837, -1.500000000000002220 ) ) ;
#54362 = AXIS2_PLACEMENT_3D ( 'NONE', #64177, #23569, #55046 ) ;
#54363 = DIRECTION ( 'NONE',  ( 1.000000000000000000, -0.000000000000000000, 0.000000000000000000 ) ) ;
#54364 = ORIENTED_EDGE ( 'NONE', *, *, #44609, .T. ) ;
#54365 = DIRECTION ( 'NONE',  ( 0.7512896232465892110, -0.000000000000000000, 0.6599726524652352877 ) ) ;
#54366 = CARTESIAN_POINT ( 'NONE',  ( -11.77723790057865116, -15.68276428244051779, 11.49999999999999645 ) ) ;
#54367 = DIRECTION ( 'NONE',  ( -1.000000000000000000, 0.000000000000000000, 1.257682986112628908E-16 ) ) ;
#54368 = DIRECTION ( 'NONE',  ( 0.000000000000000000, -1.000000000000000000, 0.000000000000000000 ) ) ;
#54369 = ORIENTED_EDGE ( 'NONE', *, *, #87417, .F. ) ;
#54370 = VECTOR ( 'NONE', #65216, 1000.000000000000114 ) ;
#54371 = CARTESIAN_POINT ( 'NONE',  ( -99.59916881451887605, -23.48783264082478439, -1.443836473390062825 ) ) ;
#54372 = DIRECTION ( 'NONE',  ( 3.773278334444166432E-23, -1.000000000000000000, 0.000000000000000000 ) ) ;
#54373 = FACE_BOUND ( 'NONE', #50362, .T. ) ;
#54374 = CIRCLE ( 'NONE', #51187, 1.149999999999999911 ) ;
#54375 = CARTESIAN_POINT ( 'NONE',  ( 9.261118129494249729, -17.44851725036260248, 11.49999999999998934 ) ) ;
#54376 = VERTEX_POINT ( 'NONE', #43993 ) ;
#54377 = EDGE_CURVE ( 'NONE', #20176, #43203, #17076, .T. ) ;
#54378 = CARTESIAN_POINT ( 'NONE',  ( 8.817327481837082814, 3.316774720514257702, -28.08864864913269699 ) ) ;
#54379 = ADVANCED_FACE ( 'NONE', ( #62103 ), #23501, .F. ) ;
#54380 = DATE_AND_TIME ( #23394, #23091 ) ;
#54381 = EDGE_LOOP ( 'NONE', ( #95353, #72444, #67566, #46429 ) ) ;
#54382 = DIRECTION ( 'NONE',  ( -0.7512896232465891000, 0.000000000000000000, -0.6599726524652351767 ) ) ;
#54383 = DIRECTION ( 'NONE',  ( 0.000000000000000000, 0.000000000000000000, -1.000000000000000000 ) ) ;
#54384 = CARTESIAN_POINT ( 'NONE',  ( -55.58286566446923871, -24.73486907724917572, 1.287355809206962798 ) ) ;
#54385 = DIRECTION ( 'NONE',  ( 0.000000000000000000, 0.000000000000000000, -1.000000000000000000 ) ) ;
#54386 = CARTESIAN_POINT ( 'NONE',  ( -85.55620429048339304, -23.48783264082478084, -1.443836473390063269 ) ) ;
#54387 = CARTESIAN_POINT ( 'NONE',  ( -44.58953762381673158, -24.64965694238406613, 8.947790433994660120 ) ) ;
#54388 = CARTESIAN_POINT ( 'NONE',  ( -29.96442075442584851, -23.42317284524191123, -1.443836447538997314 ) ) ;
#54389 = CARTESIAN_POINT ( 'NONE',  ( 19.86090765050778728, -2.328952942160339212, 11.49999999999998934 ) ) ;
#54390 = ADVANCED_FACE ( 'NONE', ( #90666 ), #52114, .F. ) ;
#54391 = FACE_OUTER_BOUND ( 'NONE', #53773, .T. ) ;
#54392 = CARTESIAN_POINT ( 'NONE',  ( -45.63589775446569519, -24.63419186844611986, 9.035850630976927533 ) ) ;
#54393 = VERTEX_POINT ( 'NONE', #35400 ) ;
#54394 = PLANE ( 'NONE',  #71292 ) ;
#54395 = CIRCLE ( 'NONE', #52733, 2.000000000000000000 ) ;
#54396 = PLANE ( 'NONE',  #7078 ) ;
#54397 = CARTESIAN_POINT ( 'NONE',  ( -35.50852639300465086, -23.85016227208580730, -0.8807180028928170978 ) ) ;
#54398 = CARTESIAN_POINT ( 'NONE',  ( -100.5228709571500758, -24.52323809116981934, 9.355190652339423707 ) ) ;
#54399 = CARTESIAN_POINT ( 'NONE',  ( -118.8949105597723843, -25.34741607406076724, 3.801658267186116547 ) ) ;
#54400 = DIRECTION ( 'NONE',  ( -0.000000000000000000, 2.173523156925979552E-06, -0.9999999999976378895 ) ) ;
#54401 = DIRECTION ( 'NONE',  ( -1.000000000000000000, -3.773278334444166432E-23, -8.201307841325785021E-29 ) ) ;
#54402 = DIRECTION ( 'NONE',  ( 0.000000000000000000, 0.000000000000000000, 1.000000000000000000 ) ) ;
#54403 = ORIENTED_EDGE ( 'NONE', *, *, #25593, .T. ) ;
#54404 = CARTESIAN_POINT ( 'NONE',  ( 20.05935882324986963, -3.104462954613115500, -1.500000000000002220 ) ) ;
#54405 = DIRECTION ( 'NONE',  ( 0.000000000000000000, 0.000000000000000000, -1.000000000000000000 ) ) ;
#54406 = CARTESIAN_POINT ( 'NONE',  ( -82.52287095715006160, -29.50250243563736774, 8.947779886222141599 ) ) ;
#54407 = EDGE_LOOP ( 'NONE', ( #67150, #66062, #47705, #25058 ) ) ;
#54409 = ADVANCED_FACE ( 'NONE', ( #76789 ), #27773, .T. ) ;
#54408 = CARTESIAN_POINT ( 'NONE',  ( -81.62287095715005592, -24.65952944569304606, 1.056160979905699460 ) ) ;
#54410 = CARTESIAN_POINT ( 'NONE',  ( 13.72940079880349984, -14.68433028913016791, -1.500000000000002220 ) ) ;
#54411 = CARTESIAN_POINT ( 'NONE',  ( -20.97943885474387216, 2.004451313549292735, 11.49999999999999645 ) ) ;
#54412 = CARTESIAN_POINT ( 'NONE',  ( 22.05266032001784637, -1.487345182339283367, 11.49999999999998934 ) ) ;
#54413 = EDGE_CURVE ( 'NONE', #13115, #84470, #70275, .T. ) ;
#54414 = CARTESIAN_POINT ( 'NONE',  ( -16.44861368136865920, 12.28130381464353782, -1.500000000000002220 ) ) ;
#54415 = VECTOR ( 'NONE', #95855, 1000.000000000000000 ) ;
#54416 = CARTESIAN_POINT ( 'NONE',  ( -60.54477366480123379, -24.40034930558990922, 0.3402023900116026289 ) ) ;
#54417 = EDGE_LOOP ( 'NONE', ( #22471, #35589, #96005, #21719, #75114, #54528, #65589, #24917, #30217 ) ) ;
#54418 = CARTESIAN_POINT ( 'NONE',  ( -32.62287095715004881, -24.64898659630367206, 1.056161002820817485 ) ) ;
#54419 = ORIENTED_EDGE ( 'NONE', *, *, #90877, .T. ) ;
#54420 = DIRECTION ( 'NONE',  ( -8.334928612639484546E-17, 1.000000000000000000, -7.321843366904296032E-17 ) ) ;
#54421 = CARTESIAN_POINT ( 'NONE',  ( 6.573941812937369455, 1.185825954564562440E-17, -0.2639660507643281639 ) ) ;
#54422 = ORIENTED_EDGE ( 'NONE', *, *, #70611, .T. ) ;
#54423 = VECTOR ( 'NONE', #75908, 1000.000000000000114 ) ;
#54424 = ORIENTED_EDGE ( 'NONE', *, *, #7604, .F. ) ;
#54425 = CIRCLE ( 'NONE', #91717, 1.306876713926001354 ) ;
#54426 = ORIENTED_EDGE ( 'NONE', *, *, #2502, .T. ) ;
#54427 = CARTESIAN_POINT ( 'NONE',  ( -116.9228709571500389, -23.47593901973090169, -1.443836447538996648 ) ) ;
#54428 = CARTESIAN_POINT ( 'NONE',  ( -74.62287095715004170, -24.66019654487199375, 8.947790411086129936 ) ) ;
#54429 = CARTESIAN_POINT ( 'NONE',  ( -68.52210146834674731, -23.48786465467241058, 11.44779295918254824 ) ) ;
#54430 = CARTESIAN_POINT ( 'NONE',  ( -18.82610421443283499, -8.410905081555696938, -1.500000000000002220 ) ) ;
#54431 = AXIS2_PLACEMENT_3D ( 'NONE', #70203, #8300, #86425 ) ;
#54432 = CARTESIAN_POINT ( 'NONE',  ( -8.642975711230413083, 19.83371042614930957, 11.49999999999999645 ) ) ;
#54433 = ORIENTED_EDGE ( 'NONE', *, *, #44990, .F. ) ;
#54434 = CARTESIAN_POINT ( 'NONE',  ( -0.4909855769230799249, -5.876774720514410077, 19.14743589743590491 ) ) ;
#54435 = CARTESIAN_POINT ( 'NONE',  ( 6.184520403203634942, 6.376774720514426953, -25.32021290018218451 ) ) ;
#54436 = CARTESIAN_POINT ( 'NONE',  ( -20.28323820415832657, -9.445149539555593776, -1.500000000000002220 ) ) ;
#54437 = VECTOR ( 'NONE', #73005, 1000.000000000000114 ) ;
#54438 = CARTESIAN_POINT ( 'NONE',  ( -71.52287095715006160, -24.34917612406836795, 0.1852690917426534634 ) ) ;
#54439 = LINE ( 'NONE', #23455, #96721 ) ;
#54440 = VERTEX_POINT ( 'NONE', #58723 ) ;
#54441 = CARTESIAN_POINT ( 'NONE',  ( -117.0507892446735525, -25.34772161262076295, 6.200219024653767619 ) ) ;
#54442 = DIRECTION ( 'NONE',  ( 0.000000000000000000, -1.000000000000000000, 0.000000000000000000 ) ) ;
#54443 = CARTESIAN_POINT ( 'NONE',  ( 4.013313563623547964, -20.52093592976233438, -1.500000000000002220 ) ) ;
#54444 = VERTEX_POINT ( 'NONE', #51115 ) ;
#54445 = EDGE_CURVE ( 'NONE', #96748, #73913, #35250, .T. ) ;
#54446 = DIRECTION ( 'NONE',  ( -1.000000000000000000, 0.000000000000000000, 0.000000000000000000 ) ) ;
#54447 = ORIENTED_EDGE ( 'NONE', *, *, #4292, .F. ) ;
#54448 = DIRECTION ( 'NONE',  ( 5.328431011793917330E-15, 0.000000000000000000, 1.000000000000000000 ) ) ;
#54449 = CARTESIAN_POINT ( 'NONE',  ( -6.202713861520617655, -20.23501359363181962, -1.500000000000002220 ) ) ;
#54450 = ORIENTED_EDGE ( 'NONE', *, *, #71542, .F. ) ;
#54451 = CARTESIAN_POINT ( 'NONE',  ( -50.58555295165667332, -24.63355581998386157, 0.9682620441943928791 ) ) ;
#54452 = CARTESIAN_POINT ( 'NONE',  ( -9.857415191643349672, 19.42730305858377449, -1.500000000000002220 ) ) ;
#54453 = CARTESIAN_POINT ( 'NONE',  ( -121.5228709571500616, -23.48786465467241769, 11.44779295918253759 ) ) ;
#54454 = CARTESIAN_POINT ( 'NONE',  ( -41.52287095715006870, -23.47593901973090169, -1.443836447538997092 ) ) ;
#54455 = CARTESIAN_POINT ( 'NONE',  ( -35.52287095715008292, -24.82576562948883137, 8.398263436605599708 ) ) ;
#54456 = CARTESIAN_POINT ( 'NONE',  ( 18.19902423439809525, 11.99547645517801442, -1.500000000000002220 ) ) ;
#54457 = CARTESIAN_POINT ( 'NONE',  ( -30.57287095715006586, -24.75921641729242495, 8.610803353223845491 ) ) ;
#54458 = ORIENTED_EDGE ( 'NONE', *, *, #93418, .F. ) ;
#54459 = B_SPLINE_CURVE_WITH_KNOTS ( 'NONE', 3,
 ( #90306, #21771, #13663, #29399 ),
 .UNSPECIFIED., .F., .F.,
 ( 4, 4 ),
 ( 0.000000000000000000, 9.999999999997510880E-05 ),
 .UNSPECIFIED. ) ;
#54460 = CARTESIAN_POINT ( 'NONE',  ( 7.311104923646705167, -5.876774720514416295, 20.13320233724603980 ) ) ;
#54461 = CARTESIAN_POINT ( 'NONE',  ( -117.5228709571500616, -24.50216790748203977, 0.6166512839542631630 ) ) ;
#54462 = VERTEX_POINT ( 'NONE', #2704 ) ;
#54463 = ADVANCED_FACE ( 'NONE', ( #26025 ), #85928, .F. ) ;
#54464 = ORIENTED_EDGE ( 'NONE', *, *, #26253, .T. ) ;
#54465 = ORIENTED_EDGE ( 'NONE', *, *, #2514, .T. ) ;
#54466 = B_SPLINE_CURVE_WITH_KNOTS ( 'NONE', 3,
 ( #1741, #93566, #39789, #48422, #33181, #86965, #94581, #95582 ),
 .UNSPECIFIED., .F., .F.,
 ( 4, 2, 2, 4 ),
 ( 6.391158118975187985E-06, 0.002007136338672934825, 0.003007508928949912536, 0.004007881519226890246 ),
 .UNSPECIFIED. ) ;
#54467 = CARTESIAN_POINT ( 'NONE',  ( -70.32380231474228083, -25.13313949306887096, 7.101635536975467566 ) ) ;
#54468 = DIRECTION ( 'NONE',  ( 0.000000000000000000, -1.000000000000000000, 0.000000000000000000 ) ) ;
#54469 = CARTESIAN_POINT ( 'NONE',  ( 0.06830352742921809439, -21.21198074455918814, -1.500000000000002220 ) ) ;
#54470 = CARTESIAN_POINT ( 'NONE',  ( -52.62287095715005592, -24.66019654487199020, 8.947790411086135265 ) ) ;
#54471 = CARTESIAN_POINT ( 'NONE',  ( -80.18401481691103072, -25.27791967176670340, 7.536602771734753681 ) ) ;
#54472 = FACE_OUTER_BOUND ( 'NONE', #62301, .T. ) ;
#54473 = CARTESIAN_POINT ( 'NONE',  ( -48.52287095715006160, -23.47596703998600631, 11.44779298504229104 ) ) ;
#54474 = CARTESIAN_POINT ( 'NONE',  ( 14.41255161864883583, -12.98630880007775268, 11.49999999999998934 ) ) ;
#54475 = CARTESIAN_POINT ( 'NONE',  ( -41.88654540179980756, -25.30060000302003687, 6.009290021095885059 ) ) ;
#54476 = ORIENTED_EDGE ( 'NONE', *, *, #68022, .T. ) ;
#54477 = CARTESIAN_POINT ( 'NONE',  ( 1.255614643274026276, -19.41590359075080841, 11.49999999999999645 ) ) ;
#54478 = CYLINDRICAL_SURFACE ( 'NONE', #3367, 1.050000000000000488 ) ;
#54479 = EDGE_CURVE ( 'NONE', #35375, #32600, #40257, .T. ) ;
#54480 = CARTESIAN_POINT ( 'NONE',  ( 13.10664265030973930, -5.965225279485574461, -27.62597719988137612 ) ) ;
#54481 = EDGE_LOOP ( 'NONE', ( #48839, #100366, #95048, #76676 ) ) ;
#54482 = CARTESIAN_POINT ( 'NONE',  ( 3.552794897967157528, -6.376774720514401196, 18.18650940196788568 ) ) ;
#54483 = CARTESIAN_POINT ( 'NONE',  ( -97.52287095715010423, -23.48783264082477018, -1.443836473390087027 ) ) ;
#54484 = CARTESIAN_POINT ( 'NONE',  ( -64.62287095715009855, -24.33832256527048088, 0.1851278514138592346 ) ) ;
#54485 = DIRECTION ( 'NONE',  ( -0.000000000000000000, 0.000000000000000000, -1.000000000000000000 ) ) ;
#54486 = CARTESIAN_POINT ( 'NONE',  ( 19.59260286812380514, -1.442238090573773501, -1.500000000000002220 ) ) ;
#54487 = LINE ( 'NONE', #69718, #46149 ) ;
#54488 = EDGE_LOOP ( 'NONE', ( #31517, #62549 ) ) ;
#54489 = CARTESIAN_POINT ( 'NONE',  ( -16.60028029328060128, 13.79055755010687356, -1.500000000000002220 ) ) ;
#54490 = CARTESIAN_POINT ( 'NONE',  ( -40.53727650475425293, -24.52300882791530157, 0.6510814631126360386 ) ) ;
#54491 = DIRECTION ( 'NONE',  ( 0.000000000000000000, -1.000000000000000000, 0.000000000000000000 ) ) ;
#54492 = CARTESIAN_POINT ( 'NONE',  ( -19.18584950847915493, -12.73052202388904952, -1.500000000000002220 ) ) ;
#54493 = ADVANCED_FACE ( 'NONE', ( #54984 ), #56500, .T. ) ;
#54494 = AXIS2_PLACEMENT_3D ( 'NONE', #86719, #79103, #79607 ) ;
#54495 = B_SPLINE_CURVE_WITH_KNOTS ( 'NONE', 3,
 ( #10038, #40998, #71955, #87669, #18149, #13893 ),
 .UNSPECIFIED., .F., .F.,
 ( 4, 2, 4 ),
 ( 1.570887131794795405E-05, 0.001396322306279765193, 0.002776935741241582344 ),
 .UNSPECIFIED. ) ;
#54496 = PERSON_AND_ORGANIZATION ( #70597, #27821 ) ;
#54497 = CARTESIAN_POINT ( 'NONE',  ( -93.58859060503255023, -24.34968618360934300, 0.1864209137778838898 ) ) ;
#54498 = CARTESIAN_POINT ( 'NONE',  ( -90.52287095715006160, -24.99156044556202616, 7.747789690856173195 ) ) ;
#54499 = CARTESIAN_POINT ( 'NONE',  ( -121.6259261874522934, -23.96169478059713498, 10.65365249895717525 ) ) ;
#54500 = FACE_OUTER_BOUND ( 'NONE', #83603, .T. ) ;
#54501 = VECTOR ( 'NONE', #20828, 1000.000000000000227 ) ;
#54503 = CARTESIAN_POINT ( 'NONE',  ( -111.5321115232925564, -25.29823951520918612, 3.478177323284377120 ) ) ;
#54502 = VECTOR ( 'NONE', #99853, 1000.000000000000000 ) ;
#54504 = CARTESIAN_POINT ( 'NONE',  ( -129.5559603475894903, -23.96119346886880663, -0.6495511937831975890 ) ) ;
#54505 = CARTESIAN_POINT ( 'NONE',  ( -114.6278463927332893, -23.96169478059714208, 10.65365249895717170 ) ) ;
#54506 = CARTESIAN_POINT ( 'NONE',  ( 19.87125486832220744, 0.9792442318621276121, -1.500000000000002220 ) ) ;
#54507 = ADVANCED_FACE ( 'NONE', ( #48879 ), #77790, .T. ) ;
#54508 = CARTESIAN_POINT ( 'NONE',  ( -79.11611000704996854, -25.14083923594767001, 2.947789366383933185 ) ) ;
#54509 = CARTESIAN_POINT ( 'NONE',  ( -2.602694502683683631, -19.63732897141692391, -1.500000000000002220 ) ) ;
#54510 = VECTOR ( 'NONE', #44929, 1000.000000000000114 ) ;
#54511 = CARTESIAN_POINT ( 'NONE',  ( 0.3910256410256418569, -5.876774720514419847, 20.67377804487180271 ) ) ;
#54512 = EDGE_CURVE ( 'NONE', #49424, #52090, #7412, .T. ) ;
#54513 = DIRECTION ( 'NONE',  ( 0.7512896232465892110, -0.000000000000000000, 0.6599726524652351767 ) ) ;
#54514 = CARTESIAN_POINT ( 'NONE',  ( -94.62287095715005592, -23.47593901973091235, -1.443836447539002865 ) ) ;
#54515 = CARTESIAN_POINT ( 'NONE',  ( 20.29938135082171158, -4.300543036493735372, 11.49999999999999645 ) ) ;
#54516 = CARTESIAN_POINT ( 'NONE',  ( -7.641025641025641413, -6.376774720514418959, 20.36458333333334636 ) ) ;
#54517 = B_SPLINE_CURVE_WITH_KNOTS ( 'NONE', 3,
 ( #77193, #8711, #91933, #92429, #22896, #7699, #53388, #45765, #47273, #84317, #91, #86328, #15806, #69608, #23400 ),
 .UNSPECIFIED., .F., .F.,
 ( 4, 1, 1, 1, 1, 1, 1, 1, 1, 1, 1, 1, 4 ),
 ( 0.000000000000000000, 0.07176606415833945707, 0.1412255357663688426, 0.2091158524974623678, 0.2748396534685264014, 0.3394829303752206484, 0.4024762667353993240, 0.4649418891713267277, 0.5268326406463827993, 0.6474148160608228508, 0.7655615117859491114, 0.8816150870393308914, 1.000000000000000000 ),
 .UNSPECIFIED. ) ;
#54518 = CARTESIAN_POINT ( 'NONE',  ( -106.5515625499468371, -24.34968618360934300, 0.1864209137778878034 ) ) ;
#54519 = CARTESIAN_POINT ( 'NONE',  ( -22.16177213047534877, -5.259615592301647879, 11.49999999999999645 ) ) ;
#54520 = ORIENTED_EDGE ( 'NONE', *, *, #21002, .F. ) ;
#54521 = CARTESIAN_POINT ( 'NONE',  ( -69.63097038022910112, -24.34968618360933945, 0.1864209137778826408 ) ) ;
#54522 = CARTESIAN_POINT ( 'NONE',  ( -69.39531695424813051, -25.21178052097284450, 6.510839736813604617 ) ) ;
#54523 = ORIENTED_EDGE ( 'NONE', *, *, #12664, .F. ) ;
#54524 = CARTESIAN_POINT ( 'NONE',  ( -19.56588111578679090, -4.897929960003377658, -1.500000000000002220 ) ) ;
#54525 = DIRECTION ( 'NONE',  ( -2.352173255807796056E-16, 0.000000000000000000, 1.000000000000000000 ) ) ;
#54526 = CARTESIAN_POINT ( 'NONE',  ( -97.62287095715008434, -23.47596703998600631, 11.44779298504227860 ) ) ;
#54527 = EDGE_LOOP ( 'NONE', ( #100097, #48466, #42046, #5800 ) ) ;
#54528 = ORIENTED_EDGE ( 'NONE', *, *, #98736, .F. ) ;
#54529 = CARTESIAN_POINT ( 'NONE',  ( -0.1037292527911751056, -6.376774720514413630, 19.53657742262743824 ) ) ;
#54530 = CARTESIAN_POINT ( 'NONE',  ( 12.66508800429495629, 19.07499079241581086, -1.500000000000002220 ) ) ;
#54531 = CARTESIAN_POINT ( 'NONE',  ( -51.10270014058699672, -25.18439706043954018, 3.552654129014596762 ) ) ;
#54532 = CARTESIAN_POINT ( 'NONE',  ( -9.004746288917990782, -19.65190454534591069, -1.500000000000002220 ) ) ;
#54533 = DIRECTION ( 'NONE',  ( -1.000000000000000000, -0.000000000000000000, -0.000000000000000000 ) ) ;
#54534 = CARTESIAN_POINT ( 'NONE',  ( -13.97254113366623152, 15.51630364309664856, 11.49999999999999645 ) ) ;
#54535 = ORIENTED_EDGE ( 'NONE', *, *, #50484, .T. ) ;
#54536 = DIRECTION ( 'NONE',  ( 0.000000000000000000, 0.000000000000000000, -1.000000000000000000 ) ) ;
#54537 = CARTESIAN_POINT ( 'NONE',  ( -21.12052157030387889, 6.262089831203976331, -1.500000000000002220 ) ) ;
#54538 = CARTESIAN_POINT ( 'NONE',  ( -4.141025641025641413, -5.876774720514419847, 20.67377804487180271 ) ) ;
#54539 = CARTESIAN_POINT ( 'NONE',  ( -66.58953762381672448, -24.64965694238406968, 8.947790433994660120 ) ) ;
#54541 = VERTEX_POINT ( 'NONE', #71208 ) ;
#54540 = EDGE_CURVE ( 'NONE', #19866, #93563, #79305, .T. ) ;
#54542 = CARTESIAN_POINT ( 'NONE',  ( -12.84880425037203011, -5.965225279485592225, -26.59900746623528534 ) ) ;
#54543 = PLANE ( 'NONE',  #28426 ) ;
#54544 = ORIENTED_EDGE ( 'NONE', *, *, #80729, .F. ) ;
#54545 = DIRECTION ( 'NONE',  ( -0.000000000000000000, -1.000000000000000000, -0.000000000000000000 ) ) ;
#54546 = ORIENTED_EDGE ( 'NONE', *, *, #80065, .T. ) ;
#54547 = VERTEX_POINT ( 'NONE', #1702 ) ;
#54548 = CARTESIAN_POINT ( 'NONE',  ( -71.56491059194962645, -23.48786465467241058, 11.44779295918254824 ) ) ;
#54549 = LINE ( 'NONE', #7362, #68080 ) ;
#54550 = CARTESIAN_POINT ( 'NONE',  ( -4.213970605900704491, -5.876774720514415407, 20.02963804100705758 ) ) ;
#54551 = CARTESIAN_POINT ( 'NONE',  ( 20.41236503877875563, 1.188189311754236144, -1.500000000000002220 ) ) ;
#54552 = VERTEX_POINT ( 'NONE', #25018 ) ;
#54553 = CARTESIAN_POINT ( 'NONE',  ( -79.52287095715009002, -24.33832256527049154, 0.1851278514138619824 ) ) ;
#54554 = CARTESIAN_POINT ( 'NONE',  ( -44.62858516920130114, -24.51314013834316086, 0.6176544820404110681 ) ) ;
#54555 = DIRECTION ( 'NONE',  ( -0.06486421869277853025, 0.000000000000000000, 0.9978940991575085961 ) ) ;
#54556 = CARTESIAN_POINT ( 'NONE',  ( -13.27262489239681997, 17.90159134968837051, 11.49999999999998934 ) ) ;
#54557 = CIRCLE ( 'NONE', #10809, 251.4258649670780699 ) ;
#54558 = CARTESIAN_POINT ( 'NONE',  ( -90.55620429048339304, -23.47593901973091235, -1.443836447539002865 ) ) ;
#54559 = CARTESIAN_POINT ( 'NONE',  ( -1.568769572606061535, -5.876774720514415407, 19.76359802465961835 ) ) ;
#54560 = ORIENTED_EDGE ( 'NONE', *, *, #26105, .T. ) ;
#54561 = CARTESIAN_POINT ( 'NONE',  ( 0.000000000000000000, -4.056774720514426669, 0.000000000000000000 ) ) ;
#54562 = CARTESIAN_POINT ( 'NONE',  ( -29.81175120719462157, -24.63645345484493632, 4.942812314408664420 ) ) ;
#54563 = CARTESIAN_POINT ( 'NONE',  ( -5.744250498300313090, 20.02623800365557472, -1.500000000000002220 ) ) ;
#54564 = ORIENTED_EDGE ( 'NONE', *, *, #90843, .F. ) ;
#54566 = EDGE_LOOP ( 'NONE', ( #58078, #22697, #93848 ) ) ;
#54565 = CARTESIAN_POINT ( 'NONE',  ( 5.550000000000006040, -14.50000000000000178, 11.24599928863593767 ) ) ;
#54567 = VECTOR ( 'NONE', #94925, 1000.000000000000000 ) ;
#54568 = EDGE_CURVE ( 'NONE', #62223, #20563, #32635, .T. ) ;
#54569 = EDGE_LOOP ( 'NONE', ( #11501, #59815, #28161, #84846 ) ) ;
#54570 = CARTESIAN_POINT ( 'NONE',  ( -51.11259392460791418, -25.12217823885073997, 6.923368740699049617 ) ) ;
#54571 = CARTESIAN_POINT ( 'NONE',  ( 20.78037738254806399, 3.014218216234254566, -1.500000000000002220 ) ) ;
#54572 = EDGE_CURVE ( 'NONE', #71695, #9907, #56996, .T. ) ;
#54573 = VERTEX_POINT ( 'NONE', #95037 ) ;
#54574 = AXIS2_PLACEMENT_3D ( 'NONE', #1656, #86879, #84875 ) ;
#54575 = CARTESIAN_POINT ( 'NONE',  ( 282.9764569301858046, 5.965225279485572685, 20.79159422840526616 ) ) ;
#54576 = DIRECTION ( 'NONE',  ( -0.000000000000000000, 2.173523156925979552E-06, -0.9999999999976378895 ) ) ;
#54577 = CARTESIAN_POINT ( 'NONE',  ( 9.214646252596866205, -5.356774720515496746, -27.04520690447069597 ) ) ;
#54578 = AXIS2_PLACEMENT_3D ( 'NONE', #7891, #38843, #71305 ) ;
#54579 = DIRECTION ( 'NONE',  ( -0.000000000000000000, -1.000000000000000000, -0.000000000000000000 ) ) ;
#54580 = CARTESIAN_POINT ( 'NONE',  ( -92.62572372221266903, -24.51419770103156281, 9.386484678747175181 ) ) ;
#54581 = LINE ( 'NONE', #47972, #33492 ) ;
#54583 = ORIENTED_EDGE ( 'NONE', *, *, #24326, .T. ) ;
#54582 = CARTESIAN_POINT ( 'NONE',  ( -9.187330254778467875, -20.22999604658808082, 11.49999999999999645 ) ) ;
#54584 = PLANE ( 'NONE',  #24274 ) ;
#54585 = CARTESIAN_POINT ( 'NONE',  ( -93.62287095715005592, -24.64965695001468404, 8.947790433994180503 ) ) ;
#54586 = ORIENTED_EDGE ( 'NONE', *, *, #58858, .F. ) ;
#54587 = CARTESIAN_POINT ( 'NONE',  ( -0.4833002549469566644, -22.66139224067150337, 11.49999999999998934 ) ) ;
#54588 = EDGE_CURVE ( 'NONE', #5782, #94189, #8804, .T. ) ;
#54589 = VECTOR ( 'NONE', #8959, 1000.000000000000227 ) ;
#54590 = EDGE_CURVE ( 'NONE', #77509, #26860, #87346, .T. ) ;
#54592 = ORIENTED_EDGE ( 'NONE', *, *, #1703, .T. ) ;
#54591 = CARTESIAN_POINT ( 'NONE',  ( -111.5228709571500616, -24.35013146730204525, 9.818937971375092388 ) ) ;
#54593 = ORIENTED_EDGE ( 'NONE', *, *, #91820, .T. ) ;
#54594 = ADVANCED_FACE ( 'NONE', ( #31631 ), #40752, .F. ) ;
#54595 = CARTESIAN_POINT ( 'NONE',  ( 14.76093561896379214, -3.316774720514426456, -26.55548769130089681 ) ) ;
#54596 = CARTESIAN_POINT ( 'NONE',  ( 14.76687977769557847, -13.71354340032049457, -1.500000000000002220 ) ) ;
#54597 = CARTESIAN_POINT ( 'NONE',  ( -6.775140224358976226, -5.876774720514409189, 19.14743589743590846 ) ) ;
#54598 = ORIENTED_EDGE ( 'NONE', *, *, #73938, .T. ) ;
#54599 = DIRECTION ( 'NONE',  ( 3.773278334444167608E-23, -1.000000000000000000, 0.000000000000000000 ) ) ;
#54600 = CARTESIAN_POINT ( 'NONE',  ( -12.45998644600372884, -18.51849504856558681, -1.500000000000002220 ) ) ;
#54601 = EDGE_CURVE ( 'NONE', #69272, #98613, #23174, .T. ) ;
#54602 = ORIENTED_EDGE ( 'NONE', *, *, #100148, .F. ) ;
#54603 = ORIENTED_EDGE ( 'NONE', *, *, #65989, .T. ) ;
#54604 = CARTESIAN_POINT ( 'NONE',  ( 22.81105451610979173, -1.475225279485572916, -18.46691820600746681 ) ) ;
#54605 = CARTESIAN_POINT ( 'NONE',  ( -94.50776865740360222, -24.51419770103156281, 9.386484678747184063 ) ) ;
#54606 = CARTESIAN_POINT ( 'NONE',  ( -1.044871794871790938, -5.876774720514426953, 21.75000000000000355 ) ) ;
#54607 = CIRCLE ( 'NONE', #95165, 1.000000000000000444 ) ;
#54608 = DIRECTION ( 'NONE',  ( -3.773278334444166432E-23, 1.000000000000000000, 0.000000000000000000 ) ) ;
#54609 = CARTESIAN_POINT ( 'NONE',  ( 2.000000000000000000, 7.470345474798854293E-16, -6.099999999999999645 ) ) ;
#54610 = CARTESIAN_POINT ( 'NONE',  ( 19.54226456527178257, 0.3027743077981833730, 11.49999999999998934 ) ) ;
#54611 = CARTESIAN_POINT ( 'NONE',  ( -53.01255352321339842, 2.682774720514426559, 35.59556822165056644 ) ) ;
#54612 = CARTESIAN_POINT ( 'NONE',  ( 4.199879391047538491, -21.09745483596041282, 11.49999999999998934 ) ) ;
#54613 = VECTOR ( 'NONE', #32623, 1000.000000000000000 ) ;
#54614 = FACE_OUTER_BOUND ( 'NONE', #7567, .T. ) ;
#54615 = CARTESIAN_POINT ( 'NONE',  ( -50.40445135320380388, -25.18492896333868103, 3.293943116708552221 ) ) ;
#54616 = DIRECTION ( 'NONE',  ( 1.000000000000000000, 3.773278334444166432E-23, 8.201307841325785021E-29 ) ) ;
#54617 = CARTESIAN_POINT ( 'NONE',  ( 32.84232313084847732, -4.840274619473232676, -11.71291885348859196 ) ) ;
#54618 = CARTESIAN_POINT ( 'NONE',  ( -20.40978113611479827, 10.34812579263477872, -1.500000000000002220 ) ) ;
#54619 = EDGE_CURVE ( 'NONE', #50558, #58657, #59505, .T. ) ;
#54620 = B_SPLINE_CURVE_WITH_KNOTS ( 'NONE', 3,
 ( #15648, #70953, #69937, #425 ),
 .UNSPECIFIED., .F., .F.,
 ( 4, 4 ),
 ( 0.000000000000000000, 0.0001000000000000167422 ),
 .UNSPECIFIED. ) ;
#54621 = EDGE_CURVE ( 'NONE', #91381, #77509, #49625, .T. ) ;
#54622 = APPROVAL_ROLE ( '' ) ;
#54623 = DIRECTION ( 'NONE',  ( -0.000000000000000000, 1.000000000000000000, -0.000000000000000000 ) ) ;
#54624 = CARTESIAN_POINT ( 'NONE',  ( -53.56013271601442227, -23.73766607897669800, -1.055555164236460008 ) ) ;
#54625 = CARTESIAN_POINT ( 'NONE',  ( -19.89792590360708147, -2.209704250470923892, 11.49999999999999645 ) ) ;
#54626 = CARTESIAN_POINT ( 'NONE',  ( -78.96619831399281964, -25.26612626921278348, 5.670633042279167313 ) ) ;
#54627 = PLANE ( 'NONE',  #74357 ) ;
#54628 = CARTESIAN_POINT ( 'NONE',  ( -78.52287095715006160, -29.50250243563736774, 8.947779886222141599 ) ) ;
#54629 = LINE ( 'NONE', #79453, #53746 ) ;
#54630 = ORIENTED_EDGE ( 'NONE', *, *, #74495, .F. ) ;
#54631 = CARTESIAN_POINT ( 'NONE',  ( -50.62287095715005592, -24.83620972994591014, 8.398175272781365663 ) ) ;
#54632 = CARTESIAN_POINT ( 'NONE',  ( -115.6228709571500843, -24.92604778743018201, 8.074972756849350120 ) ) ;
#54633 = EDGE_CURVE ( 'NONE', #67086, #90447, #8447, .T. ) ;
#54634 = CARTESIAN_POINT ( 'NONE',  ( 9.899741330608472722, -19.37759744025533593, -1.500000000000002220 ) ) ;
#54635 = CARTESIAN_POINT ( 'NONE',  ( -19.61143073682725202, -1.510137823221562092, -1.500000000000002220 ) ) ;
#54636 = CIRCLE ( 'NONE', #59483, 1.249999999999996003 ) ;
#54637 = PLANE ( 'NONE',  #52377 ) ;
#54638 = EDGE_CURVE ( 'NONE', #37940, #73668, #65618, .T. ) ;
#54639 = EDGE_CURVE ( 'NONE', #35049, #48122, #82308, .T. ) ;
#54640 = DIRECTION ( 'NONE',  ( 1.000000000000000000, 3.773278334444166432E-23, 8.201307841325785021E-29 ) ) ;
#54641 = APPROVAL_DATE_TIME ( #77943, #69216 ) ;
#54642 = LINE ( 'NONE', #39407, #28912 ) ;
#54643 = DIRECTION ( 'NONE',  ( 0.5473879298857849962, 0.000000000000000000, 0.8368789961609472972 ) ) ;
#54644 = CARTESIAN_POINT ( 'NONE',  ( 10.47388184937329214, 17.72644800832989986, 11.49999999999999645 ) ) ;
#54645 = CARTESIAN_POINT ( 'NONE',  ( 30.58729439590577570, 4.540774720514427543, 26.14186284044645703 ) ) ;
#54646 = VECTOR ( 'NONE', #23192, 1000.000000000000000 ) ;
#54647 = CARTESIAN_POINT ( 'NONE',  ( 9.071512145086499501, -0.9000000000000000222, 3.687490859131163923 ) ) ;
#54648 = EDGE_CURVE ( 'NONE', #16838, #95239, #35148, .T. ) ;
#54649 = VERTEX_POINT ( 'NONE', #3702 ) ;
#54650 = CARTESIAN_POINT ( 'NONE',  ( -100.3574794290996266, -25.26387448364017985, 4.711073633588144460 ) ) ;
#54651 = PLANE ( 'NONE',  #55893 ) ;
#54652 = CARTESIAN_POINT ( 'NONE',  ( -108.5562042904834072, -23.48783264082479505, -1.443836473390060160 ) ) ;
#54653 = CARTESIAN_POINT ( 'NONE',  ( 22.02124265030973760, 3.456774720514426136, 15.05402280011862004 ) ) ;
#54654 = VECTOR ( 'NONE', #45228, 1000.000000000000114 ) ;
#54655 = CARTESIAN_POINT ( 'NONE',  ( -33.62287095715005592, -23.72747288104469732, -1.053458166803227680 ) ) ;
#54656 = CARTESIAN_POINT ( 'NONE',  ( -42.62287095715005592, -23.95044443724992078, 10.65354141964649592 ) ) ;
#54657 = B_SPLINE_CURVE_WITH_KNOTS ( 'NONE', 3,
 ( #78756, #23978, #47836, #40220 ),
 .UNSPECIFIED., .F., .F.,
 ( 4, 4 ),
 ( 0.000000000000000000, 9.999999999996123101E-05 ),
 .UNSPECIFIED. ) ;
#54658 = EDGE_LOOP ( 'NONE', ( #60597, #57064, #94059, #74148 ) ) ;
#54659 = CARTESIAN_POINT ( 'NONE',  ( 22.92345266703080142, -2.467471440992916154, 11.49999999999999645 ) ) ;
#54660 = CARTESIAN_POINT ( 'NONE',  ( 17.58993269669914383, -14.52173041563253975, 11.49999999999998934 ) ) ;
#54661 = CARTESIAN_POINT ( 'NONE',  ( 4.413617546364139166, -5.876774720514407413, 18.86076033669171181 ) ) ;
#54662 = CARTESIAN_POINT ( 'NONE',  ( -96.63573453449330941, -23.73766607897670511, -1.055555164236452681 ) ) ;
#54663 = LINE ( 'NONE', #69377, #30629 ) ;
#54664 = B_SPLINE_CURVE_WITH_KNOTS ( 'NONE', 3,
 ( #99881, #59862, #91294, #46634, #99398, #30389 ),
 .UNSPECIFIED., .F., .F.,
 ( 4, 2, 4 ),
 ( 0.000000000000000000, 0.001380901958385385509, 0.002761803916770771018 ),
 .UNSPECIFIED. ) ;
#54665 = CARTESIAN_POINT ( 'NONE',  ( 17.77913403553526805, 13.70458096452923691, 11.49999999999999645 ) ) ;
#54666 = ORIENTED_EDGE ( 'NONE', *, *, #79456, .T. ) ;
#54667 = CARTESIAN_POINT ( 'NONE',  ( -69.62287095715005592, -24.65952944569304961, 1.056160979905697017 ) ) ;
#54668 = CARTESIAN_POINT ( 'NONE',  ( -70.62287095715004170, -24.52323809116983355, 9.355190652339413049 ) ) ;
#54669 = CARTESIAN_POINT ( 'NONE',  ( 5.197331492371871420, 21.31670716312865466, 11.49999999999998934 ) ) ;
#54670 = CARTESIAN_POINT ( 'NONE',  ( -5.053929855541893446, -6.376774720514410077, 19.14848118821636547 ) ) ;
#54671 = CARTESIAN_POINT ( 'NONE',  ( -34.47819092748605385, -24.66019654487199730, 8.947790411086117501 ) ) ;
#54672 = CARTESIAN_POINT ( 'NONE',  ( -0.02075734969026423599, 6.475225279485573360, -0.08597719988137648983 ) ) ;
#54673 = VERTEX_POINT ( 'NONE', #12785 ) ;
#54674 = CARTESIAN_POINT ( 'NONE',  ( -25.92875734969025814, 3.316774720514426456, 30.51402280011862089 ) ) ;
#54675 = DIRECTION ( 'NONE',  ( 0.000000000000000000, -2.173523156925979552E-06, 0.9999999999976378895 ) ) ;
#54676 = ORIENTED_EDGE ( 'NONE', *, *, #78411, .F. ) ;
#54677 = CARTESIAN_POINT ( 'NONE',  ( -12.04554601739387998, 16.56303510970703385, 11.49999999999998934 ) ) ;
#54678 = EDGE_LOOP ( 'NONE', ( #96977, #16176, #19703, #16257 ) ) ;
#54679 = ORIENTED_EDGE ( 'NONE', *, *, #92934, .T. ) ;
#54680 = ORIENTED_EDGE ( 'NONE', *, *, #75756, .F. ) ;
#54681 = ORIENTED_EDGE ( 'NONE', *, *, #17578, .T. ) ;
#54682 = CARTESIAN_POINT ( 'NONE',  ( 0.1381291366035634904, -23.06709338131901532, -1.500000000000002220 ) ) ;
#54683 = CARTESIAN_POINT ( 'NONE',  ( -49.28099472632571576, -25.20958802453461089, 3.393435110817564215 ) ) ;
#54684 = CARTESIAN_POINT ( 'NONE',  ( -11.07518157712430096, -17.02944518001645946, -1.500000000000002220 ) ) ;
#54685 = VERTEX_POINT ( 'NONE', #27029 ) ;
#54686 = CIRCLE ( 'NONE', #74157, 2.500000000000000444 ) ;
#54687 = LINE ( 'NONE', #85618, #8807 ) ;
#54688 = CARTESIAN_POINT ( 'NONE',  ( -92.63100931479979749, -24.15543982623908192, -0.2315651400026453588 ) ) ;
#54689 = CARTESIAN_POINT ( 'NONE',  ( -28.52287095715006870, -23.78764107635717906, 10.65372851796821685 ) ) ;
#54690 = CARTESIAN_POINT ( 'NONE',  ( 4.653733606810938284, -5.876774720514412742, 19.95301661664751336 ) ) ;
#54692 = EDGE_LOOP ( 'NONE', ( #64082, #75565, #70249, #92832 ) ) ;
#54691 = CARTESIAN_POINT ( 'NONE',  ( -18.46100929034391314, -11.06139713797464985, 11.49999999999999645 ) ) ;
#54693 = CARTESIAN_POINT ( 'NONE',  ( -75.63387239539466123, -24.52300882791530512, 0.6510814631126415897 ) ) ;
#54694 = CARTESIAN_POINT ( 'NONE',  ( -94.62287095715005592, -24.64965695001469115, 8.947790433994180503 ) ) ;
#54695 = ORIENTED_EDGE ( 'NONE', *, *, #65787, .T. ) ;
#54696 = AXIS2_PLACEMENT_3D ( 'NONE', #38244, #46872, #100119 ) ;
#54697 = CARTESIAN_POINT ( 'NONE',  ( -17.23291202157775359, 11.51834372740795231, 11.49999999999998934 ) ) ;
#54698 = ORIENTED_EDGE ( 'NONE', *, *, #49595, .T. ) ;
#54700 = ORIENTED_EDGE ( 'NONE', *, *, #89084, .F. ) ;
#54699 = CARTESIAN_POINT ( 'NONE',  ( -69.86226847989213695, -25.12049686670126292, 2.832401160916445004 ) ) ;
#54701 = B_SPLINE_CURVE_WITH_KNOTS ( 'NONE', 3,
 ( #29109, #62073, #93496, #68681, #23986, #92005, #657, #7770, #39715, #7262, #84891, #160, #54958, #76762, #30104, #70674, #69679, #94002, #6767 ),
 .UNSPECIFIED., .F., .F.,
 ( 4, 1, 1, 1, 1, 1, 1, 1, 1, 1, 1, 1, 1, 1, 1, 1, 4 ),
 ( 0.000000000000000000, 0.07560433049574560860, 0.1479650154827357456, 0.2187969985237000203, 0.2894704453213765016, 0.3597242180874995476, 0.4297077387530455206, 0.5004965198485865630, 0.5744290198679483650, 0.6139472962286703916, 0.6571552698261112768, 0.7039727697209375856, 0.7549389848168005512, 0.8097066112894875101, 0.8688329536985499590, 0.9323854739325975194, 1.000000000000000000 ),
 .UNSPECIFIED. ) ;
#54702 = ADVANCED_FACE ( 'NONE', ( #87932 ), #41773, .F. ) ;
#54703 = B_SPLINE_SURFACE_WITH_KNOTS ( 'NONE', 3, 1, ( 
 ( #96679, #10444 ),
 ( #20058, #72861 ),
 ( #18557, #87575 ),
 ( #80461, #19554 ),
 ( #50513, #73848 ),
 ( #97186, #18059 ) ),
 .UNSPECIFIED., .F., .F., .F.,
 ( 4, 2, 4 ),
 ( 2, 2 ),
 ( 0.000000000000000000, 0.5000000000000000000, 1.000000000000000000 ),
 ( 0.000000000000000000, 1.000000000000000000 ),
 .UNSPECIFIED. ) ;
#54704 = CARTESIAN_POINT ( 'NONE',  ( -111.6272348879597587, -24.15620529776629510, 10.23563542870659582 ) ) ;
#54705 = LINE ( 'NONE', #71427, #50289 ) ;
#54706 = ORIENTED_EDGE ( 'NONE', *, *, #5546, .T. ) ;
#54707 = VERTEX_POINT ( 'NONE', #57499 ) ;
#54708 = ADVANCED_FACE ( 'NONE', ( #58492 ), #19900, .T. ) ;
#54709 = DIRECTION ( 'NONE',  ( 1.000000000000000000, 3.773278334444167608E-23, 8.201307833595939069E-29 ) ) ;
#54710 = CARTESIAN_POINT ( 'NONE',  ( -42.64759707562362934, -23.96169478059713143, 10.65365249895718947 ) ) ;
#54711 = CARTESIAN_POINT ( 'NONE',  ( -102.5228709571500332, -23.95044443724990657, 10.65354141964648882 ) ) ;
#54712 = CARTESIAN_POINT ( 'NONE',  ( -2.902263480631018577, 21.84654903556016947, 11.49999999999999645 ) ) ;
#54713 = EDGE_CURVE ( 'NONE', #17843, #76499, #4856, .T. ) ;
#54714 = CARTESIAN_POINT ( 'NONE',  ( -89.63470426873689689, -23.96169478059713498, 10.65365249895717703 ) ) ;
#54715 = CARTESIAN_POINT ( 'NONE',  ( 22.38532167473930556, -2.757513164441831144, -1.500000000000002220 ) ) ;
#54716 = EDGE_CURVE ( 'NONE', #55102, #93973, #52843, .T. ) ;
#54717 = AXIS2_PLACEMENT_3D ( 'NONE', #80937, #83797, #36628 ) ;
#54718 = CARTESIAN_POINT ( 'NONE',  ( -2.639205680565387624, -20.84613592336672028, 11.49999999999998934 ) ) ;
#54719 = EDGE_CURVE ( 'NONE', #48074, #72664, #10759, .T. ) ;
#54720 = VERTEX_POINT ( 'NONE', #29015 ) ;
#54721 = VERTEX_POINT ( 'NONE', #52364 ) ;
#54722 = EDGE_CURVE ( 'NONE', #27752, #35590, #22036, .T. ) ;
#54723 = DIRECTION ( 'NONE',  ( -0.000000000000000000, 1.000000000000000000, -0.000000000000000000 ) ) ;
#54724 = AXIS2_PLACEMENT_3D ( 'NONE', #19223, #35465, #73524 ) ;
#54725 = CARTESIAN_POINT ( 'NONE',  ( -113.6228709571500417, -24.50321055353806088, 9.387540953477516936 ) ) ;
#54726 = ORIENTED_EDGE ( 'NONE', *, *, #73493, .F. ) ;
#54727 = CARTESIAN_POINT ( 'NONE',  ( -1.424071398598787397, -21.11453822904667277, 11.49999999999998934 ) ) ;
#54728 = CARTESIAN_POINT ( 'NONE',  ( -83.62287095715005592, -24.64898659630528854, 1.056161002820826145 ) ) ;
#54729 = CARTESIAN_POINT ( 'NONE',  ( -51.78109907783319699, -25.26040949718250772, 6.793045023519886705 ) ) ;
#54730 = CARTESIAN_POINT ( 'NONE',  ( -49.71071415242499114, -25.29402636989360076, 4.468221159579485402 ) ) ;
#54731 = VECTOR ( 'NONE', #33127, 1000.000000000000000 ) ;
#54732 = CARTESIAN_POINT ( 'NONE',  ( -44.52287095715006160, -29.50247984919015209, -1.443849546365060466 ) ) ;
#54733 = DIRECTION ( 'NONE',  ( -3.773278334453079618E-23, 0.9999999999976377785, 2.173523156925979975E-06 ) ) ;
#54734 = CARTESIAN_POINT ( 'NONE',  ( -14.74362065938029076, 16.57599527146691898, -1.500000000000002220 ) ) ;
#54735 = CARTESIAN_POINT ( 'NONE',  ( -71.60770107105075510, -23.48783264082476663, -1.443836473390092578 ) ) ;
#54736 = EDGE_CURVE ( 'NONE', #28349, #73864, #67770, .T. ) ;
#54737 = ORIENTED_EDGE ( 'NONE', *, *, #10077, .F. ) ;
#54738 = CARTESIAN_POINT ( 'NONE',  ( 6.437068816671457583, 3.316774720514427344, -28.37834077173919667 ) ) ;
#54739 = CARTESIAN_POINT ( 'NONE',  ( -48.62287095715004881, -23.94994826722515313, -0.6494450866351707541 ) ) ;
#54740 = CARTESIAN_POINT ( 'NONE',  ( -126.6237062192220861, -24.51314013834316796, 0.6176544820404223923 ) ) ;
#54741 = CARTESIAN_POINT ( 'NONE',  ( -100.5044705759059269, -25.00158670708910691, 2.256160236439218369 ) ) ;
#54742 = FACE_OUTER_BOUND ( 'NONE', #87914, .T. ) ;
#54743 = EDGE_CURVE ( 'NONE', #12190, #68328, #21726, .T. ) ;
#54744 = CARTESIAN_POINT ( 'NONE',  ( 18.22972481837485859, -6.773019484731225504, 11.49999999999998934 ) ) ;
#54745 = B_SPLINE_CURVE_WITH_KNOTS ( 'NONE', 3,
 ( #55324, #78622, #17749, #32471 ),
 .UNSPECIFIED., .F., .F.,
 ( 4, 4 ),
 ( 0.000000000000000000, 9.999999999998206125E-05 ),
 .UNSPECIFIED. ) ;
#54746 = CARTESIAN_POINT ( 'NONE',  ( 20.74164082462262471, 5.259929546262127609, 11.49999999999998934 ) ) ;
#54747 = CARTESIAN_POINT ( 'NONE',  ( -68.94187076657172497, -25.24898040475824246, 6.277239383255088789 ) ) ;
#54748 = CARTESIAN_POINT ( 'NONE',  ( -94.52287095715006160, -24.64965694238575011, 8.947790433994196491 ) ) ;
#54749 = CARTESIAN_POINT ( 'NONE',  ( -28.84663072490566194, 0.3587747205144265483, 28.73989617533406715 ) ) ;
#54750 = CARTESIAN_POINT ( 'NONE',  ( -101.1478676400630405, -25.27360041239775512, 3.600571350085281175 ) ) ;
#54751 = CARTESIAN_POINT ( 'NONE',  ( -14.94938274637043207, -17.11189489004485864, -1.500000000000002220 ) ) ;
#54752 = EDGE_CURVE ( 'NONE', #84710, #28719, #26602, .T. ) ;
#54753 = CARTESIAN_POINT ( 'NONE',  ( -98.55492856983048000, -23.96119346886880663, -0.6495511937832080251 ) ) ;
#54754 = LINE ( 'NONE', #1966, #75108 ) ;
#54755 = CARTESIAN_POINT ( 'NONE',  ( -19.55781625546462976, 3.520333346782119843, 11.49999999999999645 ) ) ;
#54756 = CARTESIAN_POINT ( 'NONE',  ( -123.5546973089963956, -24.35071581493544457, 9.817618358456016381 ) ) ;
#54757 = CARTESIAN_POINT ( 'NONE',  ( -32.52287095715006160, -23.48783264083359867, -1.443836473376375329 ) ) ;
#54758 = ORIENTED_EDGE ( 'NONE', *, *, #19906, .F. ) ;
#54759 = FACE_OUTER_BOUND ( 'NONE', #23589, .T. ) ;
#54760 = DIRECTION ( 'NONE',  ( -0.000000000000000000, -1.000000000000000000, 0.000000000000000000 ) ) ;
#54761 = CARTESIAN_POINT ( 'NONE',  ( -117.5562042904833930, -24.66019654487199730, 8.947790411086121054 ) ) ;
#54762 = CARTESIAN_POINT ( 'NONE',  ( -10.04279811845843007, 19.21892966915218892, -1.500000000000002220 ) ) ;
#54763 = AXIS2_PLACEMENT_3D ( 'NONE', #24866, #84889, #55841 ) ;
#54764 = CARTESIAN_POINT ( 'NONE',  ( 6.983913900142676212, -1.335655600570678558, 18.31352460785937453 ) ) ;
#54765 = CARTESIAN_POINT ( 'NONE',  ( 5.650214204171827070, -18.61605495904187535, -1.500000000000002220 ) ) ;
#54766 = DIRECTION ( 'NONE',  ( -3.773278334444167608E-23, 1.000000000000000000, 0.000000000000000000 ) ) ;
#54767 = EDGE_CURVE ( 'NONE', #11050, #80312, #46390, .T. ) ;
#54768 = B_SPLINE_CURVE_WITH_KNOTS ( 'NONE', 3,
 ( #73327, #40371, #65239, #64742, #34758, #26649 ),
 .UNSPECIFIED., .F., .F.,
 ( 4, 2, 4 ),
 ( 1.570755371633797249E-05, 0.001396183895866087319, 0.002776660238015836446 ),
 .UNSPECIFIED. ) ;
#54769 = ORIENTED_EDGE ( 'NONE', *, *, #19531, .F. ) ;
#54770 = CARTESIAN_POINT ( 'NONE',  ( 18.82465703714932204, -7.861812626244089053, 11.49999999999999645 ) ) ;
#54771 = DIRECTION ( 'NONE',  ( -3.773278334453080206E-23, 0.9999999999976377785, 2.173523156925979975E-06 ) ) ;
#54772 = EDGE_CURVE ( 'NONE', #20834, #84257, #90862, .T. ) ;
#54773 = CARTESIAN_POINT ( 'NONE',  ( 10.24059822343757986, -5.876774720514426953, 22.82308057603840368 ) ) ;
#54774 = ORIENTED_EDGE ( 'NONE', *, *, #25474, .F. ) ;
#54775 = CARTESIAN_POINT ( 'NONE',  ( -40.70660919605776940, -25.19832496394808885, 3.317317603583394892 ) ) ;
#54776 = CARTESIAN_POINT ( 'NONE',  ( -92.52287095715006160, -23.94994826722565762, -0.6494450866342746931 ) ) ;
#54777 = LINE ( 'NONE', #61890, #56486 ) ;
#54778 = CARTESIAN_POINT ( 'NONE',  ( -40.57216639332711594, -25.00182538069146787, 7.747789668545040698 ) ) ;
#54779 = DIRECTION ( 'NONE',  ( 1.000000000000000000, 3.773278334444166432E-23, 8.201307841325785021E-29 ) ) ;
#54780 = CARTESIAN_POINT ( 'NONE',  ( 1.236116150138429903, -20.07036509671028668, 11.49999999999998934 ) ) ;
#54781 = EDGE_CURVE ( 'NONE', #78854, #50194, #37629, .T. ) ;
#54782 = DIRECTION ( 'NONE',  ( 0.9951627101165076983, -0.09824042138329622254, -3.430045979798646929E-16 ) ) ;
#54783 = ORIENTED_EDGE ( 'NONE', *, *, #65772, .F. ) ;
#54784 = CARTESIAN_POINT ( 'NONE',  ( -82.22287095715006444, -23.47593901973090169, -1.443836447538997092 ) ) ;
#54785 = VECTOR ( 'NONE', #60131, 1000.000000000000000 ) ;
#54786 = CARTESIAN_POINT ( 'NONE',  ( 6.305670413343573699, 22.00876638805999974, 11.49999999999999645 ) ) ;
#54787 = CARTESIAN_POINT ( 'NONE',  ( -20.26579564662877075, -10.28286414166031726, 11.49999999999998934 ) ) ;
#54788 = ORIENTED_EDGE ( 'NONE', *, *, #78685, .T. ) ;
#54789 = CARTESIAN_POINT ( 'NONE',  ( -71.66738459694697383, -25.21749834187382078, 6.546833690950035312 ) ) ;
#54790 = LINE ( 'NONE', #78093, #99591 ) ;
#54791 = LINE ( 'NONE', #54294, #85692 ) ;
#54792 = CARTESIAN_POINT ( 'NONE',  ( -30.57287095715006586, -23.79279866861233828, 10.96694982589930767 ) ) ;
#54793 = VECTOR ( 'NONE', #97970, 1000.000000000000114 ) ;
#54794 = CARTESIAN_POINT ( 'NONE',  ( -118.6228709571500701, -23.48786465467241769, 11.44779295918253759 ) ) ;
#54795 = CARTESIAN_POINT ( 'NONE',  ( -98.90869474253671001, -25.31200697284943146, 5.895134381143665614 ) ) ;
#54796 = ORIENTED_EDGE ( 'NONE', *, *, #2639, .T. ) ;
#54797 = VECTOR ( 'NONE', #63518, 1000.000000000000114 ) ;
#54798 = CARTESIAN_POINT ( 'NONE',  ( -13.40315722217803973, 15.35114911505495172, -1.500000000000002220 ) ) ;
#54799 = ORIENTED_EDGE ( 'NONE', *, *, #14674, .F. ) ;
#54800 = CARTESIAN_POINT ( 'NONE',  ( 4.903590608199674072, 22.46510890469962263, -1.500000000000002220 ) ) ;
#54801 = DIRECTION ( 'NONE',  ( 1.000000000000000000, 3.773278334444166432E-23, 8.201307841325785021E-29 ) ) ;
#54802 = EDGE_LOOP ( 'NONE', ( #41890, #47122, #2580, #87495, #57601 ) ) ;
#54803 = CARTESIAN_POINT ( 'NONE',  ( -108.6314038554107100, -23.73791477778912196, 11.05961554403169878 ) ) ;
#54804 = DIRECTION ( 'NONE',  ( -0.000000000000000000, 1.000000000000000000, -0.000000000000000000 ) ) ;
#54805 = CARTESIAN_POINT ( 'NONE',  ( -89.55620429048340725, -24.65952944569304606, 1.056160979905701014 ) ) ;
#54806 = AXIS2_PLACEMENT_3D ( 'NONE', #73232, #17431, #27051 ) ;
#54808 = VERTEX_POINT ( 'NONE', #30515 ) ;
#54807 = CARTESIAN_POINT ( 'NONE',  ( 3.065528897535349628, -21.08962430476942274, 11.49999999999999645 ) ) ;
#54809 = ORIENTED_EDGE ( 'NONE', *, *, #91943, .T. ) ;
#54810 = CARTESIAN_POINT ( 'NONE',  ( 21.63176498729014341, 4.993826359924048219, -1.500000000000002220 ) ) ;
#54811 = CARTESIAN_POINT ( 'NONE',  ( 14.37238272058661259, 14.81585024043302035, 11.49999999999998934 ) ) ;
#54812 = B_SPLINE_CURVE_WITH_KNOTS ( 'NONE', 3,
 ( #12513, #43480, #19624, #88155, #66830, #35369 ),
 .UNSPECIFIED., .F., .F.,
 ( 4, 2, 4 ),
 ( 1.570755371634033063E-05, 0.001396183895866089488, 0.002776660238015838614 ),
 .UNSPECIFIED. ) ;
#54813 = ORIENTED_EDGE ( 'NONE', *, *, #95128, .F. ) ;
#54814 = ORIENTED_EDGE ( 'NONE', *, *, #15652, .F. ) ;
#54815 = CARTESIAN_POINT ( 'NONE',  ( -108.9979829822171951, -25.27682655912521881, 4.539662868468415269 ) ) ;
#54816 = ADVANCED_FACE ( 'NONE', ( #91407 ), #21884, .T. ) ;
#54817 = CARTESIAN_POINT ( 'NONE',  ( -95.62462548333338930, -24.92592662359561473, 8.075495903017998245 ) ) ;
#54818 = ORIENTED_EDGE ( 'NONE', *, *, #91243, .T. ) ;
#54819 = EDGE_CURVE ( 'NONE', #66922, #17140, #22385, .T. ) ;
#54820 = CARTESIAN_POINT ( 'NONE',  ( -50.40445135320378967, -25.13313949306887451, 7.101635536975466678 ) ) ;
#54821 = EDGE_LOOP ( 'NONE', ( #70989, #17643, #85359, #71544 ) ) ;
#54823 = ADVANCED_FACE ( 'NONE', ( #60981 ), #61482, .T. ) ;
#54822 = CARTESIAN_POINT ( 'NONE',  ( -58.54268383830879685, -24.35071581493543036, 9.817618358456028815 ) ) ;
#54824 = PLANE ( 'NONE',  #29268 ) ;
#54825 = CARTESIAN_POINT ( 'NONE',  ( -17.75621389795859884, -10.86975384844714831, -1.500000000000002220 ) ) ;
#54826 = CARTESIAN_POINT ( 'NONE',  ( 19.17057494584436839, 10.47865234463220396, 11.49999999999999645 ) ) ;
#54827 = ADVANCED_FACE ( 'NONE', ( #76668 ), #53369, .T. ) ;
#54828 = FACE_OUTER_BOUND ( 'NONE', #99495, .T. ) ;
#54829 = CARTESIAN_POINT ( 'NONE',  ( -78.54638029082808259, -24.35071581493543391, 9.817618358456027039 ) ) ;
#54830 = CARTESIAN_POINT ( 'NONE',  ( 19.77452139984142221, -10.64395493966388706, -1.500000000000002220 ) ) ;
#54831 = EDGE_CURVE ( 'NONE', #1282, #60109, #43148, .T. ) ;
#54832 = CARTESIAN_POINT ( 'NONE',  ( -38.64868663285562178, -23.96119346886880308, -0.6495511937831990323 ) ) ;
#54833 = CARTESIAN_POINT ( 'NONE',  ( -87.58953762381671027, -23.48783264082478794, -1.443836473390063269 ) ) ;
#54834 = CARTESIAN_POINT ( 'NONE',  ( -32.30247028140506416, 6.475225279485573360, 27.60502002861223048 ) ) ;
#54835 = B_SPLINE_SURFACE_WITH_KNOTS ( 'NONE', 3, 3, ( 
 ( #55851, #47730, #541, #95398 ),
 ( #78646, #79664, #8662, #31489 ),
 ( #41122, #93380, #10163, #25382 ),
 ( #62453, #2066, #85785, #25887 ),
 ( #16267, #63980, #9152, #94393 ),
 ( #17270, #56859, #11159, #82167 ),
 ( #19753, #3064, #50729, #57857 ),
 ( #18763, #5044, #51224, #34004 ),
 ( #12651, #81674, #96396, #12147 ),
 ( #88797, #43117, #42627, #4055 ) ),
 .UNSPECIFIED., .F., .F., .F.,
 ( 4, 3, 3, 4 ),
 ( 4, 4 ),
 ( 0.7022005934544806038, 0.7765311282028796169, 0.8508616629512786300, 0.9995227324480766562 ),
 ( 0.7995904963587343595, 0.8010797657131805138 ),
 .UNSPECIFIED. ) ;
#54836 = ORIENTED_EDGE ( 'NONE', *, *, #19409, .F. ) ;
#54837 = ORIENTED_EDGE ( 'NONE', *, *, #85735, .T. ) ;
#54838 = ORIENTED_EDGE ( 'NONE', *, *, #67321, .T. ) ;
#54839 = CARTESIAN_POINT ( 'NONE',  ( -20.23222619987061677, -6.887663580918623296, -1.500000000000002220 ) ) ;
#54840 = ORIENTED_EDGE ( 'NONE', *, *, #70466, .F. ) ;
#54841 = CARTESIAN_POINT ( 'NONE',  ( -20.88184962559319402, -2.832954952542597660, 11.49999999999998934 ) ) ;
#54842 = CARTESIAN_POINT ( 'NONE',  ( -30.46019145506044623, -23.77870465984290149, -0.9707498849204322378 ) ) ;
#54843 = CARTESIAN_POINT ( 'NONE',  ( -11.44242300287478820, -16.35863574123370512, -1.500000000000002220 ) ) ;
#54844 = DIRECTION ( 'NONE',  ( -1.000000000000000000, -0.000000000000000000, -0.000000000000000000 ) ) ;
#54845 = CARTESIAN_POINT ( 'NONE',  ( -50.40895856474225667, -25.04307398257883577, 7.563174194274489892 ) ) ;
#54846 = CARTESIAN_POINT ( 'NONE',  ( -12.87221125579857528, -17.80329210173279364, -1.500000000000002220 ) ) ;
#54847 = PLANE ( 'NONE',  #73920 ) ;
#54848 = ORIENTED_EDGE ( 'NONE', *, *, #74195, .T. ) ;
#54849 = CARTESIAN_POINT ( 'NONE',  ( -111.5228709571500616, -29.50250243563736774, 8.947779886222136270 ) ) ;
#54850 = B_SPLINE_CURVE_WITH_KNOTS ( 'NONE', 3,
 ( #40083, #63441, #94361, #24847, #2034, #2737, #88966 ),
 .UNSPECIFIED., .F., .F.,
 ( 4, 1, 1, 1, 4 ),
 ( 0.000000000000000000, 0.2835948081386937547, 0.5433948405759735367, 0.7806456291745620391, 1.000000000000000000 ),
 .UNSPECIFIED. ) ;
#54851 = CARTESIAN_POINT ( 'NONE',  ( -121.5228709571500048, -23.47593901973090524, -1.443836447538996204 ) ) ;
#54852 = CARTESIAN_POINT ( 'NONE',  ( -5.744250498300313090, 20.02623800365557472, 11.49999999999999645 ) ) ;
#54853 = VECTOR ( 'NONE', #80589, 1000.000000000000227 ) ;
#54854 = B_SPLINE_CURVE_WITH_KNOTS ( 'NONE', 3,
 ( #75897, #74897, #29732, #75396, #82518, #4907 ),
 .UNSPECIFIED., .F., .F.,
 ( 4, 2, 4 ),
 ( 0.000000000000000000, 0.001380901958385387027, 0.002761803916770774053 ),
 .UNSPECIFIED. ) ;
#54855 = CARTESIAN_POINT ( 'NONE',  ( 29.58524742607616176, -4.112217781777255610, 29.11978736867098760 ) ) ;
#54856 = CARTESIAN_POINT ( 'NONE',  ( -5.576923076923076650, -5.876774720514418071, 20.44941907051282470 ) ) ;
#54857 = CARTESIAN_POINT ( 'NONE',  ( -38.62287095715004881, -23.96177878511306503, 10.65340807706330395 ) ) ;
#54858 = CARTESIAN_POINT ( 'NONE',  ( -20.61954105445765251, -5.431428859615135885, 11.49999999999998934 ) ) ;
#54859 = CARTESIAN_POINT ( 'NONE',  ( -98.52218354524907795, -23.48786465467241769, 11.44779295918254469 ) ) ;
#54860 = DIRECTION ( 'NONE',  ( -3.773278334453079618E-23, 0.9999999999976377785, 2.173523156925979975E-06 ) ) ;
#54861 = LINE ( 'NONE', #2574, #55231 ) ;
#54862 = CARTESIAN_POINT ( 'NONE',  ( -5.554587162835583847, -5.876774720514417183, 19.99258394656885329 ) ) ;
#54863 = CARTESIAN_POINT ( 'NONE',  ( -3.310667818835141940, 22.29536907041311977, -1.500000000000002220 ) ) ;
#54864 = CARTESIAN_POINT ( 'NONE',  ( -129.6228709571500417, -24.66019654487200086, 8.947790411086117501 ) ) ;
#54865 = ORIENTED_EDGE ( 'NONE', *, *, #65397, .F. ) ;
#54866 = CARTESIAN_POINT ( 'NONE',  ( -51.26855917001611829, -25.30346314791453821, 5.552786049883900787 ) ) ;
#54867 = CARTESIAN_POINT ( 'NONE',  ( 2.993365552154886089, -5.876774720514413630, 19.24059921568563425 ) ) ;
#54868 = CARTESIAN_POINT ( 'NONE',  ( -13.08164486973500118, 14.69858247433046650, 11.49999999999999645 ) ) ;
#54869 = FACE_OUTER_BOUND ( 'NONE', #52138, .T. ) ;
#54870 = VECTOR ( 'NONE', #85968, 1000.000000000000114 ) ;
#54871 = CARTESIAN_POINT ( 'NONE',  ( 14.83405752585509596, -4.881907540129173384, -27.54622755360215791 ) ) ;
#54872 = ORIENTED_EDGE ( 'NONE', *, *, #18656, .T. ) ;
#54873 = DIRECTION ( 'NONE',  ( -1.000000000000000000, -3.773278334444165844E-23, -8.201307836089272790E-29 ) ) ;
#54874 = CARTESIAN_POINT ( 'NONE',  ( -65.05438548721848235, 6.475225279485573360, 0.7300228001186309656 ) ) ;
#54875 = FACE_OUTER_BOUND ( 'NONE', #60804, .T. ) ;
#54876 = FACE_OUTER_BOUND ( 'NONE', #91085, .T. ) ;
#54877 = CARTESIAN_POINT ( 'NONE',  ( 3.553741186906278493, -19.43417129498564577, -1.500000000000002220 ) ) ;
#54878 = AXIS2_PLACEMENT_3D ( 'NONE', #73733, #66153, #74233 ) ;
#54879 = VERTEX_POINT ( 'NONE', #37131 ) ;
#54880 = CARTESIAN_POINT ( 'NONE',  ( -120.5228709571500900, -25.00182538069145366, 7.747789668545101982 ) ) ;
#54881 = EDGE_CURVE ( 'NONE', #29962, #32572, #37560, .T. ) ;
#54882 = PERSON_AND_ORGANIZATION_ROLE ( 'creator' ) ;
#54883 = EDGE_CURVE ( 'NONE', #19708, #13572, #13935, .T. ) ;
#54884 = ORIENTED_EDGE ( 'NONE', *, *, #57699, .F. ) ;
#54885 = PLANE ( 'NONE',  #69402 ) ;
#54886 = CARTESIAN_POINT ( 'NONE',  ( -53.62287095715005592, -24.64898659630528499, 1.056161002820821038 ) ) ;
#54887 = CARTESIAN_POINT ( 'NONE',  ( 18.22465585706453339, -0.5000000000000000000, -2.153101996372891236 ) ) ;
#54888 = CARTESIAN_POINT ( 'NONE',  ( -98.89303308397303738, -25.03144863224170180, 6.110950661846722198 ) ) ;
#54889 = CARTESIAN_POINT ( 'NONE',  ( 5.464387484610083057, -6.376774720514420736, 21.31215092858952431 ) ) ;
#54890 = B_SPLINE_CURVE_WITH_KNOTS ( 'NONE', 3,
 ( #67355, #98275, #99280, #28781, #43019, #90677 ),
 .UNSPECIFIED., .F., .F.,
 ( 4, 2, 4 ),
 ( 0.000000000000000000, 0.001380764517854760195, 0.002761529035709520390 ),
 .UNSPECIFIED. ) ;
#54891 = CARTESIAN_POINT ( 'NONE',  ( -4.141025641025642301, -5.876774720514409189, 19.19230769230769695 ) ) ;
#54892 = DIRECTION ( 'NONE',  ( 0.000000000000000000, 0.000000000000000000, 1.000000000000000000 ) ) ;
#54893 = CARTESIAN_POINT ( 'NONE',  ( -18.81269933604069067, 6.858547123926768130, 11.49999999999998934 ) ) ;
#54894 = CARTESIAN_POINT ( 'NONE',  ( -117.5228709571500758, -24.64898659630368272, 1.056161002820833028 ) ) ;
#54895 = FACE_OUTER_BOUND ( 'NONE', #53433, .T. ) ;
#54896 = ORIENTED_EDGE ( 'NONE', *, *, #48658, .T. ) ;
#54897 = CARTESIAN_POINT ( 'NONE',  ( -79.50884703881661153, -24.15620529776628089, 10.23563542870660470 ) ) ;
#54898 = CARTESIAN_POINT ( 'NONE',  ( -109.3608459871604026, -25.29012903889914554, 4.114984869304729287 ) ) ;
#54899 = CARTESIAN_POINT ( 'NONE',  ( -58.52287095715006870, -24.35013146730203815, 9.818937971375103047 ) ) ;
#54900 = CARTESIAN_POINT ( 'NONE',  ( -101.5468792378191836, -25.25287247409163527, 6.236250661346386615 ) ) ;
#54901 = CARTESIAN_POINT ( 'NONE',  ( -117.5801350442859672, -25.31825869351653679, 3.539998670762450672 ) ) ;
#54902 = FACE_OUTER_BOUND ( 'NONE', #33717, .T. ) ;
#54903 = FACE_OUTER_BOUND ( 'NONE', #96277, .T. ) ;
#54904 = LINE ( 'NONE', #78218, #37169 ) ;
#54905 = ORIENTED_EDGE ( 'NONE', *, *, #99060, .F. ) ;
#54906 = AXIS2_PLACEMENT_3D ( 'NONE', #86286, #40118, #15767 ) ;
#54907 = CARTESIAN_POINT ( 'NONE',  ( 6.844040470191356640, -19.11863935190610064, -1.500000000000002220 ) ) ;
#54908 = CARTESIAN_POINT ( 'NONE',  ( 22.81105451610979173, 2.682774720514426559, -18.46691820600746681 ) ) ;
#54909 = AXIS2_PLACEMENT_3D ( 'NONE', #30214, #75890, #6391 ) ;
#54910 = LINE ( 'NONE', #85853, #70313 ) ;
#54911 = ORIENTED_EDGE ( 'NONE', *, *, #35247, .F. ) ;
#54912 = EDGE_CURVE ( 'NONE', #27060, #73557, #87169, .T. ) ;
#54913 = CARTESIAN_POINT ( 'NONE',  ( 31.59245846751552378, -5.049734226592146769, -4.287355462049295518 ) ) ;
#54914 = CARTESIAN_POINT ( 'NONE',  ( -12.46103870137906711, 15.87156016069071462, -1.500000000000002220 ) ) ;
#54915 = CARTESIAN_POINT ( 'NONE',  ( -15.95541298346445735, 13.85296639876547076, 11.49999999999999645 ) ) ;
#54916 = VECTOR ( 'NONE', #1369, 1000.000000000000000 ) ;
#54917 = CARTESIAN_POINT ( 'NONE',  ( 14.84500176111689207, -16.38379996218902335, 11.49999999999998934 ) ) ;
#54918 = CARTESIAN_POINT ( 'NONE',  ( 4.814550503181614260, -19.98661186389175271, -1.500000000000002220 ) ) ;
#54919 = CARTESIAN_POINT ( 'NONE',  ( -60.60739371882706195, -23.85016227208579664, -0.8807180028928355275 ) ) ;
#54920 = ORIENTED_EDGE ( 'NONE', *, *, #12563, .F. ) ;
#54921 = CARTESIAN_POINT ( 'NONE',  ( -32.62287095715007013, -23.94994826722565406, -0.6494450866342722506 ) ) ;
#54922 = ORIENTED_EDGE ( 'NONE', *, *, #13967, .T. ) ;
#54923 = CARTESIAN_POINT ( 'NONE',  ( -51.62287095715006302, -24.33832256527048088, 0.1851278514138594566 ) ) ;
#54924 = CARTESIAN_POINT ( 'NONE',  ( -70.52287095715010423, -23.84081130425358097, 10.88220057483159664 ) ) ;
#54925 = EDGE_LOOP ( 'NONE', ( #20818, #59839, #71153, #56117 ) ) ;
#54927 = ORIENTED_EDGE ( 'NONE', *, *, #6045, .T. ) ;
#54926 = EDGE_CURVE ( 'NONE', #65683, #44226, #50874, .T. ) ;
#54928 = AXIS2_PLACEMENT_3D ( 'NONE', #30826, #92218, #98322 ) ;
#54929 = ORIENTED_EDGE ( 'NONE', *, *, #86679, .T. ) ;
#54930 = LINE ( 'NONE', #9238, #37306 ) ;
#54931 = CARTESIAN_POINT ( 'NONE',  ( -113.5228709571500616, -29.50247984919015209, -1.443849546365048253 ) ) ;
#54932 = CARTESIAN_POINT ( 'NONE',  ( -2.717543299849222826, 17.80004702990586196, 0.000000000000000000 ) ) ;
#54933 = CARTESIAN_POINT ( 'NONE',  ( -6.358105417860958397, -19.66046682221446318, -1.500000000000002220 ) ) ;
#54934 = CARTESIAN_POINT ( 'NONE',  ( 4.495418090846292181, 21.21921847905042569, 11.49999999999999645 ) ) ;
#54935 = ORIENTED_EDGE ( 'NONE', *, *, #39012, .F. ) ;
#54936 = EDGE_CURVE ( 'NONE', #18736, #32470, #35056, .T. ) ;
#54937 = DIRECTION ( 'NONE',  ( -1.000000000000000000, -0.000000000000000000, -0.000000000000000000 ) ) ;
#54938 = DIRECTION ( 'NONE',  ( -0.4771587602595988020, -0.8788171126619706008, -0.000000000000000000 ) ) ;
#54939 = CARTESIAN_POINT ( 'NONE',  ( -19.80502325505778671, 10.42642913751328670, 11.49999999999998934 ) ) ;
#54940 = EDGE_CURVE ( 'NONE', #100313, #9886, #41170, .T. ) ;
#54941 = CARTESIAN_POINT ( 'NONE',  ( -79.42863770186421846, -25.12205661262295919, 6.408999591950016672 ) ) ;
#54942 = CARTESIAN_POINT ( 'NONE',  ( -120.6228709571499706, -24.82576562982392687, 8.398263435472960836 ) ) ;
#54943 = ORIENTED_EDGE ( 'NONE', *, *, #66528, .F. ) ;
#54944 = B_SPLINE_CURVE_WITH_KNOTS ( 'NONE', 3,
 ( #4797, #50473, #75290, #34748 ),
 .UNSPECIFIED., .F., .F.,
 ( 4, 4 ),
 ( 0.000000000000000000, 9.999999999998897304E-05 ),
 .UNSPECIFIED. ) ;
#54945 = CARTESIAN_POINT ( 'NONE',  ( 33.07248226229787491, -4.977706540348799891, -12.91345179487514905 ) ) ;
#54946 = CARTESIAN_POINT ( 'NONE',  ( -35.54073533905776827, -24.40133493613049609, 9.663955038902800609 ) ) ;
#54947 = ADVANCED_FACE ( 'NONE', ( #33029 ), #46753, .F. ) ;
#54948 = CARTESIAN_POINT ( 'NONE',  ( 8.587038044527741221, -19.06309208085484386, -1.500000000000002220 ) ) ;
#54949 = ADVANCED_FACE ( 'NONE', ( #47253 ), #85299, .F. ) ;
#54950 = EDGE_LOOP ( 'NONE', ( #63933, #15523, #21113, #56095 ) ) ;
#54951 = CARTESIAN_POINT ( 'NONE',  ( -20.27875734969026311, -4.543225279485573864, 24.00402280011862288 ) ) ;
#54952 = VERTEX_POINT ( 'NONE', #93407 ) ;
#54953 = CARTESIAN_POINT ( 'NONE',  ( -50.62287095715008434, -24.51254535404256529, 9.355368623467660072 ) ) ;
#54954 = CARTESIAN_POINT ( 'NONE',  ( 8.100108036306837178, -19.54698220168213041, -1.500000000000002220 ) ) ;
#54955 = ORIENTED_EDGE ( 'NONE', *, *, #90530, .T. ) ;
#54956 = CARTESIAN_POINT ( 'NONE',  ( -118.5228709571500758, -29.50248528299804818, 1.056150453629045360 ) ) ;
#54957 = CARTESIAN_POINT ( 'NONE',  ( -21.44618410820073606, 4.064364382921047181, -1.500000000000002220 ) ) ;
#54958 = CARTESIAN_POINT ( 'NONE',  ( -7.603582339867426043, -6.376774720514417183, 19.86545874326176175 ) ) ;
#54959 = FACE_OUTER_BOUND ( 'NONE', #91379, .T. ) ;
#54960 = CARTESIAN_POINT ( 'NONE',  ( -40.41683116089613748, -25.31532428806244539, 5.082404371757057504 ) ) ;
#54961 = CARTESIAN_POINT ( 'NONE',  ( 9.495391690522565042, 19.61495305411445500, -1.500000000000002220 ) ) ;
#54962 = CARTESIAN_POINT ( 'NONE',  ( -67.22287095715005023, -23.47593901973090169, -1.443836447538997536 ) ) ;
#54963 = ORIENTED_EDGE ( 'NONE', *, *, #26779, .F. ) ;
#54964 = ADVANCED_FACE ( 'NONE', ( #9687 ), #71597, .T. ) ;
#54965 = CARTESIAN_POINT ( 'NONE',  ( -30.57287095715006942, -23.48213395187224606, 11.44779283644488999 ) ) ;
#54966 = CARTESIAN_POINT ( 'NONE',  ( -85.50024737997124191, -24.73531770709095312, 8.716586749053508498 ) ) ;
#54967 = ORIENTED_EDGE ( 'NONE', *, *, #76438, .F. ) ;
#54968 = ORIENTED_EDGE ( 'NONE', *, *, #17773, .F. ) ;
#54969 = B_SPLINE_CURVE_WITH_KNOTS ( 'NONE', 3,
 ( #1177, #26888, #19264, #11652 ),
 .UNSPECIFIED., .F., .F.,
 ( 4, 4 ),
 ( 0.000000000000000000, 9.999999999998900014E-05 ),
 .UNSPECIFIED. ) ;
#54970 = ORIENTED_EDGE ( 'NONE', *, *, #70450, .T. ) ;
#54971 = DIRECTION ( 'NONE',  ( 3.773278334444166432E-23, -1.000000000000000000, 0.000000000000000000 ) ) ;
#54972 = CARTESIAN_POINT ( 'NONE',  ( -31.24388727629348139, -25.16930718282847579, 7.183628892452282422 ) ) ;
#54973 = CARTESIAN_POINT ( 'NONE',  ( 13.55612473118199723, -16.30799122071102403, -1.500000000000002220 ) ) ;
#54974 = CARTESIAN_POINT ( 'NONE',  ( -94.62287095715001328, -24.51283580621365132, 0.6167428607019771469 ) ) ;
#54975 = PLANE ( 'NONE',  #53492 ) ;
#54976 = CARTESIAN_POINT ( 'NONE',  ( 30.32108885906865936, 4.540774720514427543, 3.274824222184972822 ) ) ;
#54977 = ADVANCED_BREP_SHAPE_REPRESENTATION ( '', ( #42411, #37391 ), #16366 ) ;
#54978 = CARTESIAN_POINT ( 'NONE',  ( 11.07193147992585835, -15.93265361536492364, 11.49999999999998934 ) ) ;
#54979 = CARTESIAN_POINT ( 'NONE',  ( -51.92621816357582532, -25.27152954406082230, 6.039110851711205541 ) ) ;
#54980 = EDGE_LOOP ( 'NONE', ( #29361, #72765, #25030, #21570 ) ) ;
#54981 = CARTESIAN_POINT ( 'NONE',  ( 12.63578256557813795, 14.83599306707809085, 11.49999999999999645 ) ) ;
#54982 = DIRECTION ( 'NONE',  ( -1.000000000000000000, -1.224646799147353207E-16, 0.000000000000000000 ) ) ;
#54983 = AXIS2_PLACEMENT_3D ( 'NONE', #35812, #90099, #20573 ) ;
#54984 = FACE_OUTER_BOUND ( 'NONE', #18988, .T. ) ;
#54985 = ADVANCED_FACE ( 'NONE', ( #40646 ), #24902, .F. ) ;
#54986 = ORIENTED_EDGE ( 'NONE', *, *, #91014, .T. ) ;
#54987 = CARTESIAN_POINT ( 'NONE',  ( -58.62287095715004881, -24.50321055353806443, 9.387540953477540029 ) ) ;
#54988 = CARTESIAN_POINT ( 'NONE',  ( -70.35227678678285201, -25.30467589278440244, 4.853662785711239991 ) ) ;
#54989 = VECTOR ( 'NONE', #88014, 1000.000000000000000 ) ;
#54990 = DIRECTION ( 'NONE',  ( 7.960204194457801640E-17, 1.000000000000000000, 0.000000000000000000 ) ) ;
#54991 = EDGE_CURVE ( 'NONE', #37559, #15956, #62994, .T. ) ;
#54992 = CARTESIAN_POINT ( 'NONE',  ( -55.62287095715009144, -24.15431212366392444, -0.2830839119429288120 ) ) ;
#54993 = CARTESIAN_POINT ( 'NONE',  ( -14.15603575923578283, -13.64839490926926580, 11.49999999999998934 ) ) ;
#54994 = AXIS2_PLACEMENT_3D ( 'NONE', #53062, #29708, #92590 ) ;
#54995 = CARTESIAN_POINT ( 'NONE',  ( -41.29362909362059497, -25.31583684833336179, 4.684754115636811989 ) ) ;
#54996 = ORIENTED_EDGE ( 'NONE', *, *, #15857, .F. ) ;
#54997 = CARTESIAN_POINT ( 'NONE',  ( -15.49073194614445015, 15.02706685249526686, -1.500000000000002220 ) ) ;
#54998 = CIRCLE ( 'NONE', #74472, 28.96799999999999642 ) ;
#54999 = FACE_OUTER_BOUND ( 'NONE', #19597, .T. ) ;
#55000 = DIRECTION ( 'NONE',  ( -1.000000000000000000, -0.000000000000000000, -0.000000000000000000 ) ) ;
#55001 = CARTESIAN_POINT ( 'NONE',  ( -46.52287095715007581, -23.47593901973090524, -1.443836447538997314 ) ) ;
#55002 = EDGE_CURVE ( 'NONE', #16487, #55933, #8186, .T. ) ;
#55003 = VECTOR ( 'NONE', #82284, 1000.000000000000114 ) ;
#55004 = PERSON_AND_ORGANIZATION ( #70597, #27821 ) ;
#55005 = EDGE_CURVE ( 'NONE', #22611, #74525, #56385, .T. ) ;
#55006 = DIRECTION ( 'NONE',  ( 0.000000000000000000, 0.9999999999976377785, 2.173523156925979128E-06 ) ) ;
#55007 = DIRECTION ( 'NONE',  ( 0.000000000000000000, 0.9999999999976377785, 2.173523156925979975E-06 ) ) ;
#55008 = CARTESIAN_POINT ( 'NONE',  ( 6.365284455128204399, -6.376774720514413630, 19.73076923076922640 ) ) ;
#55009 = PLANE ( 'NONE',  #20744 ) ;
#55010 = CARTESIAN_POINT ( 'NONE',  ( -110.0268685312161665, -25.19071142001657293, 3.335046394459539876 ) ) ;
#55011 = CARTESIAN_POINT ( 'NONE',  ( -98.52287095715006160, -24.64898659630368272, 1.056161002820829697 ) ) ;
#55012 = CARTESIAN_POINT ( 'NONE',  ( -111.3776484685884327, -25.29779381075475442, 4.332404409858182426 ) ) ;
#55013 = CARTESIAN_POINT ( 'NONE',  ( -3.169371320753151977, 19.67850563098683736, 11.49999999999998934 ) ) ;
#55014 = CARTESIAN_POINT ( 'NONE',  ( -41.62287095715006302, -23.48783264082477729, -1.443836473390071928 ) ) ;
#55015 = CARTESIAN_POINT ( 'NONE',  ( -11.18921147948170614, -16.41150865552512883, -1.500000000000002220 ) ) ;
#55016 = CARTESIAN_POINT ( 'NONE',  ( -10.75273025779354796, -6.376774720514426953, 23.03521261039436752 ) ) ;
#55017 = CARTESIAN_POINT ( 'NONE',  ( -33.62287095715005592, -24.64898659630367206, 1.056161002820817485 ) ) ;
#55018 = LINE ( 'NONE', #40784, #73441 ) ;
#55019 = CARTESIAN_POINT ( 'NONE',  ( -10.32638548400381673, 17.97674989526738898, 11.49999999999999645 ) ) ;
#55020 = PLANE ( 'NONE',  #64610 ) ;
#55021 = PRODUCT_RELATED_PRODUCT_CATEGORY ( 'detail', '', ( #51515 ) ) ;
#55022 = DIRECTION ( 'NONE',  ( 0.000000000000000000, -0.9999999999976377785, -2.173523156925979128E-06 ) ) ;
#55023 = CARTESIAN_POINT ( 'NONE',  ( 21.14626179850551324, 8.528272852130310611, 11.49999999999999645 ) ) ;
#55024 = ORIENTED_EDGE ( 'NONE', *, *, #93759, .F. ) ;
#55025 = CARTESIAN_POINT ( 'NONE',  ( -83.62287095715012697, -24.35013146730204170, 9.818937971375106599 ) ) ;
#55026 = DIRECTION ( 'NONE',  ( -0.9888510809027408754, 5.365801633547210331E-16, -0.1489078231574191558 ) ) ;
#55027 = ORIENTED_EDGE ( 'NONE', *, *, #20421, .F. ) ;
#55028 = CARTESIAN_POINT ( 'NONE',  ( 18.20877288740043198, -8.745817889818592761, 11.49999999999998934 ) ) ;
#55029 = CARTESIAN_POINT ( 'NONE',  ( 8.984133506251076540, -0.9496381019629098752, -3.727086380289611256 ) ) ;
#55030 = CARTESIAN_POINT ( 'NONE',  ( -69.62287095715005592, -23.48783264082478084, -1.443836473390067265 ) ) ;
#55031 = ORIENTED_EDGE ( 'NONE', *, *, #38030, .T. ) ;
#55032 = B_SPLINE_CURVE_WITH_KNOTS ( 'NONE', 3,
 ( #27650, #26648, #41883, #58594, #72831, #3330 ),
 .UNSPECIFIED., .F., .F.,
 ( 4, 2, 4 ),
 ( 6.384118694792690538E-06, 0.001386860460836467687, 0.002767336802978142760 ),
 .UNSPECIFIED. ) ;
#55033 = B_SPLINE_CURVE_WITH_KNOTS ( 'NONE', 3,
 ( #79709, #13062, #11206, #74958 ),
 .UNSPECIFIED., .F., .F.,
 ( 4, 4 ),
 ( 0.000000000000000000, 1.000000000000000000 ),
 .UNSPECIFIED. ) ;
#55034 = ORIENTED_EDGE ( 'NONE', *, *, #59098, .T. ) ;
#55035 = CARTESIAN_POINT ( 'NONE',  ( -5.023036858974361252, -6.376774720514410077, 19.14743589743590846 ) ) ;
#55036 = CARTESIAN_POINT ( 'NONE',  ( -21.13427563780003382, 8.902639844219676135, 11.49999999999998934 ) ) ;
#55037 = CARTESIAN_POINT ( 'NONE',  ( -51.26181408848110976, -25.27420670906736078, 3.790032851153764870 ) ) ;
#55038 = CARTESIAN_POINT ( 'NONE',  ( -17.57154585214776077, 12.61476001598989782, -1.500000000000002220 ) ) ;
#55039 = CARTESIAN_POINT ( 'NONE',  ( -104.6228709571500559, -24.65952944569304961, 1.056160979905701236 ) ) ;
#55040 = CARTESIAN_POINT ( 'NONE',  ( -13.85205798638896901, 15.75786377350088507, 11.49999999999999645 ) ) ;
#55041 = VERTEX_POINT ( 'NONE', #48766 ) ;
#55042 = CARTESIAN_POINT ( 'NONE',  ( -52.62287095715005592, -29.50247984919015209, -1.443849546365058689 ) ) ;
#55043 = CARTESIAN_POINT ( 'NONE',  ( -124.5198396697245045, -24.51314013834317151, 0.6176544820404232805 ) ) ;
#55044 = CARTESIAN_POINT ( 'NONE',  ( -1.213202359833694732, 22.00568734548514627, 11.49999999999998934 ) ) ;
#55045 = VECTOR ( 'NONE', #10920, 1000.000000000000000 ) ;
#55046 = DIRECTION ( 'NONE',  ( 8.503546450866693616E-15, 0.000000000000000000, 1.000000000000000000 ) ) ;
#55047 = ORIENTED_EDGE ( 'NONE', *, *, #7716, .T. ) ;
#55048 = CARTESIAN_POINT ( 'NONE',  ( -49.79812375574695693, -25.27344795505599961, 3.459241572631841954 ) ) ;
#55049 = CARTESIAN_POINT ( 'NONE',  ( -106.6228709571500559, -23.47596703998600631, 11.44779298504227860 ) ) ;
#55050 = ORIENTED_EDGE ( 'NONE', *, *, #1627, .F. ) ;
#55051 = PLANE ( 'NONE',  #66469 ) ;
#55052 = ORIENTED_EDGE ( 'NONE', *, *, #17760, .T. ) ;
#55053 = AXIS2_PLACEMENT_3D ( 'NONE', #63683, #72282, #34217 ) ;
#55054 = ORIENTED_EDGE ( 'NONE', *, *, #51860, .T. ) ;
#55055 = EDGE_CURVE ( 'NONE', #54440, #69030, #31014, .T. ) ;
#55056 = FACE_OUTER_BOUND ( 'NONE', #81144, .T. ) ;
#55057 = DIRECTION ( 'NONE',  ( -0.000000000000000000, 1.000000000000000000, -0.000000000000000000 ) ) ;
#55058 = CARTESIAN_POINT ( 'NONE',  ( -4.213970605900704491, -6.376774720514415407, 20.02963804100705758 ) ) ;
#55059 = CARTESIAN_POINT ( 'NONE',  ( -7.302954156136775232, -19.11528491071161540, -1.500000000000002220 ) ) ;
#55060 = EDGE_LOOP ( 'NONE', ( #91851, #9797, #13613, #3177 ) ) ;
#55061 = DIRECTION ( 'NONE',  ( 0.000000000000000000, 0.000000000000000000, -1.000000000000000000 ) ) ;
#55062 = CARTESIAN_POINT ( 'NONE',  ( -10.26072176705811145, 4.666310954396869271, 28.98969649327457532 ) ) ;
#55063 = DIRECTION ( 'NONE',  ( 7.960204194457801640E-17, 1.000000000000000000, 0.000000000000000000 ) ) ;
#55064 = CARTESIAN_POINT ( 'NONE',  ( -14.60993195340527251, 16.82711592829100411, 11.49999999999998934 ) ) ;
#55065 = CARTESIAN_POINT ( 'NONE',  ( -101.6228709571500559, -24.64965695001469115, 8.947790433994178727 ) ) ;
#55066 = CARTESIAN_POINT ( 'NONE',  ( -27.61134344903479843, -24.63328469850957347, 8.250456965916750818 ) ) ;
#55067 = VERTEX_POINT ( 'NONE', #15787 ) ;
#55068 = CARTESIAN_POINT ( 'NONE',  ( -28.98875734969026396, -5.965225279485572685, 7.870022800118628759 ) ) ;
#55069 = AXIS2_PLACEMENT_3D ( 'NONE', #23224, #39966, #61818 ) ;
#55070 = CARTESIAN_POINT ( 'NONE',  ( 8.971512145086530055, -9.528487854913503696, -1.499999999999995337 ) ) ;
#55071 = ADVANCED_FACE ( 'NONE', ( #77675 ), #89313, .T. ) ;
#55072 = CIRCLE ( 'NONE', #27546, 84.48086791635431325 ) ;
#55073 = CARTESIAN_POINT ( 'NONE',  ( 0.5783248939474509021, 20.82821387695577187, -1.500000000000002220 ) ) ;
#55074 = EDGE_CURVE ( 'NONE', #23903, #40713, #49737, .T. ) ;
#55075 = ORIENTED_EDGE ( 'NONE', *, *, #95265, .T. ) ;
#55077 = ORIENTED_EDGE ( 'NONE', *, *, #29999, .T. ) ;
#55076 = CARTESIAN_POINT ( 'NONE',  ( -51.52287095715006870, -24.64898659630367206, 1.056161002820821038 ) ) ;
#55078 = VERTEX_POINT ( 'NONE', #27908 ) ;
#55079 = CIRCLE ( 'NONE', #12969, 3.349999999999998757 ) ;
#55080 = CARTESIAN_POINT ( 'NONE',  ( -51.49483116284216067, -25.12217715923064176, 6.426654410346007040 ) ) ;
#55081 = CARTESIAN_POINT ( 'NONE',  ( -7.324709186033012465, -19.69651249574825513, -1.500000000000002220 ) ) ;
#55082 = ORIENTED_EDGE ( 'NONE', *, *, #87437, .T. ) ;
#55083 = CARTESIAN_POINT ( 'NONE',  ( 6.184520403203634942, -6.376774720514426953, -25.32021290018218451 ) ) ;
#55084 = CARTESIAN_POINT ( 'NONE',  ( -53.52287095715009002, -23.72773821059537269, 11.05748984161097503 ) ) ;
#55085 = CARTESIAN_POINT ( 'NONE',  ( 7.732492002959944877, -5.356774720515376842, -27.16032169580908473 ) ) ;
#55086 = CARTESIAN_POINT ( 'NONE',  ( 29.73860345376319003, -1.477225279485574028, 19.84760796525321780 ) ) ;
#55087 = CARTESIAN_POINT ( 'NONE',  ( -119.5228709571500758, -23.48786465467241769, 11.44779295918253759 ) ) ;
#55088 = CARTESIAN_POINT ( 'NONE',  ( -64.52287095715004739, -24.50321055353805377, 9.387540953477524042 ) ) ;
#55090 = VERTEX_POINT ( 'NONE', #3094 ) ;
#55089 = CARTESIAN_POINT ( 'NONE',  ( 7.537409830304743430, 20.87355781386819942, 11.49999999999999645 ) ) ;
#55091 = EDGE_CURVE ( 'NONE', #64522, #73782, #55741, .T. ) ;
#55092 = PLANE ( 'NONE',  #32388 ) ;
#55093 = CARTESIAN_POINT ( 'NONE',  ( -38.62287095715005592, -23.96127896941631619, -0.6493128931037943641 ) ) ;
#55094 = ORIENTED_EDGE ( 'NONE', *, *, #59641, .T. ) ;
#55095 = CARTESIAN_POINT ( 'NONE',  ( -21.16080155796574047, 8.166215375980355518, -1.500000000000002220 ) ) ;
#55097 = ORIENTED_EDGE ( 'NONE', *, *, #10027, .F. ) ;
#55096 = CARTESIAN_POINT ( 'NONE',  ( -6.680782769985652791, -6.376774720514411854, 19.46295461892502132 ) ) ;
#55098 = VERTEX_POINT ( 'NONE', #87816 ) ;
#55099 = DIRECTION ( 'NONE',  ( 1.000000000000000000, 0.000000000000000000, 0.000000000000000000 ) ) ;
#55100 = CARTESIAN_POINT ( 'NONE',  ( -3.510519812331947875, -19.85243952969433323, -1.500000000000002220 ) ) ;
#55101 = DIRECTION ( 'NONE',  ( 1.000000000000000000, -0.000000000000000000, -0.000000000000000000 ) ) ;
#55102 = VERTEX_POINT ( 'NONE', #34029 ) ;
#55103 = DIRECTION ( 'NONE',  ( -3.773278334444167608E-23, 1.000000000000000000, 0.000000000000000000 ) ) ;
#55104 = CARTESIAN_POINT ( 'NONE',  ( -8.193370562272118462, -20.86776251599019361, -1.500000000000002220 ) ) ;
#55105 = ADVANCED_FACE ( 'NONE', ( #95424 ), #65251, .T. ) ;
#55106 = ORIENTED_EDGE ( 'NONE', *, *, #63217, .T. ) ;
#55107 = ORIENTED_EDGE ( 'NONE', *, *, #9452, .T. ) ;
#55108 = CARTESIAN_POINT ( 'NONE',  ( -101.1944152955115044, -25.16257438707235039, 6.858246049920544429 ) ) ;
#55109 = CARTESIAN_POINT ( 'NONE',  ( -48.62287095715004881, -24.66019654487199020, 8.947790411086135265 ) ) ;
#55110 = CARTESIAN_POINT ( 'NONE',  ( -96.58953762381672448, -23.47596703998600631, 11.44779298504227683 ) ) ;
#55111 = DIRECTION ( 'NONE',  ( 3.773278334444168195E-23, -1.000000000000000000, 0.000000000000000000 ) ) ;
#55112 = LINE ( 'NONE', #62230, #16338 ) ;
#55113 = EDGE_CURVE ( 'NONE', #47587, #85757, #94985, .T. ) ;
#55114 = CARTESIAN_POINT ( 'NONE',  ( -14.26233628608129855, 13.40890954296891024, -1.500000000000002220 ) ) ;
#55115 = CARTESIAN_POINT ( 'NONE',  ( 8.160000000000000142, -9.652339641703484574, 1.628518864987183790 ) ) ;
#55116 = ORIENTED_EDGE ( 'NONE', *, *, #3857, .F. ) ;
#55117 = CARTESIAN_POINT ( 'NONE',  ( 16.48747857468482891, 13.79107804547330929, -1.500000000000002220 ) ) ;
#55118 = CARTESIAN_POINT ( 'NONE',  ( -36.52287095715006870, -24.65952944569304606, 1.056160979905691910 ) ) ;
#55119 = CARTESIAN_POINT ( 'NONE',  ( 13.57151214508650305, 0.000000000000000000, 0.000000000000000000 ) ) ;
#55120 = CARTESIAN_POINT ( 'NONE',  ( -59.52287095715006160, -23.48783264082477018, -1.443836473390095021 ) ) ;
#55121 = AXIS2_PLACEMENT_3D ( 'NONE', #58066, #5251, #50437 ) ;
#55122 = CARTESIAN_POINT ( 'NONE',  ( -92.62287095715005592, -29.50248528299804818, 1.056150453629040253 ) ) ;
#55123 = CARTESIAN_POINT ( 'NONE',  ( -19.55383134093860420, 11.88776249338449986, -1.500000000000002220 ) ) ;
#55124 = EDGE_CURVE ( 'NONE', #71450, #63790, #7491, .T. ) ;
#55125 = EDGE_CURVE ( 'NONE', #3631, #36107, #31446, .T. ) ;
#55126 = PERSON_AND_ORGANIZATION_ROLE ( 'design_owner' ) ;
#55127 = B_SPLINE_CURVE_WITH_KNOTS ( 'NONE', 3,
 ( #97753, #29237, #14003, #90147 ),
 .UNSPECIFIED., .F., .F.,
 ( 4, 4 ),
 ( 0.000000000000000000, 0.0001000000000000028644 ),
 .UNSPECIFIED. ) ;
#55128 = DIRECTION ( 'NONE',  ( 0.000000000000000000, 0.000000000000000000, 1.000000000000000000 ) ) ;
#55129 = CARTESIAN_POINT ( 'NONE',  ( -2.599001758237162285, -5.876774720514414518, 19.60308799987317485 ) ) ;
#55130 = CARTESIAN_POINT ( 'NONE',  ( 7.608091486120485136, 18.53616061196756704, 11.49999999999999645 ) ) ;
#55131 = CARTESIAN_POINT ( 'NONE',  ( -79.92757955003747838, -25.26612385862897980, 4.561565571244288186 ) ) ;
#55132 = CARTESIAN_POINT ( 'NONE',  ( -107.5562042904834072, -24.64898659630528854, 1.056161002820829919 ) ) ;
#55133 = VECTOR ( 'NONE', #97597, 1000.000000000000000 ) ;
#55134 = CARTESIAN_POINT ( 'NONE',  ( 4.403244164709623654, -5.876774720514404748, 18.35516266052912826 ) ) ;
#55135 = PLANE ( 'NONE',  #22907 ) ;
#55136 = ORIENTED_EDGE ( 'NONE', *, *, #34116, .F. ) ;
#55137 = CARTESIAN_POINT ( 'NONE',  ( -85.62287095715009855, -24.14321612903114911, -0.2833117244521602407 ) ) ;
#55138 = VECTOR ( 'NONE', #37050, 1000.000000000000000 ) ;
#55139 = CARTESIAN_POINT ( 'NONE',  ( -20.93004649427559016, -6.003493321846349318, -1.500000000000002220 ) ) ;
#55140 = CARTESIAN_POINT ( 'NONE',  ( 15.98182857103851795, 3.492575169077971609, -27.92678846288758976 ) ) ;
#55141 = CARTESIAN_POINT ( 'NONE',  ( -18.24527198174902765, 7.358211898524878336, -1.500000000000002220 ) ) ;
#55143 = B_SPLINE_CURVE_WITH_KNOTS ( 'NONE', 3,
 ( #5884, #29224, #52568, #83501, #13986, #44963, #75888, #84003, #94615, #24097, #55571, #64196, #31720, #62183, #1775, #70288, #93602, #8883, #55066, #39325 ),
 .UNSPECIFIED., .F., .F.,
 ( 4, 2, 2, 2, 2, 2, 2, 2, 2, 4 ),
 ( 8.673617379884034509E-19, 0.0005507670852896362143, 0.001101534170579271561, 0.001652301255868906908, 0.002203068341158542255, 0.002753835426448177602, 0.003304602511737812949, 0.003855369597027447862, 0.004130753139672266837, 0.004406136682317085378 ),
 .UNSPECIFIED. ) ;
#55142 = CARTESIAN_POINT ( 'NONE',  ( -85.52287095715011844, -24.52323809116985132, 9.355190652339427260 ) ) ;
#55144 = AXIS2_PLACEMENT_3D ( 'NONE', #10539, #52106, #5422 ) ;
#55145 = CARTESIAN_POINT ( 'NONE',  ( 32.60294298177590377, -2.682774720514426559, -11.48871326860665931 ) ) ;
#55146 = ITEM_DEFINED_TRANSFORMATION ( 'NONE', 'NONE', #24482,  #37391 ) ;
#55147 = VECTOR ( 'NONE', #72030, 1000.000000000000000 ) ;
#55148 = CARTESIAN_POINT ( 'NONE',  ( -56.62287095715005592, -24.50321055353805022, 9.387540953477531147 ) ) ;
#55149 = CARTESIAN_POINT ( 'NONE',  ( -73.62287095715007013, -23.73934037231756733, 11.05740245334329153 ) ) ;
#55150 = CARTESIAN_POINT ( 'NONE',  ( -9.016818060619870678, -18.48156098877705844, 11.49999999999999645 ) ) ;
#55151 = DIRECTION ( 'NONE',  ( 0.000000000000000000, -1.000000000000000000, 0.000000000000000000 ) ) ;
#55152 = CYLINDRICAL_SURFACE ( 'NONE', #80441, 0.2500000000000011102 ) ;
#55153 = EDGE_CURVE ( 'NONE', #85265, #80623, #42160, .T. ) ;
#55154 = CIRCLE ( 'NONE', #95632, 2.040000000000000036 ) ;
#55155 = CARTESIAN_POINT ( 'NONE',  ( 11.26306171725914851, -19.60737681494043727, 11.49999999999999645 ) ) ;
#55156 = ORIENTED_EDGE ( 'NONE', *, *, #10026, .F. ) ;
#55157 = SHAPE_REPRESENTATION_RELATIONSHIP ( 'NONE' , 'NONE' ,  #44034, #7692 ) ;
#55158 = CARTESIAN_POINT ( 'NONE',  ( -70.03562343076868046, -25.25639593825284024, 7.066378759041874957 ) ) ;
#55159 = CARTESIAN_POINT ( 'NONE',  ( 25.61870917940689196, 5.965225279485572685, 29.49402280011862487 ) ) ;
#55160 = CARTESIAN_POINT ( 'NONE',  ( -125.6244067124949169, -24.52399227489127043, 9.353111116836528183 ) ) ;
#55161 = CYLINDRICAL_SURFACE ( 'NONE', #74256, 1.700000000000000178 ) ;
#55162 = EDGE_CURVE ( 'NONE', #98033, #69591, #14551, .T. ) ;
#55163 = DIRECTION ( 'NONE',  ( 0.09824042138329625029, 0.9951627101165079203, 3.504396110891627214E-15 ) ) ;
#55164 = CARTESIAN_POINT ( 'NONE',  ( -2.750773227259631692, -6.376774720514413630, 19.84584863393302001 ) ) ;
#55165 = ADVANCED_FACE ( 'NONE', ( #60868 ), #99890, .T. ) ;
#55166 = EDGE_CURVE ( 'NONE', #71187, #70309, #61369, .T. ) ;
#55167 = ORIENTED_EDGE ( 'NONE', *, *, #56423, .T. ) ;
#55168 = CARTESIAN_POINT ( 'NONE',  ( -79.71799800425125682, -25.26749921723603975, 5.176233770711395898 ) ) ;
#55169 = CARTESIAN_POINT ( 'NONE',  ( 13.81544771398824345, -18.15223324129861382, -1.500000000000002220 ) ) ;
#55170 = FACE_OUTER_BOUND ( 'NONE', #29220, .T. ) ;
#55171 = CARTESIAN_POINT ( 'NONE',  ( -115.5228709571500616, -23.47596703998600631, 11.44779298504227860 ) ) ;
#55172 = PLANE ( 'NONE',  #17677 ) ;
#55173 = CARTESIAN_POINT ( 'NONE',  ( 22.44084908143146251, -0.7541981612834567361, 11.49999999999999645 ) ) ;
#55174 = EDGE_LOOP ( 'NONE', ( #26141, #60459, #1906, #53308 ) ) ;
#55175 = CARTESIAN_POINT ( 'NONE',  ( -70.62287095715008434, -24.15516710230295416, 10.28746687063725318 ) ) ;
#55176 = CARTESIAN_POINT ( 'NONE',  ( 9.922928194174257754, 19.57116106031148561, -1.500000000000002220 ) ) ;
#55177 = CARTESIAN_POINT ( 'NONE',  ( -113.5228709571500758, -24.51283580621365488, 0.6167428607019769249 ) ) ;
#55178 = B_SPLINE_CURVE_WITH_KNOTS ( 'NONE', 3,
 ( #45573, #98836, #60303, #91227, #21704, #52676, #83613, #14098 ),
 .UNSPECIFIED., .F., .F.,
 ( 4, 2, 2, 4 ),
 ( 6.384118696468709548E-06, 0.002007151183516189211, 0.003007534715926047687, 0.004007918248335905730 ),
 .UNSPECIFIED. ) ;
#55179 = CARTESIAN_POINT ( 'NONE',  ( -44.63403588481693163, -24.35071581493542681, 9.817618358456025263 ) ) ;
#55180 = CARTESIAN_POINT ( 'NONE',  ( -56.55620429048340725, -23.48786465467241058, 11.44779295918254824 ) ) ;
#55181 = ORIENTED_EDGE ( 'NONE', *, *, #80707, .T. ) ;
#55182 = DIRECTION ( 'NONE',  ( 0.000000000000000000, -1.000000000000000000, 0.000000000000000000 ) ) ;
#55183 = CARTESIAN_POINT ( 'NONE',  ( 15.00000000000000533, 0.000000000000000000, 0.000000000000000000 ) ) ;
#55184 = ORIENTED_EDGE ( 'NONE', *, *, #95508, .T. ) ;
#55185 = CARTESIAN_POINT ( 'NONE',  ( -18.82070947631147106, 8.064391923812276985, 11.49999999999998934 ) ) ;
#55186 = VERTEX_POINT ( 'NONE', #99406 ) ;
#55187 = ORIENTED_EDGE ( 'NONE', *, *, #72679, .T. ) ;
#55188 = VERTEX_POINT ( 'NONE', #5067 ) ;
#55189 = VERTEX_POINT ( 'NONE', #92297 ) ;
#55190 = EDGE_CURVE ( 'NONE', #50489, #99448, #22269, .T. ) ;
#55191 = CARTESIAN_POINT ( 'NONE',  ( 1.912052097559287844, -22.98750448113701239, -1.500000000000002220 ) ) ;
#55192 = CARTESIAN_POINT ( 'NONE',  ( -49.61653484136814996, -25.15870442618641789, 3.051990030215718797 ) ) ;
#55193 = CARTESIAN_POINT ( 'NONE',  ( -11.05657426389776354, 17.00066307926000420, -1.500000000000002220 ) ) ;
#55194 = VERTEX_POINT ( 'NONE', #36511 ) ;
#55195 = CARTESIAN_POINT ( 'NONE',  ( 29.77147767949874790, 5.356774720514425603, 26.15915692125051706 ) ) ;
#55196 = CARTESIAN_POINT ( 'NONE',  ( 22.81105451610979173, 4.772774720514425972, -18.46691820600746681 ) ) ;
#55197 = CARTESIAN_POINT ( 'NONE',  ( -44.62287095715004881, -24.66019654487198665, 8.947790411086135265 ) ) ;
#55198 = CARTESIAN_POINT ( 'NONE',  ( 4.613443512364428400, -5.876774720514412742, 19.38647409819875733 ) ) ;
#55200 = ORIENTED_EDGE ( 'NONE', *, *, #94861, .T. ) ;
#55199 = CARTESIAN_POINT ( 'NONE',  ( -14.42888051209446409, 15.91495273949476363, 11.49999999999999645 ) ) ;
#55201 = CARTESIAN_POINT ( 'NONE',  ( -75.61136025641945935, -23.48783264082477018, -1.443836473390089914 ) ) ;
#55202 = LINE ( 'NONE', #393, #58794 ) ;
#55203 = ORIENTED_EDGE ( 'NONE', *, *, #1924, .F. ) ;
#55204 = CARTESIAN_POINT ( 'NONE',  ( -5.954758479537505700, 19.85987847461844424, -1.500000000000002220 ) ) ;
#55205 = AXIS2_PLACEMENT_3D ( 'NONE', #16992, #39332, #47457 ) ;
#55206 = EDGE_CURVE ( 'NONE', #61568, #84539, #32703, .T. ) ;
#55207 = ORIENTED_EDGE ( 'NONE', *, *, #53255, .F. ) ;
#55209 = ORIENTED_EDGE ( 'NONE', *, *, #63936, .F. ) ;
#55208 = CARTESIAN_POINT ( 'NONE',  ( -125.6257035845457750, -23.85016227208582151, -0.8807180028928047744 ) ) ;
#55210 = EDGE_CURVE ( 'NONE', #22015, #38564, #22768, .T. ) ;
#55211 = CARTESIAN_POINT ( 'NONE',  ( -111.5879331448754641, -24.51419770103157703, 9.386484678747162747 ) ) ;
#55212 = CARTESIAN_POINT ( 'NONE',  ( -129.5562042904834072, -23.47596703998600631, 11.44779298504227683 ) ) ;
#55213 = VERTEX_POINT ( 'NONE', #67982 ) ;
#55214 = ORIENTED_EDGE ( 'NONE', *, *, #33867, .T. ) ;
#55215 = CARTESIAN_POINT ( 'NONE',  ( -6.499903988472228278, -5.876774720514408301, 19.18381548539529646 ) ) ;
#55216 = CARTESIAN_POINT ( 'NONE',  ( -42.66381526571083072, -23.48786465467240347, 11.44779295918255535 ) ) ;
#55217 = CYLINDRICAL_SURFACE ( 'NONE', #57853, 10.11363636363636331 ) ;
#55218 = CARTESIAN_POINT ( 'NONE',  ( -20.87105610827876134, -7.033761084331515256, 11.49999999999999645 ) ) ;
#55219 = ADVANCED_FACE ( 'NONE', ( #53755 ), #36015, .T. ) ;
#55220 = CARTESIAN_POINT ( 'NONE',  ( -89.63160444167392882, -24.15620529776628445, 10.23563542870660115 ) ) ;
#55221 = CARTESIAN_POINT ( 'NONE',  ( -12.77507031947300042, 18.62636059118606724, -1.500000000000002220 ) ) ;
#55222 = CARTESIAN_POINT ( 'NONE',  ( -10.24336464640716216, -18.35016636821181280, 11.49999999999998934 ) ) ;
#55223 = ADVANCED_FACE ( 'NONE', ( #29900 ), #6064, .F. ) ;
#55224 = DIRECTION ( 'NONE',  ( -0.7640209514960704107, 0.000000000000000000, 0.6451914333552789538 ) ) ;
#55226 = ORIENTED_EDGE ( 'NONE', *, *, #29816, .F. ) ;
#55225 = CARTESIAN_POINT ( 'NONE',  ( -20.77875734969026311, -6.143225279485574397, 29.49402280011862487 ) ) ;
#55227 = EDGE_CURVE ( 'NONE', #50221, #5350, #4241, .T. ) ;
#55228 = CIRCLE ( 'NONE', #45507, 3.979149600822063704 ) ;
#55229 = VERTEX_POINT ( 'NONE', #67477 ) ;
#55230 = DIRECTION ( 'NONE',  ( 3.773278334444166432E-23, -1.000000000000000000, 0.000000000000000000 ) ) ;
#55231 = VECTOR ( 'NONE', #23889, 1000.000000000000000 ) ;
#55232 = DIRECTION ( 'NONE',  ( -0.1875268396392987258, -0.000000000000000000, -0.9822594791677485837 ) ) ;
#55233 = VERTEX_POINT ( 'NONE', #91302 ) ;
#55234 = CARTESIAN_POINT ( 'NONE',  ( 4.565063516603933280, 20.63981631578574039, -1.500000000000002220 ) ) ;
#55235 = CYLINDRICAL_SURFACE ( 'NONE', #88699, 2.499999999999996891 ) ;
#55236 = CARTESIAN_POINT ( 'NONE',  ( -58.86390871394272040, -25.03722704563418944, 7.590184509431679771 ) ) ;
#55237 = CARTESIAN_POINT ( 'NONE',  ( 0.000000000000000000, -6.376774720514426953, 0.000000000000000000 ) ) ;
#55238 = CARTESIAN_POINT ( 'NONE',  ( -118.5562042904833930, -23.47593901973091235, -1.443836447538997536 ) ) ;
#55239 = LINE ( 'NONE', #70954, #42192 ) ;
#55240 = CARTESIAN_POINT ( 'NONE',  ( -0.9571703918902072505, -22.19477237104690914, -1.500000000000002220 ) ) ;
#55241 = CARTESIAN_POINT ( 'NONE',  ( -81.59989503929168109, -23.73791477778912196, 11.05961554403170943 ) ) ;
#55242 = ORIENTED_EDGE ( 'NONE', *, *, #82704, .T. ) ;
#55243 = CARTESIAN_POINT ( 'NONE',  ( 14.43441819135927950, -5.965225279485592225, -28.36222020317712378 ) ) ;
#55244 = CARTESIAN_POINT ( 'NONE',  ( -37.56099248051968686, -23.73766607897670866, -1.055555164236442245 ) ) ;
#55245 = CARTESIAN_POINT ( 'NONE',  ( -126.5909412814345814, -23.48783264082477018, -1.443836473390087027 ) ) ;
#55246 = FACE_OUTER_BOUND ( 'NONE', #81717, .T. ) ;
#55247 = CARTESIAN_POINT ( 'NONE',  ( -67.52287095715006160, -29.50250786944525672, 11.44777988621623699 ) ) ;
#55248 = CARTESIAN_POINT ( 'NONE',  ( -17.65537929698502495, 8.214918384300796461, -1.500000000000002220 ) ) ;
#55249 = CARTESIAN_POINT ( 'NONE',  ( 4.431377227695222132, -20.94745169971119481, -1.500000000000002220 ) ) ;
#55250 = PLANE ( 'NONE',  #14205 ) ;
#55251 = CARTESIAN_POINT ( 'NONE',  ( -60.57813319489011405, -24.92592662360294042, 8.075495902990192931 ) ) ;
#55252 = FACE_OUTER_BOUND ( 'NONE', #73183, .T. ) ;
#55253 = CARTESIAN_POINT ( 'NONE',  ( -124.6228709571500559, -29.50250243563736774, 8.947779886222134493 ) ) ;
#55254 = CARTESIAN_POINT ( 'NONE',  ( 20.21490908150494192, 10.32750977814155391, -1.500000000000002220 ) ) ;
#55255 = LINE ( 'NONE', #61366, #23907 ) ;
#55256 = CARTESIAN_POINT ( 'NONE',  ( 7.662324775236977636, 31.59999999999999787, 0.000000000000000000 ) ) ;
#55257 = CARTESIAN_POINT ( 'NONE',  ( -1.769646468872753120, 19.80360307839763934, 11.49999999999999645 ) ) ;
#55258 = CARTESIAN_POINT ( 'NONE',  ( -123.6238837146930933, -24.51419770103158768, 9.386484678747160970 ) ) ;
#55259 = DIRECTION ( 'NONE',  ( 0.000000000000000000, 0.9999999999976377785, 2.173523156925979975E-06 ) ) ;
#55260 = CARTESIAN_POINT ( 'NONE',  ( -41.62287095715006302, -23.47596703998600276, 11.44779298504227505 ) ) ;
#55261 = EDGE_LOOP ( 'NONE', ( #90345, #89256, #85378, #57084 ) ) ;
#55262 = DIRECTION ( 'NONE',  ( 1.000000000000000000, 0.000000000000000000, -0.000000000000000000 ) ) ;
#55263 = DIRECTION ( 'NONE',  ( 0.000000000000000000, 0.9999999999976377785, 2.173523156925979128E-06 ) ) ;
#55264 = CARTESIAN_POINT ( 'NONE',  ( -51.70072539166533687, -25.27412478701024412, 3.987152057456385901 ) ) ;
#55265 = CARTESIAN_POINT ( 'NONE',  ( -21.63489631200954122, -1.325961216813365429, 11.49999999999998934 ) ) ;
#55266 = CARTESIAN_POINT ( 'NONE',  ( -56.58273429346868255, -24.51419770103157347, 9.386484678747180510 ) ) ;
#55267 = CARTESIAN_POINT ( 'NONE',  ( -7.007757480239389380, 18.17491015770016816, -1.500000000000002220 ) ) ;
#55268 = CARTESIAN_POINT ( 'NONE',  ( -61.62287095715005592, -24.33927499327855415, 9.819080762295822495 ) ) ;
#55269 = ORIENTED_EDGE ( 'NONE', *, *, #72938, .F. ) ;
#55270 = CARTESIAN_POINT ( 'NONE',  ( 20.35419724272142616, 1.316291261081859787, 11.49999999999999645 ) ) ;
#55271 = DIRECTION ( 'NONE',  ( -3.773278334453079618E-23, 0.9999999999976377785, 2.173523156925979975E-06 ) ) ;
#55272 = AXIS2_PLACEMENT_3D ( 'NONE', #61733, #16027, #63232 ) ;
#55273 = CARTESIAN_POINT ( 'NONE',  ( 8.376690734369038438, 11.49999999999999645, 2.100000000000000089 ) ) ;
#55274 = EDGE_CURVE ( 'NONE', #67048, #29423, #76558, .T. ) ;
#55275 = ORIENTED_EDGE ( 'NONE', *, *, #45606, .T. ) ;
#55276 = CARTESIAN_POINT ( 'NONE',  ( -41.46433198031985512, -25.28409534238342715, 4.125402634550018099 ) ) ;
#55277 = LINE ( 'NONE', #72002, #97935 ) ;
#55278 = CARTESIAN_POINT ( 'NONE',  ( -48.87629837916329478, -25.31602057134209360, 6.044965623264298316 ) ) ;
#55279 = FACE_OUTER_BOUND ( 'NONE', #13709, .T. ) ;
#55280 = B_SPLINE_CURVE_WITH_KNOTS ( 'NONE', 3,
 ( #5727, #3752, #36188, #82352 ),
 .UNSPECIFIED., .F., .F.,
 ( 4, 4 ),
 ( 0.000000000000000000, 9.999999999998897304E-05 ),
 .UNSPECIFIED. ) ;
#55281 = CARTESIAN_POINT ( 'NONE',  ( -0.4686347352592966087, -5.876774720514411854, 19.46274624311237034 ) ) ;
#55282 = CARTESIAN_POINT ( 'NONE',  ( 6.297820759360134524, 19.07352124001985771, 11.49999999999998934 ) ) ;
#55283 = CARTESIAN_POINT ( 'NONE',  ( -57.62287095715004881, -23.47593901973091235, -1.443836447539007972 ) ) ;
#55284 = ORIENTED_EDGE ( 'NONE', *, *, #73738, .T. ) ;
#55285 = ADVANCED_FACE ( 'NONE', ( #53253 ), #97903, .F. ) ;
#55286 = FACE_OUTER_BOUND ( 'NONE', #52173, .T. ) ;
#55287 = ADVANCED_FACE ( 'NONE', ( #37018 ), #14672, .T. ) ;
#55288 = EDGE_CURVE ( 'NONE', #84515, #16871, #27859, .T. ) ;
#55289 = AXIS2_PLACEMENT_3D ( 'NONE', #24530, #698, #53512 ) ;
#55290 = CARTESIAN_POINT ( 'NONE',  ( 7.457602374657920308, -21.66695214233757838, 11.49999999999999645 ) ) ;
#55291 = CARTESIAN_POINT ( 'NONE',  ( 11.07647423179810531, -19.82844882884714366, 11.49999999999998934 ) ) ;
#55292 = ORIENTED_EDGE ( 'NONE', *, *, #24002, .F. ) ;
#55293 = CARTESIAN_POINT ( 'NONE',  ( -30.47287095715008931, -25.29768654522517224, 5.277398094566895459 ) ) ;
#55294 = DIRECTION ( 'NONE',  ( 1.000000000000000000, 0.000000000000000000, 0.000000000000000000 ) ) ;
#55295 = CARTESIAN_POINT ( 'NONE',  ( -46.62287095715004881, -24.65952944569304250, 1.056160979905693020 ) ) ;
#55296 = EDGE_CURVE ( 'NONE', #12270, #97111, #54459, .T. ) ;
#55297 = CARTESIAN_POINT ( 'NONE',  ( -30.57287095715006942, -24.39443487893185747, 0.3225640792553110536 ) ) ;
#55298 = CARTESIAN_POINT ( 'NONE',  ( -128.5562989009644639, -23.48786465467242124, 11.44779295918253403 ) ) ;
#55299 = CARTESIAN_POINT ( 'NONE',  ( -48.87557505443476202, -25.26869748743544264, 6.071662630268244598 ) ) ;
#55300 = CARTESIAN_POINT ( 'NONE',  ( -98.89580656140421411, -25.31200720546054583, 6.002154695688947328 ) ) ;
#55301 = ORIENTED_EDGE ( 'NONE', *, *, #47825, .F. ) ;
#55302 = CARTESIAN_POINT ( 'NONE',  ( 19.80222353126469415, -4.898785079568316547, 11.49999999999998934 ) ) ;
#55303 = ORIENTED_EDGE ( 'NONE', *, *, #68054, .F. ) ;
#55304 = EDGE_CURVE ( 'NONE', #61812, #82610, #47277, .T. ) ;
#55305 = CARTESIAN_POINT ( 'NONE',  ( -22.04953120734539240, -6.464106996104416858, 11.49999999999998934 ) ) ;
#55306 = CARTESIAN_POINT ( 'NONE',  ( -1.595974963000059477, -5.876774720514407413, 19.39236848396478408 ) ) ;
#55307 = VERTEX_POINT ( 'NONE', #83179 ) ;
#55308 = CARTESIAN_POINT ( 'NONE',  ( -108.5923757939725078, -23.96169478059714208, 10.65365249895716993 ) ) ;
#55309 = EDGE_CURVE ( 'NONE', #68317, #99683, #71481, .T. ) ;
#55310 = CARTESIAN_POINT ( 'NONE',  ( -53.58734467797736301, -24.35071581493542681, 9.817618358456032368 ) ) ;
#55312 = ORIENTED_EDGE ( 'NONE', *, *, #74359, .F. ) ;
#55311 = CARTESIAN_POINT ( 'NONE',  ( -8.160016139516647726, -19.69179572373923648, 11.49999999999999645 ) ) ;
#55313 = VERTEX_POINT ( 'NONE', #47642 ) ;
#55314 = CARTESIAN_POINT ( 'NONE',  ( -2.380169663812839342, 22.11153957539610104, -1.500000000000002220 ) ) ;
#55315 = B_SPLINE_CURVE_WITH_KNOTS ( 'NONE', 3,
 ( #36201, #28090, #12844, #35704 ),
 .UNSPECIFIED., .F., .F.,
 ( 4, 4 ),
 ( 0.000000000000000000, 1.000000000000000000 ),
 .UNSPECIFIED. ) ;
#55316 = CARTESIAN_POINT ( 'NONE',  ( -12.00526669028610272, -16.82065764665920682, -1.500000000000002220 ) ) ;
#55317 = EDGE_CURVE ( 'NONE', #73668, #81696, #93191, .T. ) ;
#55318 = ORIENTED_EDGE ( 'NONE', *, *, #49118, .F. ) ;
#55319 = CARTESIAN_POINT ( 'NONE',  ( -112.6228709571500559, -23.47596703998600631, 11.44779298504227860 ) ) ;
#55320 = CARTESIAN_POINT ( 'NONE',  ( -70.79082562273967483, -25.25978459231412288, 3.590539514744167437 ) ) ;
#55321 = VERTEX_POINT ( 'NONE', #46642 ) ;
#55322 = DIRECTION ( 'NONE',  ( 0.000000000000000000, -1.000000000000000000, -0.000000000000000000 ) ) ;
#55323 = VERTEX_POINT ( 'NONE', #86687 ) ;
#55324 = CARTESIAN_POINT ( 'NONE',  ( -49.62287095715005592, -23.48783264082478084, -1.443836473390070596 ) ) ;
#55325 = CARTESIAN_POINT ( 'NONE',  ( 11.78947449592735275, 0.3587747205144256601, -28.08498176919931666 ) ) ;
#55326 = CARTESIAN_POINT ( 'NONE',  ( -20.80165436122882383, -1.723964017131293103, -1.500000000000002220 ) ) ;
#55327 = CARTESIAN_POINT ( 'NONE',  ( 21.83365961380331655, 0.8745889840297637052, 11.49999999999999645 ) ) ;
#55328 = EDGE_CURVE ( 'NONE', #82055, #64861, #1191, .T. ) ;
#55329 = CARTESIAN_POINT ( 'NONE',  ( -85.62287095715005592, -23.47596703998600631, 11.44779298504227860 ) ) ;
#55330 = CARTESIAN_POINT ( 'NONE',  ( 5.085443162053245203, -3.316774720514426456, -27.56355752155217331 ) ) ;
#55331 = CARTESIAN_POINT ( 'NONE',  ( 19.74966320730700176, -10.79507447929251107, 11.49999999999998934 ) ) ;
#55332 = B_SPLINE_CURVE_WITH_KNOTS ( 'NONE', 3,
 ( #23833, #54805, #85744, #14214 ),
 .UNSPECIFIED., .F., .F.,
 ( 4, 4 ),
 ( 1.387778780781445521E-17, 9.999999999997510880E-05 ),
 .UNSPECIFIED. ) ;
#55333 = EDGE_CURVE ( 'NONE', #12687, #3446, #52054, .T. ) ;
#55334 = DIRECTION ( 'NONE',  ( 0.000000000000000000, -1.000000000000000000, 0.000000000000000000 ) ) ;
#55335 = CARTESIAN_POINT ( 'NONE',  ( -122.5228709571500758, -23.47593901973090524, -1.443836447538996204 ) ) ;
#55336 = CARTESIAN_POINT ( 'NONE',  ( -78.55620429048340725, -23.48783264082478084, -1.443836473390064157 ) ) ;
#55337 = VERTEX_POINT ( 'NONE', #40018 ) ;
#55338 = ORIENTED_EDGE ( 'NONE', *, *, #92120, .F. ) ;
#55339 = ORIENTED_EDGE ( 'NONE', *, *, #86548, .F. ) ;
#55340 = AXIS2_PLACEMENT_3D ( 'NONE', #27679, #42425, #10442 ) ;
#55341 = ORIENTED_EDGE ( 'NONE', *, *, #47565, .T. ) ;
#55342 = CARTESIAN_POINT ( 'NONE',  ( -20.52298544035203776, 6.160189734329080125, -1.500000000000002220 ) ) ;
#55343 = CARTESIAN_POINT ( 'NONE',  ( 16.92800457317958518, -14.60656088873787262, 11.49999999999999645 ) ) ;
#55344 = ORIENTED_EDGE ( 'NONE', *, *, #13513, .T. ) ;
#55345 = CARTESIAN_POINT ( 'NONE',  ( 8.294003578737715543, -19.35633765900385939, -1.500000000000002220 ) ) ;
#55346 = CARTESIAN_POINT ( 'NONE',  ( -30.54276571906597226, -24.67129498985978131, 8.908675929220796874 ) ) ;
#55347 = CARTESIAN_POINT ( 'NONE',  ( 19.20567810191101898, 5.375360269454119155, -1.500000000000002220 ) ) ;
#55348 = CARTESIAN_POINT ( 'NONE',  ( -117.6228709571499706, -24.51283580621365132, 0.6167428607019862508 ) ) ;
#55349 = CARTESIAN_POINT ( 'NONE',  ( -43.52287095715006870, -23.73934037231756022, 11.05740245334330041 ) ) ;
#55350 = CARTESIAN_POINT ( 'NONE',  ( 7.855769811932122870, -20.56199346058834720, -1.500000000000002220 ) ) ;
#55351 = CARTESIAN_POINT ( 'NONE',  ( -17.97250661212648026, -5.965225279485594001, -23.43622901028613015 ) ) ;
#55352 = ORIENTED_EDGE ( 'NONE', *, *, #2022, .T. ) ;
#55353 = DIRECTION ( 'NONE',  ( -3.773278334453079030E-23, 0.9999999999976377785, 2.173523156925979128E-06 ) ) ;
#55354 = CARTESIAN_POINT ( 'NONE',  ( -70.62287095715005592, -23.47593901973091235, -1.443836447539006196 ) ) ;
#55355 = CARTESIAN_POINT ( 'NONE',  ( 5.313885144808909722, 20.14914662543312929, 11.49999999999999645 ) ) ;
#55356 = CARTESIAN_POINT ( 'NONE',  ( 31.60706529141451426, -4.540774720514427543, 26.12024523944107202 ) ) ;
#55357 = AXIS2_PLACEMENT_3D ( 'NONE', #42175, #80213, #87318 ) ;
#55358 = CARTESIAN_POINT ( 'NONE',  ( -108.6228709571500843, -23.96177878511308990, 10.65340807706329684 ) ) ;
#55359 = APPROVAL_PERSON_ORGANIZATION ( #90063, #39556, #20536 ) ;
#55360 = DIRECTION ( 'NONE',  ( -7.994117400814786717E-16, -0.000000000000000000, 1.000000000000000000 ) ) ;
#55361 = CARTESIAN_POINT ( 'NONE',  ( -20.61954105445765251, -5.431428859615135885, -1.500000000000002220 ) ) ;
#55362 = DIRECTION ( 'NONE',  ( 1.000000000000000000, 3.773278334444166432E-23, 8.201307841325785021E-29 ) ) ;
#55363 = CARTESIAN_POINT ( 'NONE',  ( -51.29013145356853443, -25.26457908625394566, 3.888394836251752196 ) ) ;
#55364 = FACE_OUTER_BOUND ( 'NONE', #22986, .T. ) ;
#55365 = LINE ( 'NONE', #71589, #60513 ) ;
#55366 = CARTESIAN_POINT ( 'NONE',  ( 21.68943130245101258, -6.005725296444199834, -1.500000000000002220 ) ) ;
#55367 = DIRECTION ( 'NONE',  ( -1.000000000000000000, 0.000000000000000000, -7.994117400814786717E-16 ) ) ;
#55368 = ORIENTED_EDGE ( 'NONE', *, *, #79693, .F. ) ;
#55369 = DIRECTION ( 'NONE',  ( -1.000000000000000000, -3.491481338843133355E-15, -2.352173255807796056E-16 ) ) ;
#55370 = CARTESIAN_POINT ( 'NONE',  ( -31.53769362740780480, -24.35071581493542325, 9.817618358456039473 ) ) ;
#55371 = CARTESIAN_POINT ( 'NONE',  ( -11.91260469445801995, 15.66180005371307260, 11.49999999999999645 ) ) ;
#55372 = CARTESIAN_POINT ( 'NONE',  ( -49.52287095715006160, -24.64898659630367561, 1.056161002820821038 ) ) ;
#55373 = CARTESIAN_POINT ( 'NONE',  ( -30.57287095715006231, -29.50248298729120222, -6.412432995908637812E-05 ) ) ;
#55374 = ORIENTED_EDGE ( 'NONE', *, *, #98468, .T. ) ;
#55375 = CARTESIAN_POINT ( 'NONE',  ( -99.55027089583788324, -24.34968618360934300, 0.1864209137778966852 ) ) ;
#55376 = CARTESIAN_POINT ( 'NONE',  ( -55.62287095715004170, -24.91544648472619983, 1.928969306349233470 ) ) ;
#55377 = FACE_OUTER_BOUND ( 'NONE', #21977, .T. ) ;
#55378 = DIRECTION ( 'NONE',  ( 2.352173255807804438E-16, -2.352173255807796056E-16, -1.000000000000000000 ) ) ;
#55379 = CARTESIAN_POINT ( 'NONE',  ( -0.9724026449420489771, -19.73431249065222204, 11.49999999999998934 ) ) ;
#55380 = VERTEX_POINT ( 'NONE', #54757 ) ;
#55381 = CARTESIAN_POINT ( 'NONE',  ( 17.97931717627152182, 9.192180251422895410, 11.49999999999999645 ) ) ;
#55382 = CARTESIAN_POINT ( 'NONE',  ( 10.16119454606818984, 3.316774720514931829, -28.04611093432389524 ) ) ;
#55383 = VECTOR ( 'NONE', #14135, 1000.000000000000227 ) ;
#55384 = APPROVAL_STATUS ( 'not_yet_approved' ) ;
#55385 = ORIENTED_EDGE ( 'NONE', *, *, #19224, .T. ) ;
#55386 = CARTESIAN_POINT ( 'NONE',  ( -100.5228709571500616, -24.99156044556120904, 7.747789690856173195 ) ) ;
#55387 = DIRECTION ( 'NONE',  ( 0.000000000000000000, 1.000000000000000000, 0.000000000000000000 ) ) ;
#55388 = LINE ( 'NONE', #3607, #73625 ) ;
#55389 = CARTESIAN_POINT ( 'NONE',  ( 6.420673076923079314, -6.376774720514427841, 21.83974358974358765 ) ) ;
#55390 = EDGE_CURVE ( 'NONE', #22224, #99855, #98032, .T. ) ;
#55391 = CARTESIAN_POINT ( 'NONE',  ( -67.62287095715005592, -24.64965695001468404, 8.947790433994184056 ) ) ;
#55392 = ADVANCED_FACE ( 'NONE', ( #9565 ), #39519, .T. ) ;
#55393 = DIRECTION ( 'NONE',  ( -0.7512896232465786639, -0.000000000000000000, -0.6599726524652470561 ) ) ;
#55394 = CARTESIAN_POINT ( 'NONE',  ( 17.55240489776628721, -9.587225365216566431, -1.500000000000002220 ) ) ;
#55395 = B_SPLINE_CURVE_WITH_KNOTS ( 'NONE', 3,
 ( #57275, #81588, #97307, #12058, #58745, #89696 ),
 .UNSPECIFIED., .F., .F.,
 ( 4, 2, 4 ),
 ( 0.000000000000000000, 0.001380901958385383774, 0.002761803916770767548 ),
 .UNSPECIFIED. ) ;
#55396 = EDGE_CURVE ( 'NONE', #8604, #21913, #3718, .T. ) ;
#55397 = LINE ( 'NONE', #86334, #61325 ) ;
#55398 = CARTESIAN_POINT ( 'NONE',  ( -45.62317026584761237, -23.48786465467240703, 11.44779295918255002 ) ) ;
#55399 = VERTEX_POINT ( 'NONE', #63884 ) ;
#55400 = ADVANCED_FACE ( 'NONE', ( #94798 ), #93290, .F. ) ;
#55401 = CARTESIAN_POINT ( 'NONE',  ( 26.73860345374794534, -1.477225279485574028, -1.352392034746782823 ) ) ;
#55402 = DIRECTION ( 'NONE',  ( -1.000000000000000000, 0.000000000000000000, -0.000000000000000000 ) ) ;
#55403 = CARTESIAN_POINT ( 'NONE',  ( 30.53060340732035982, 6.376774720514426953, 20.86760796525322093 ) ) ;
#55404 = CARTESIAN_POINT ( 'NONE',  ( -100.5562042904833930, -23.48786465467241769, 11.44779295918254114 ) ) ;
#55405 = B_SPLINE_CURVE_WITH_KNOTS ( 'NONE', 3,
 ( #361, #99799, #93705, #92698, #53667, #70379 ),
 .UNSPECIFIED., .F., .F.,
 ( 4, 2, 4 ),
 ( 0.000000000000000000, 0.001380901958385393315, 0.002761803916770786630 ),
 .UNSPECIFIED. ) ;
#55406 = VECTOR ( 'NONE', #63515, 1000.000000000000114 ) ;
#55407 = CARTESIAN_POINT ( 'NONE',  ( -29.49875734969025842, -5.965225279485572685, 15.62202280011862321 ) ) ;
#55408 = CARTESIAN_POINT ( 'NONE',  ( -4.700032041049139409, -6.144890974841530351, -9.000000000000000000 ) ) ;
#55409 = CARTESIAN_POINT ( 'NONE',  ( -106.6228709571500559, -23.47593901973091235, -1.443836447538999312 ) ) ;
#55410 = CARTESIAN_POINT ( 'NONE',  ( -101.9683921942802982, -25.31392319263090229, 5.203681702801227438 ) ) ;
#55411 = ORIENTED_EDGE ( 'NONE', *, *, #41584, .F. ) ;
#55412 = CARTESIAN_POINT ( 'NONE',  ( 2.303441031721801480, -20.17751241584783628, 11.49999999999998934 ) ) ;
#55413 = CARTESIAN_POINT ( 'NONE',  ( -39.56136241089613037, -29.50249502162446902, 5.536722193922502200 ) ) ;
#55414 = CARTESIAN_POINT ( 'NONE',  ( 32.59332756141814258, 1.682774720514426114, -11.41404606144462797 ) ) ;
#55415 = ORIENTED_EDGE ( 'NONE', *, *, #30052, .T. ) ;
#55416 = B_SPLINE_CURVE_WITH_KNOTS ( 'NONE', 3,
 ( #9444, #24658, #77439, #40403 ),
 .UNSPECIFIED., .F., .F.,
 ( 4, 4 ),
 ( 0.08881981938298308399, 0.08982056642374858235 ),
 .UNSPECIFIED. ) ;
#55417 = CARTESIAN_POINT ( 'NONE',  ( -81.62287095715005592, -23.48783264082478794, -1.443836473390065711 ) ) ;
#55418 = VECTOR ( 'NONE', #86290, 1000.000000000000000 ) ;
#55419 = CARTESIAN_POINT ( 'NONE',  ( 15.40757771627215256, 13.04930689719894765, -1.500000000000002220 ) ) ;
#55420 = CARTESIAN_POINT ( 'NONE',  ( 6.572693220633653688, -20.11273663914708365, 11.49999999999999645 ) ) ;
#55421 = PRODUCT_DEFINITION_FORMATION_WITH_SPECIFIED_SOURCE ( 'ANY', '', #44230, .NOT_KNOWN. ) ;
#55422 = CARTESIAN_POINT ( 'NONE',  ( 18.07010470096111021, 12.80550835427630574, -1.500000000000002220 ) ) ;
#55423 = CARTESIAN_POINT ( 'NONE',  ( 0.1292827521129817636, -20.55975067039486603, -1.500000000000002220 ) ) ;
#55424 = CARTESIAN_POINT ( 'NONE',  ( -116.6228709571500559, -24.64898659630368627, 1.056161002820833028 ) ) ;
#55425 = ORIENTED_EDGE ( 'NONE', *, *, #29941, .T. ) ;
#55426 = LINE ( 'NONE', #47808, #97682 ) ;
#55427 = ORIENTED_EDGE ( 'NONE', *, *, #47154, .T. ) ;
#55428 = FACE_OUTER_BOUND ( 'NONE', #13865, .T. ) ;
#55429 = CARTESIAN_POINT ( 'NONE',  ( -70.52287095715009002, -24.14406661686762945, 10.28769366194079282 ) ) ;
#55430 = ORIENTED_EDGE ( 'NONE', *, *, #42201, .T. ) ;
#55431 = VERTEX_POINT ( 'NONE', #1467 ) ;
#55432 = ORIENTED_EDGE ( 'NONE', *, *, #100352, .T. ) ;
#55433 = DIRECTION ( 'NONE',  ( 0.000000000000000000, -0.000000000000000000, -1.000000000000000000 ) ) ;
#55434 = DIRECTION ( 'NONE',  ( 0.000000000000000000, 0.9999999999976377785, 2.173523156925979975E-06 ) ) ;
#55435 = CARTESIAN_POINT ( 'NONE',  ( 0.2885822020289898759, -6.376774720514415407, 19.94806476610988710 ) ) ;
#55436 = CARTESIAN_POINT ( 'NONE',  ( -18.06733440434376092, 10.15830956056102963, -1.500000000000002220 ) ) ;
#55437 = CARTESIAN_POINT ( 'NONE',  ( -15.83346750871019992, -14.79491179806518630, 11.49999999999999645 ) ) ;
#55438 = EDGE_LOOP ( 'NONE', ( #41227, #88296, #98107, #76387 ) ) ;
#55439 = CARTESIAN_POINT ( 'NONE',  ( -100.5895376238167387, -23.47596703998600631, 11.44779298504227683 ) ) ;
#55440 = DIRECTION ( 'NONE',  ( -0.000000000000000000, 1.000000000000000000, -0.000000000000000000 ) ) ;
#55441 = CARTESIAN_POINT ( 'NONE',  ( -18.60458529277170214, -12.42720982490441095, -1.500000000000002220 ) ) ;
#55442 = EDGE_CURVE ( 'NONE', #3403, #63553, #37486, .T. ) ;
#55443 = CARTESIAN_POINT ( 'NONE',  ( -47.48415699084505803, -24.66019654487199730, 8.947790411086117501 ) ) ;
#55444 = CARTESIAN_POINT ( 'NONE',  ( -75.22287095715006444, -23.47596703998600631, 11.44779298504227860 ) ) ;
#55445 = VERTEX_POINT ( 'NONE', #31404 ) ;
#55446 = CARTESIAN_POINT ( 'NONE',  ( -118.7286108204959163, -25.33572373775064790, 6.311492575451646658 ) ) ;
#55447 = CARTESIAN_POINT ( 'NONE',  ( -35.58475201036861080, -24.63419186844611986, 9.035850630976925757 ) ) ;
#55448 = ORIENTED_EDGE ( 'NONE', *, *, #93635, .T. ) ;
#55449 = EDGE_CURVE ( 'NONE', #1269, #991, #75035, .T. ) ;
#55450 = CARTESIAN_POINT ( 'NONE',  ( -45.52287095715006160, -24.91570333825768913, 8.075032458260363200 ) ) ;
#55451 = ORIENTED_EDGE ( 'NONE', *, *, #77896, .T. ) ;
#55452 = VECTOR ( 'NONE', #56234, 1000.000000000000114 ) ;
#55453 = CARTESIAN_POINT ( 'NONE',  ( -100.6228709571500701, -23.47596703998600631, 11.44779298504227860 ) ) ;
#55454 = CARTESIAN_POINT ( 'NONE',  ( 3.105769797727405024, 20.95935918496786599, -1.500000000000002220 ) ) ;
#55455 = B_SPLINE_CURVE_WITH_KNOTS ( 'NONE', 3,
 ( #80299, #50859, #58475, #81796, #95523, #33629 ),
 .UNSPECIFIED., .F., .F.,
 ( 4, 2, 4 ),
 ( 0.000000000000000000, 0.001380901958385388545, 0.002761803916770777089 ),
 .UNSPECIFIED. ) ;
#55456 = ORIENTED_EDGE ( 'NONE', *, *, #72142, .F. ) ;
#55457 = CARTESIAN_POINT ( 'NONE',  ( -50.52198866362500240, -23.48783264082477018, -1.443836473390096797 ) ) ;
#55458 = CARTESIAN_POINT ( 'NONE',  ( -19.95566455537076678, 8.849265345510103131, -1.500000000000002220 ) ) ;
#55459 = DIRECTION ( 'NONE',  ( 3.773278334444167608E-23, -1.000000000000000000, 0.000000000000000000 ) ) ;
#55460 = B_SPLINE_CURVE_WITH_KNOTS ( 'NONE', 3,
 ( #99341, #83622, #21709, #52683 ),
 .UNSPECIFIED., .F., .F.,
 ( 4, 4 ),
 ( 0.02051464900870706917, 0.02952108028082290475 ),
 .UNSPECIFIED. ) ;
#55461 = CARTESIAN_POINT ( 'NONE',  ( -62.55620429048339304, -24.66019654487199020, 8.947790411086131712 ) ) ;
#55462 = DIRECTION ( 'NONE',  ( 1.000000000000000000, 0.000000000000000000, 0.000000000000000000 ) ) ;
#55463 = CARTESIAN_POINT ( 'NONE',  ( -6.457742198559264679, -20.83860622980983024, -1.500000000000002220 ) ) ;
#55464 = CARTESIAN_POINT ( 'NONE',  ( -1.304987980769231948, -6.376774720514413630, 19.76512419871795245 ) ) ;
#55465 = VERTEX_POINT ( 'NONE', #46136 ) ;
#55466 = CARTESIAN_POINT ( 'NONE',  ( -41.62287095715007723, -24.50216790748204687, 0.6166512839542525048 ) ) ;
#55467 = CARTESIAN_POINT ( 'NONE',  ( -48.87380231474225667, -25.12782503098429743, 6.137092279293525188 ) ) ;
#55468 = VERTEX_POINT ( 'NONE', #69466 ) ;
#55469 = CARTESIAN_POINT ( 'NONE',  ( -129.5222683580481089, -23.48786465467241769, 11.44779295918253759 ) ) ;
#55470 = ORIENTED_EDGE ( 'NONE', *, *, #99672, .T. ) ;
#55471 = ORIENTED_EDGE ( 'NONE', *, *, #31686, .T. ) ;
#55472 = AXIS2_PLACEMENT_3D ( 'NONE', #38031, #90822, #90322 ) ;
#55473 = DIRECTION ( 'NONE',  ( -3.773278334453079030E-23, 0.9999999999976377785, 2.173523156925979128E-06 ) ) ;
#55474 = CARTESIAN_POINT ( 'NONE',  ( -113.6228709571500559, -24.65952944569304961, 1.056160979905706565 ) ) ;
#55475 = CARTESIAN_POINT ( 'NONE',  ( 1.624102159173431259, 21.17561035156254334, -1.500000000000002220 ) ) ;
#55476 = AXIS2_PLACEMENT_3D ( 'NONE', #2486, #11088, #73002 ) ;
#55477 = DIRECTION ( 'NONE',  ( -0.000000000000000000, 1.000000000000000000, -0.000000000000000000 ) ) ;
#55478 = CARTESIAN_POINT ( 'NONE',  ( -41.55620429048340014, -24.65952944569304606, 1.056160979905691910 ) ) ;
#55479 = CARTESIAN_POINT ( 'NONE',  ( 8.071512145086499501, -1.028487854913504362, 3.749999999999999556 ) ) ;
#55480 = CARTESIAN_POINT ( 'NONE',  ( -127.5895376238166961, -24.66019654487200086, 8.947790411086117501 ) ) ;
#55481 = CARTESIAN_POINT ( 'NONE',  ( 8.513215801882951794, -17.43586836189350819, 11.49999999999998934 ) ) ;
#55482 = CARTESIAN_POINT ( 'NONE',  ( -117.5893256543061653, -24.35071581493544457, 9.817618358456019934 ) ) ;
#55483 = ORIENTED_EDGE ( 'NONE', *, *, #95316, .F. ) ;
#55484 = CARTESIAN_POINT ( 'NONE',  ( -12.10551386448753064, 15.32171617432465816, 11.49999999999999645 ) ) ;
#55485 = FACE_OUTER_BOUND ( 'NONE', #64006, .T. ) ;
#55486 = CARTESIAN_POINT ( 'NONE',  ( -79.39961074542060260, -25.23283802384501584, 6.332283618388551361 ) ) ;
#55487 = ORIENTED_EDGE ( 'NONE', *, *, #49097, .T. ) ;
#55488 = CARTESIAN_POINT ( 'NONE',  ( -98.62287095715005592, -24.66019654487199730, 8.947790411086124607 ) ) ;
#55489 = CARTESIAN_POINT ( 'NONE',  ( -89.54581868124135724, -24.51314013834317862, 0.6176544820404262781 ) ) ;
#55490 = FACE_OUTER_BOUND ( 'NONE', #76485, .T. ) ;
#55491 = AXIS2_PLACEMENT_3D ( 'NONE', #55617, #86546, #78923 ) ;
#55492 = FACE_OUTER_BOUND ( 'NONE', #47773, .T. ) ;
#55493 = CARTESIAN_POINT ( 'NONE',  ( -16.89733858281218204, -10.06102416988892934, -1.500000000000002220 ) ) ;
#55495 = ORIENTED_EDGE ( 'NONE', *, *, #72984, .F. ) ;
#55494 = LOCAL_TIME ( 0, 54, 15.00000000000000000, #70598 ) ;
#55496 = CARTESIAN_POINT ( 'NONE',  ( 20.55510029441247610, -6.647428040031946317, -1.500000000000002220 ) ) ;
#55497 = B_SPLINE_CURVE_WITH_KNOTS ( 'NONE', 3,
 ( #24995, #62079, #93003, #54965 ),
 .UNSPECIFIED., .F., .F.,
 ( 4, 4 ),
 ( 0.000000000000000000, 8.007323677445510822E-05 ),
 .UNSPECIFIED. ) ;
#55498 = CARTESIAN_POINT ( 'NONE',  ( -100.6814946224345846, -29.50249428492551829, 5.197779886230994073 ) ) ;
#55500 = B_SPLINE_CURVE_WITH_KNOTS ( 'NONE', 3,
 ( #82804, #51373, #75192, #5686, #12790, #43760, #59992, #45258, #29516, #74693, #75685, #5188, #21891, #76184, #36636, #36145, #6683, #67604, #98522, #68592, #90924, #83303 ),
 .UNSPECIFIED., .F., .F.,
 ( 4, 2, 2, 2, 2, 2, 2, 2, 2, 2, 4 ),
 ( 0.000000000000000000, 0.0002773043728616134650, 0.0005546087457232269299, 0.0008319131185848405033, 0.001109217491446453860, 0.001663826237169669514, 0.002218434982892885168, 0.002773043728616100823, 0.003327652474339316043, 0.003882261220062532131, 0.004436869965785747785 ),
 .UNSPECIFIED. ) ;
#55499 = CARTESIAN_POINT ( 'NONE',  ( -0.02075734969026423599, -3.316774720514426456, -0.08597719988137648983 ) ) ;
#55501 = CARTESIAN_POINT ( 'NONE',  ( 11.75533340255842596, 19.88161105567325038, -1.500000000000002220 ) ) ;
#55502 = CIRCLE ( 'NONE', #7106, 1.325999999999990298 ) ;
#55503 = APPROVAL_DATE_TIME ( #95554, #88468 ) ;
#55504 = CARTESIAN_POINT ( 'NONE',  ( 3.362030615038681169, -6.376774720514424288, 21.34376340489846413 ) ) ;
#55505 = DIRECTION ( 'NONE',  ( -3.773278334444166432E-23, 1.000000000000000000, 0.000000000000000000 ) ) ;
#55506 = DIRECTION ( 'NONE',  ( 0.000000000000000000, -0.000000000000000000, -1.000000000000000000 ) ) ;
#55507 = DIRECTION ( 'NONE',  ( -0.000000000000000000, -1.000000000000000000, -0.000000000000000000 ) ) ;
#55508 = ADVANCED_FACE ( 'NONE', ( #30900 ), #94354, .T. ) ;
#55509 = CARTESIAN_POINT ( 'NONE',  ( -110.7466941838547143, -25.10921386403298072, 2.889691385203864371 ) ) ;
#55510 = CARTESIAN_POINT ( 'NONE',  ( -121.6228709571500985, -24.35013146730204525, 9.818937971375104823 ) ) ;
#55511 = AXIS2_PLACEMENT_3D ( 'NONE', #32366, #32876, #63341 ) ;
#55512 = CARTESIAN_POINT ( 'NONE',  ( -114.5520155267526832, -24.51419770103158768, 9.386484678747160970 ) ) ;
#55513 = CARTESIAN_POINT ( 'NONE',  ( -18.69216024341242743, -6.879743215651725308, 11.49999999999998934 ) ) ;
#55514 = EDGE_CURVE ( 'NONE', #18750, #85588, #83485, .T. ) ;
#55515 = B_SPLINE_CURVE_WITH_KNOTS ( 'NONE', 3,
 ( #48018, #100261, #8942, #70851, #9943, #71354 ),
 .UNSPECIFIED., .F., .F.,
 ( 4, 2, 4 ),
 ( 0.001468967764902712192, 0.004864447352129883453, 0.008259926939357054715 ),
 .UNSPECIFIED. ) ;
#55516 = CARTESIAN_POINT ( 'NONE',  ( -75.60360349675073621, -23.85049219812685806, 10.88485053497527488 ) ) ;
#55517 = CARTESIAN_POINT ( 'NONE',  ( 4.164567180745167185, 19.39263604865329071, -1.500000000000002220 ) ) ;
#55518 = VERTEX_POINT ( 'NONE', #11556 ) ;
#55519 = CARTESIAN_POINT ( 'NONE',  ( -71.62287095715005592, -23.47593901973091235, -1.443836447539006196 ) ) ;
#55520 = EDGE_CURVE ( 'NONE', #69268, #2927, #79576, .T. ) ;
#55521 = EDGE_CURVE ( 'NONE', #5872, #31685, #43025, .T. ) ;
#55522 = CARTESIAN_POINT ( 'NONE',  ( -39.14342005660770241, -25.10925777441851992, 3.683763713153402897 ) ) ;
#55523 = DIRECTION ( 'NONE',  ( -3.773278334453079030E-23, 0.9999999999976377785, 2.173523156925979128E-06 ) ) ;
#55524 = CARTESIAN_POINT ( 'NONE',  ( 1.902724757927627408, 20.64897553884969028, 11.49999999999999645 ) ) ;
#55525 = DIRECTION ( 'NONE',  ( -1.000000000000000000, 0.000000000000000000, 2.338552693767719605E-15 ) ) ;
#55526 = EDGE_CURVE ( 'NONE', #24485, #48999, #60340, .T. ) ;
#55527 = PLANE ( 'NONE',  #11708 ) ;
#55528 = CARTESIAN_POINT ( 'NONE',  ( -18.67006117854901959, 13.05921059288911934, 11.49999999999999645 ) ) ;
#55529 = VECTOR ( 'NONE', #57495, 1000.000000000000114 ) ;
#55530 = VERTEX_POINT ( 'NONE', #25792 ) ;
#55531 = B_SPLINE_SURFACE_WITH_KNOTS ( 'NONE', 3, 3, ( 
 ( #40384, #71336, #85545, #77420 ),
 ( #79433, #8923, #1826, #48505 ),
 ( #314, #46994, #39377, #31258 ),
 ( #9924, #7923, #78426, #38871 ),
 ( #77917, #39876, #814, #31767 ),
 ( #62736, #93652, #1326, #71838 ),
 ( #35277, #40879, #66241, #87554 ),
 ( #25651, #50009, #88061, #42403 ),
 ( #19034, #2330, #81447, #50494 ),
 ( #3830, #58607, #96662, #18039 ),
 ( #64245, #88560, #33259, #65741 ),
 ( #96173, #72341, #56625, #80943 ),
 ( #27158, #97167, #11428, #34276 ),
 ( #4327, #79935, #95167, #41898 ),
 ( #58122, #72841, #81936, #2833 ),
 ( #33770, #49004, #10423, #41385 ),
 ( #65249, #27661, #26659, #64752 ),
 ( #11926, #57620, #89059, #42890 ),
 ( #73826, #73337, #89553, #19532 ),
 ( #20037, #95669, #51001, #26151 ),
 ( #57125, #34771, #18538, #49506 ),
 ( #80442, #10931, #3340, #35772 ),
 ( #98645, #30136, #51993, #6310 ),
 ( #92038, #22010, #52493, #66741 ),
 ( #59114, #29144, #52999, #75808 ) ),
 .UNSPECIFIED., .F., .F., .F.,
 ( 4, 3, 3, 3, 3, 3, 3, 3, 4 ),
 ( 4, 4 ),
 ( -7.445425705058654331E-16, 0.1249999999999994726, 0.1874999999999995837, 0.2499999999999996947, 0.5000000000000001110, 0.7500000000000004441, 0.8125000000000005551, 0.8750000000000006661, 1.000000000000000888 ),
 ( 0.000000000000000000, 1.000000000000000000 ),
 .UNSPECIFIED. ) ;
#55532 = CARTESIAN_POINT ( 'NONE',  ( -69.55396335837851041, -23.96119346886880663, -0.6495511937832122440 ) ) ;
#55533 = DIRECTION ( 'NONE',  ( 0.000000000000000000, 0.000000000000000000, 1.000000000000000000 ) ) ;
#55534 = VERTEX_POINT ( 'NONE', #88200 ) ;
#55535 = CARTESIAN_POINT ( 'NONE',  ( -0.5548696950099620828, -20.20177982057877841, 11.49999999999998934 ) ) ;
#55536 = EDGE_CURVE ( 'NONE', #36349, #93143, #10067, .T. ) ;
#55537 = CYLINDRICAL_SURFACE ( 'NONE', #45165, 5.000000000000001776 ) ;
#55538 = CYLINDRICAL_SURFACE ( 'NONE', #60966, 2.500000000000000444 ) ;
#55539 = EDGE_LOOP ( 'NONE', ( #26500, #31639, #15567, #64735 ) ) ;
#55540 = CARTESIAN_POINT ( 'NONE',  ( -0.1490770655183801252, -21.12008023607309681, -1.443836447538997758 ) ) ;
#55541 = CARTESIAN_POINT ( 'NONE',  ( 5.768980952343642166, -22.17701263744951490, -1.500000000000002220 ) ) ;
#55542 = CARTESIAN_POINT ( 'NONE',  ( -100.6228709571500559, -24.99132157543167310, 2.256160258750667502 ) ) ;
#55543 = CARTESIAN_POINT ( 'NONE',  ( -19.89792590360708147, -2.209704250470923892, -1.500000000000002220 ) ) ;
#55544 = DIRECTION ( 'NONE',  ( -0.000000000000000000, 1.000000000000000000, -0.000000000000000000 ) ) ;
#55545 = AXIS2_PLACEMENT_3D ( 'NONE', #51014, #33782, #88077 ) ;
#55546 = CARTESIAN_POINT ( 'NONE',  ( 0.9685562702117149758, 20.96446713366763248, 11.49999999999999645 ) ) ;
#55547 = DIRECTION ( 'NONE',  ( 4.835261319396784738E-10, 0.000000000000000000, -1.000000000000000000 ) ) ;
#55548 = CARTESIAN_POINT ( 'NONE',  ( -69.03429854110324015, -25.24754422676405241, 5.665244721077478118 ) ) ;
#55549 = CARTESIAN_POINT ( 'NONE',  ( -10.85839155550747392, 19.17434714687634667, 11.49999999999998934 ) ) ;
#55550 = CARTESIAN_POINT ( 'NONE',  ( -101.9228709571500815, -23.47593901973090524, -1.443836447538996870 ) ) ;
#55551 = ORIENTED_EDGE ( 'NONE', *, *, #91533, .F. ) ;
#55552 = CARTESIAN_POINT ( 'NONE',  ( -2.814730745656462307, 14.91141199530731853, 8.673617379884035472E-16 ) ) ;
#55553 = FACE_OUTER_BOUND ( 'NONE', #38862, .T. ) ;
#55554 = ORIENTED_EDGE ( 'NONE', *, *, #35448, .T. ) ;
#55555 = DIRECTION ( 'NONE',  ( 0.000000000000000000, -0.9999999999976377785, -2.173523156925979975E-06 ) ) ;
#55556 = ORIENTED_EDGE ( 'NONE', *, *, #38762, .T. ) ;
#55557 = VERTEX_POINT ( 'NONE', #96802 ) ;
#55558 = CARTESIAN_POINT ( 'NONE',  ( -118.6228709571500559, -24.66019654487200086, 8.947790411086117501 ) ) ;
#55559 = DIRECTION ( 'NONE',  ( 0.1311553622875919756, 0.000000000000000000, 0.9913618264504692190 ) ) ;
#55560 = CARTESIAN_POINT ( 'NONE',  ( -4.152941208099351300, -6.376774720514415407, 20.35309744218305639 ) ) ;
#55561 = CARTESIAN_POINT ( 'NONE',  ( 18.12345787009687115, -9.690629616749632191, -1.500000000000002220 ) ) ;
#55562 = EDGE_CURVE ( 'NONE', #33349, #51268, #33898, .T. ) ;
#55563 = ORIENTED_EDGE ( 'NONE', *, *, #11803, .F. ) ;
#55564 = CARTESIAN_POINT ( 'NONE',  ( -100.5246099931740105, -25.30387691067383926, 5.206566059064181573 ) ) ;
#55565 = DIRECTION ( 'NONE',  ( -0.9997753877537052247, 0.000000000000000000, 0.02119372647573814633 ) ) ;
#55566 = PLANE ( 'NONE',  #36968 ) ;
#55567 = CARTESIAN_POINT ( 'NONE',  ( -21.97457344801873447, 3.670769625195870134, -1.500000000000002220 ) ) ;
#55568 = ADVANCED_FACE ( 'NONE', ( #3965 ), #72479, .F. ) ;
#55570 = CARTESIAN_POINT ( 'NONE',  ( -80.52287095715006160, -23.47596703998600631, 11.44779298504228571 ) ) ;
#55569 = AXIS2_PLACEMENT_3D ( 'NONE', #88204, #49158, #26796 ) ;
#55571 = CARTESIAN_POINT ( 'NONE',  ( -26.11966125959963847, -24.71873968571609836, 7.419517041710707694 ) ) ;
#55572 = ORIENTED_EDGE ( 'NONE', *, *, #54572, .T. ) ;
#55573 = CARTESIAN_POINT ( 'NONE',  ( -29.81066356762512726, -25.24533126392478266, 4.756803792137969999 ) ) ;
#55574 = LINE ( 'NONE', #93605, #5332 ) ;
#55575 = CC_DESIGN_APPROVAL ( #76640, ( #66951 ) ) ;
#55576 = CARTESIAN_POINT ( 'NONE',  ( -12.81329989551134751, 16.42372500408851366, 11.49999999999998934 ) ) ;
#55577 = ORIENTED_EDGE ( 'NONE', *, *, #15111, .T. ) ;
#55579 = ORIENTED_EDGE ( 'NONE', *, *, #47520, .T. ) ;
#55578 = LINE ( 'NONE', #86508, #23103 ) ;
#55580 = ORIENTED_EDGE ( 'NONE', *, *, #57989, .F. ) ;
#55581 = VECTOR ( 'NONE', #85570, 1000.000000000000227 ) ;
#55582 = CARTESIAN_POINT ( 'NONE',  ( 10.24059822343757808, -6.376774720514426953, 17.17691942396160698 ) ) ;
#55583 = CARTESIAN_POINT ( 'NONE',  ( 16.07406896385161943, -13.52096256729613266, -1.500000000000002220 ) ) ;
#55584 = EDGE_CURVE ( 'NONE', #56477, #51806, #27787, .T. ) ;
#55585 = VERTEX_POINT ( 'NONE', #50137 ) ;
#55586 = CARTESIAN_POINT ( 'NONE',  ( -110.6228709571500417, -24.14321612903117753, -0.2833117244520985123 ) ) ;
#55587 = CARTESIAN_POINT ( 'NONE',  ( -49.74369414166532266, -25.30543060587212167, 4.940877950953177944 ) ) ;
#55588 = CARTESIAN_POINT ( 'NONE',  ( 8.720390671794367776, -5.356774720513354460, -27.07197491334870065 ) ) ;
#55589 = VECTOR ( 'NONE', #49093, 1000.000000000000000 ) ;
#55590 = CARTESIAN_POINT ( 'NONE',  ( -101.4365978186105366, -25.25419481222983720, 7.227288580716594524 ) ) ;
#55591 = CARTESIAN_POINT ( 'NONE',  ( -66.52287095715006160, -29.50248528299804818, 1.056150453629036701 ) ) ;
#55592 = DIRECTION ( 'NONE',  ( 0.000000000000000000, 2.173523156925980399E-06, -0.9999999999976378895 ) ) ;
#55594 = ORIENTED_EDGE ( 'NONE', *, *, #24222, .T. ) ;
#55593 = CARTESIAN_POINT ( 'NONE',  ( -20.66209241242137296, -8.185968977665980972, 11.49999999999999645 ) ) ;
#55595 = DIRECTION ( 'NONE',  ( -0.9890158633619159367, -0.1478094111296165969, 0.000000000000000000 ) ) ;
#55596 = ADVANCED_FACE ( 'NONE', ( #80576 ), #49850, .T. ) ;
#55597 = DIRECTION ( 'NONE',  ( -3.773278334453080206E-23, 0.9999999999976377785, 2.173523156925979975E-06 ) ) ;
#55598 = VERTEX_POINT ( 'NONE', #82075 ) ;
#55599 = CARTESIAN_POINT ( 'NONE',  ( 16.59953334139655468, -15.42474913338910980, -1.500000000000002220 ) ) ;
#55601 = ORIENTED_EDGE ( 'NONE', *, *, #87319, .F. ) ;
#55600 = CARTESIAN_POINT ( 'NONE',  ( -76.62287095715002749, -24.33832256526968507, 0.1851278514119898688 ) ) ;
#55602 = ORIENTED_EDGE ( 'NONE', *, *, #7194, .F. ) ;
#55603 = CARTESIAN_POINT ( 'NONE',  ( 9.552245033349362461E-16, 23.99999999999999645, 2.100000000000000089 ) ) ;
#55604 = B_SPLINE_CURVE_WITH_KNOTS ( 'NONE', 3,
 ( #93438, #24934, #55404, #69623 ),
 .UNSPECIFIED., .F., .F.,
 ( 4, 4 ),
 ( 0.000000000000000000, 9.999999999998897304E-05 ),
 .UNSPECIFIED. ) ;
#55605 = CC_DESIGN_PERSON_AND_ORGANIZATION_ASSIGNMENT ( #43037, #75451, ( #16578 ) ) ;
#55606 = CARTESIAN_POINT ( 'NONE',  ( 16.24926901856429140, 11.90123039513101411, -1.500000000000002220 ) ) ;
#55607 = CARTESIAN_POINT ( 'NONE',  ( -9.383883476483159569, 17.86611652351680846, 2.100000000000000089 ) ) ;
#55608 = ORIENTED_EDGE ( 'NONE', *, *, #59809, .T. ) ;
#55610 = CARTESIAN_POINT ( 'NONE',  ( -87.52287095715006160, -29.50250243563736774, 8.947779886222139822 ) ) ;
#55609 = SHAPE_REPRESENTATION ( 'Spool_Varsay\X2\0131\X0\lan', ( #37391 ), #45585 ) ;
#55611 = CARTESIAN_POINT ( 'NONE',  ( -3.695635658436464244, 22.08213133993951161, -1.500000000000002220 ) ) ;
#55612 = ORIENTED_EDGE ( 'NONE', *, *, #13559, .F. ) ;
#55613 = ORIENTED_EDGE ( 'NONE', *, *, #67213, .F. ) ;
#55614 = DIRECTION ( 'NONE',  ( -0.000000000000000000, 0.000000000000000000, -1.000000000000000000 ) ) ;
#55616 = CARTESIAN_POINT ( 'NONE',  ( -94.51279141762005054, -24.15620529776628089, 10.23563542870660470 ) ) ;
#55615 = AXIS2_PLACEMENT_3D ( 'NONE', #33847, #78504, #32851 ) ;
#55617 = CARTESIAN_POINT ( 'NONE',  ( -10.34999999999999254, -1.267509437117509414E-15, 2.100000000000000089 ) ) ;
#55618 = PLANE ( 'NONE',  #43315 ) ;
#55619 = CARTESIAN_POINT ( 'NONE',  ( -10.34999999999997833, 27.69999999999999929, 2.100000000000000089 ) ) ;
#55620 = B_SPLINE_CURVE_WITH_KNOTS ( 'NONE', 3,
 ( #14913, #45887, #76802, #49281 ),
 .UNSPECIFIED., .F., .F.,
 ( 4, 4 ),
 ( 0.4300930433922509066, 0.4390994746643664959 ),
 .UNSPECIFIED. ) ;
#55621 = CARTESIAN_POINT ( 'NONE',  ( 7.829539893445508270, 17.95258299782629408, -1.500000000000002220 ) ) ;
#55622 = AXIS2_PLACEMENT_3D ( 'NONE', #32294, #8459, #77946 ) ;
#55623 = CARTESIAN_POINT ( 'NONE',  ( -5.596556251055551101, -5.876774720514411854, 19.35667676486397681 ) ) ;
#55624 = ORIENTED_EDGE ( 'NONE', *, *, #73786, .F. ) ;
#55625 = CARTESIAN_POINT ( 'NONE',  ( 2.564635614221720594, -21.35862533600356983, 11.49999999999998934 ) ) ;
#55626 = CARTESIAN_POINT ( 'NONE',  ( -128.5898165004505813, -24.15543982623908548, -0.2315651400026392803 ) ) ;
#55627 = DIRECTION ( 'NONE',  ( 0.000000000000000000, 0.000000000000000000, 1.000000000000000000 ) ) ;
#55628 = DIRECTION ( 'NONE',  ( 0.000000000000000000, -0.000000000000000000, -1.000000000000000000 ) ) ;
#55629 = CARTESIAN_POINT ( 'NONE',  ( -111.6228709571500843, -24.34917612406838572, 0.1852690917426694506 ) ) ;
#55630 = CARTESIAN_POINT ( 'NONE',  ( 10.67403711042701353, -20.27515232684288549, -1.500000000000002220 ) ) ;
#55631 = DATE_AND_TIME ( #24651, #34280 ) ;
#55632 = CARTESIAN_POINT ( 'NONE',  ( -92.52287095715006160, -23.47593901973090169, -1.443836447538996426 ) ) ;
#55633 = CARTESIAN_POINT ( 'NONE',  ( -53.61318609310688288, -23.48783264082475952, -1.443836473390095909 ) ) ;
#55634 = CARTESIAN_POINT ( 'NONE',  ( 18.34943919012036773, 8.063251210807163005, 11.49999999999999645 ) ) ;
#55635 = CARTESIAN_POINT ( 'NONE',  ( -80.35919894935766195, -25.31594315932206385, 4.505481293487486383 ) ) ;
#55636 = DIRECTION ( 'NONE',  ( -0.000000000000000000, -0.000000000000000000, -1.000000000000000000 ) ) ;
#55637 = CARTESIAN_POINT ( 'NONE',  ( 4.967620699791259753, -5.876774720514416295, 19.94530485585548973 ) ) ;
#55638 = CARTESIAN_POINT ( 'NONE',  ( 5.097264368846952998, -6.475225279485573360, -27.56135813788808164 ) ) ;
#55639 = EDGE_CURVE ( 'NONE', #44287, #64682, #78112, .T. ) ;
#55640 = DIRECTION ( 'NONE',  ( 0.000000000000000000, 0.000000000000000000, 1.000000000000000000 ) ) ;
#55641 = CARTESIAN_POINT ( 'NONE',  ( 11.36066313177254905, -18.55813952095733654, 11.49999999999998934 ) ) ;
#55642 = CARTESIAN_POINT ( 'NONE',  ( -71.62287095715005592, -29.50248528299804818, 1.056150453629036701 ) ) ;
#55643 = CARTESIAN_POINT ( 'NONE',  ( 18.24227566675094181, -7.298356753547692755, -1.500000000000002220 ) ) ;
#55644 = CARTESIAN_POINT ( 'NONE',  ( -122.6228709571500701, -23.48783264082479505, -1.443836473390058828 ) ) ;
#55645 = B_SPLINE_CURVE_WITH_KNOTS ( 'NONE', 3,
 ( #84565, #15051, #76940, #38393, #85063, #79454 ),
 .UNSPECIFIED., .F., .F.,
 ( 4, 2, 4 ),
 ( 0.000000000000000000, 0.001380764517854767134, 0.002761529035709534268 ),
 .UNSPECIFIED. ) ;
#55646 = VECTOR ( 'NONE', #74479, 1000.000000000000000 ) ;
#55647 = CARTESIAN_POINT ( 'NONE',  ( -110.2093792378191921, -25.27925965549014009, 5.585409257837866903 ) ) ;
#55648 = EDGE_CURVE ( 'NONE', #67134, #38032, #19326, .T. ) ;
#55649 = DIRECTION ( 'NONE',  ( 1.000000000000000000, 3.773278334444167608E-23, 8.201307833595939069E-29 ) ) ;
#55650 = CARTESIAN_POINT ( 'NONE',  ( -30.57287095715006231, -23.47593901973084485, -1.443836476861628304 ) ) ;
#55651 = CARTESIAN_POINT ( 'NONE',  ( -7.762539992054180438, 19.06225842855939234, 11.49999999999999645 ) ) ;
#55652 = CARTESIAN_POINT ( 'NONE',  ( 4.547994309883463870, -5.876774720514421624, 20.87593061325451416 ) ) ;
#55653 = ADVANCED_FACE ( 'NONE', ( #20166 ), #91670, .T. ) ;
#55654 = FACE_OUTER_BOUND ( 'NONE', #80430, .T. ) ;
#55655 = VECTOR ( 'NONE', #25647, 1000.000000000000000 ) ;
#55656 = CARTESIAN_POINT ( 'NONE',  ( 21.16457415087624128, -7.944649954575952577, 11.49999999999999645 ) ) ;
#55657 = ORIENTED_EDGE ( 'NONE', *, *, #26438, .F. ) ;
#55658 = CARTESIAN_POINT ( 'NONE',  ( 0.000000000000000000, 0.000000000000000000, 0.000000000000000000 ) ) ;
#55659 = CARTESIAN_POINT ( 'NONE',  ( -70.22494714645260672, -25.25639600851938837, 7.098707166320516571 ) ) ;
#55660 = CARTESIAN_POINT ( 'NONE',  ( -27.08767087237659865, -24.79334963567931283, 7.466528724393665328 ) ) ;
#55661 = CARTESIAN_POINT ( 'NONE',  ( -108.5228709571500758, -23.48783264083353473, -1.443836473376470586 ) ) ;
#55662 = CARTESIAN_POINT ( 'NONE',  ( -85.62287095715002749, -24.63287334234178516, 0.9662140553045440727 ) ) ;
#55663 = VECTOR ( 'NONE', #77168, 1000.000000000000114 ) ;
#55664 = ADVANCED_FACE ( 'NONE', ( #14042 ), #12589, .T. ) ;
#55665 = CARTESIAN_POINT ( 'NONE',  ( -26.35953173686715800, -24.93063513829692823, 7.694642102573395093 ) ) ;
#55666 = CARTESIAN_POINT ( 'NONE',  ( -2.872281323269014752, 4.293056017849825601, 1.999999999999999556 ) ) ;
#55667 = ORIENTED_EDGE ( 'NONE', *, *, #2908, .F. ) ;
#55668 = CARTESIAN_POINT ( 'NONE',  ( -79.34772585426964042, -25.26750084320114453, 5.924311888455177311 ) ) ;
#55669 = CARTESIAN_POINT ( 'NONE',  ( -22.75767140345847750, 1.815691853630000629, -1.500000000000002220 ) ) ;
#55670 = CARTESIAN_POINT ( 'NONE',  ( -125.5562042904834215, -25.00158670708909980, 2.256160236439166855 ) ) ;
#55671 = B_SPLINE_SURFACE_WITH_KNOTS ( 'NONE', 3, 1, ( 
 ( #6429, #99265 ),
 ( #86044, #6921 ),
 ( #15025, #31762 ),
 ( #46487, #46990 ),
 ( #31253, #45995 ),
 ( #30756, #37383 ),
 ( #60729, #76916 ),
 ( #69321, #309 ),
 ( #77913, #62728 ),
 ( #7415, #8421 ),
 ( #61728, #55108 ) ),
 .UNSPECIFIED., .F., .F., .F.,
 ( 4, 1, 1, 1, 1, 1, 1, 1, 4 ),
 ( 2, 2 ),
 ( 0.000000000000000000, 0.1497703860319676283, 0.2913164099952436636, 0.4259663731047447777, 0.5521595739695276395, 0.6715274135235875796, 0.7861216286916553608, 0.8953250730704447324, 1.000000000000000000 ),
 ( 0.000000000000000000, 1.000000000000000000 ),
 .UNSPECIFIED. ) ;
#55672 = CARTESIAN_POINT ( 'NONE',  ( -115.5228709571500758, -24.91570333825770689, 8.075032458260366752 ) ) ;
#55673 = CARTESIAN_POINT ( 'NONE',  ( -63.55375729026285825, -23.96169478059713143, 10.65365249895718236 ) ) ;
#55674 = CARTESIAN_POINT ( 'NONE',  ( 0.003324065884441271702, 22.49086686382009503, 11.49999999999999645 ) ) ;
#55675 = VERTEX_POINT ( 'NONE', #13049 ) ;
#55676 = CARTESIAN_POINT ( 'NONE',  ( 6.660000000000001030, -10.15233964170348457, 0.003711184059992174607 ) ) ;
#55677 = CARTESIAN_POINT ( 'NONE',  ( -21.49438740719132923, 4.340694165963498996, -1.500000000000002220 ) ) ;
#55678 = CARTESIAN_POINT ( 'NONE',  ( -124.7735373858569403, -25.37153787860454557, 4.078969152973343171 ) ) ;
#55679 = CARTESIAN_POINT ( 'NONE',  ( -34.63526505597382510, -24.35071581493542681, 9.817618358456032368 ) ) ;
#55680 = DIRECTION ( 'NONE',  ( -3.773278334453079030E-23, 0.9999999999976377785, 2.173523156925979128E-06 ) ) ;
#55681 = ORIENTED_EDGE ( 'NONE', *, *, #22985, .F. ) ;
#55682 = CARTESIAN_POINT ( 'NONE',  ( -48.59960390203813319, -23.96169478059712787, 10.65365249895718236 ) ) ;
#55683 = CARTESIAN_POINT ( 'NONE',  ( -111.5228709571500616, -23.48786465467242479, 11.44779295918253936 ) ) ;
#55684 = ORIENTED_EDGE ( 'NONE', *, *, #62396, .T. ) ;
#55685 = CARTESIAN_POINT ( 'NONE',  ( -11.47117155886032158, -16.94740806926979815, 11.49999999999998934 ) ) ;
#55686 = VERTEX_POINT ( 'NONE', #51128 ) ;
#55687 = B_SPLINE_CURVE_WITH_KNOTS ( 'NONE', 3,
 ( #72135, #8725, #17838, #85329, #32052, #54399, #86835, #78214, #63024, #48291, #54901, #24435, #94453, #24935, #77709, #2125, #56417, #23415 ),
 .UNSPECIFIED., .F., .F.,
 ( 4, 2, 2, 2, 2, 2, 2, 2, 4 ),
 ( 2.602085213965210642E-18, 0.0005889077912318151520, 0.001177815582463627702, 0.001766723373695440469, 0.002355631164927252802, 0.002944538956159065135, 0.003533446747390878336, 0.004122354538622689801, 0.004711262329854501267 ),
 .UNSPECIFIED. ) ;
#55688 = ORIENTED_EDGE ( 'NONE', *, *, #97883, .F. ) ;
#55689 = VERTEX_POINT ( 'NONE', #67359 ) ;
#55690 = VERTEX_POINT ( 'NONE', #4953 ) ;
#55691 = CARTESIAN_POINT ( 'NONE',  ( 22.94779996701378266, 2.684060219229261968, 11.49999999999998934 ) ) ;
#55692 = CARTESIAN_POINT ( 'NONE',  ( -41.47713460189704193, -25.30977039686255026, 4.487062071701387822 ) ) ;
#55693 = CARTESIAN_POINT ( 'NONE',  ( 14.61151973098085222, 14.07909450314327771, -1.500000000000002220 ) ) ;
#55694 = CIRCLE ( 'NONE', #81605, 1.530000000000000249 ) ;
#55695 = VERTEX_POINT ( 'NONE', #12559 ) ;
#55696 = DIRECTION ( 'NONE',  ( 0.000000000000000000, -0.9999999999976377785, -2.173523156925979975E-06 ) ) ;
#55697 = CARTESIAN_POINT ( 'NONE',  ( -92.62357504500812411, -24.65952944569303895, 1.056160979905702346 ) ) ;
#55698 = EDGE_CURVE ( 'NONE', #69040, #83981, #96795, .T. ) ;
#55699 = FACE_OUTER_BOUND ( 'NONE', #13203, .T. ) ;
#55700 = CARTESIAN_POINT ( 'NONE',  ( 4.328803674008796065, -5.876774720514407413, 18.75671216747623049 ) ) ;
#55702 = ORIENTED_EDGE ( 'NONE', *, *, #15863, .T. ) ;
#55701 = CARTESIAN_POINT ( 'NONE',  ( -18.34654256122676941, -11.15389649534839833, 11.49999999999999645 ) ) ;
#55703 = CARTESIAN_POINT ( 'NONE',  ( -75.50777110636425959, -24.15503026093913519, -0.2815557561904521444 ) ) ;
#55705 = AXIS2_PLACEMENT_3D ( 'NONE', #82489, #50552, #81507 ) ;
#55704 = CARTESIAN_POINT ( 'NONE',  ( -112.5895376238167245, -24.64898659630368272, 1.056161002820390493 ) ) ;
#55706 = ORIENTED_EDGE ( 'NONE', *, *, #81963, .F. ) ;
#55707 = CARTESIAN_POINT ( 'NONE',  ( 16.28047541435887879, -12.87082401369967677, 11.49999999999998934 ) ) ;
#55709 = EDGE_CURVE ( 'NONE', #60813, #8894, #91927, .T. ) ;
#55708 = VERTEX_POINT ( 'NONE', #43523 ) ;
#55711 = ORIENTED_EDGE ( 'NONE', *, *, #8811, .F. ) ;
#55710 = CARTESIAN_POINT ( 'NONE',  ( -125.5549482276435640, -24.52300882791529801, 0.6510814631126508045 ) ) ;
#55712 = CARTESIAN_POINT ( 'NONE',  ( -111.5868581930692329, -24.66019654487200441, 8.947790411086105067 ) ) ;
#55713 = CARTESIAN_POINT ( 'NONE',  ( -20.27875734969026311, -4.543225279485573864, 24.00402280011862288 ) ) ;
#55714 = ORIENTED_EDGE ( 'NONE', *, *, #92711, .F. ) ;
#55715 = ORIENTED_EDGE ( 'NONE', *, *, #43205, .T. ) ;
#55716 = CARTESIAN_POINT ( 'NONE',  ( -28.98875734969026396, 0.3587747205144265483, 2.362022800118626531 ) ) ;
#55717 = FACE_OUTER_BOUND ( 'NONE', #6007, .T. ) ;
#55718 = CARTESIAN_POINT ( 'NONE',  ( -43.48725217974529045, -24.51419770103157347, 9.386484678747182286 ) ) ;
#55720 = VERTEX_POINT ( 'NONE', #76439 ) ;
#55719 = CARTESIAN_POINT ( 'NONE',  ( 2.156995527713877259, 21.93451973775924557, 11.49999999999999645 ) ) ;
#55721 = DIRECTION ( 'NONE',  ( -1.000000000000000000, 0.000000000000000000, -0.000000000000000000 ) ) ;
#55722 = CARTESIAN_POINT ( 'NONE',  ( -22.20892344277460850, -4.061126821146308963, 11.49999999999998934 ) ) ;
#55723 = CARTESIAN_POINT ( 'NONE',  ( 16.07406896385161943, -13.52096256729613266, 11.49999999999998934 ) ) ;
#55725 = VERTEX_POINT ( 'NONE', #75440 ) ;
#55724 = DIRECTION ( 'NONE',  ( 0.000000000000000000, 0.000000000000000000, 1.000000000000000000 ) ) ;
#55726 = VERTEX_POINT ( 'NONE', #85060 ) ;
#55727 = CARTESIAN_POINT ( 'NONE',  ( -59.62287095715005592, -24.33927499327854704, 9.819080762295818943 ) ) ;
#55728 = ADVANCED_FACE ( 'NONE', ( #8943 ), #24657, .F. ) ;
#55729 = VECTOR ( 'NONE', #11065, 1000.000000000000000 ) ;
#55730 = CARTESIAN_POINT ( 'NONE',  ( -114.5895376238167245, -23.47593901973091235, -1.443836447538999312 ) ) ;
#55731 = ORIENTED_EDGE ( 'NONE', *, *, #6602, .F. ) ;
#55732 = CARTESIAN_POINT ( 'NONE',  ( -3.482456173223098528, 20.84670800329844198, -1.500000000000002220 ) ) ;
#55733 = CARTESIAN_POINT ( 'NONE',  ( -66.62287095715002749, -23.95044443724991368, 10.65354141964649592 ) ) ;
#55734 = CARTESIAN_POINT ( 'NONE',  ( -59.79108751027236934, -25.31249728293746060, 5.276660823416808199 ) ) ;
#55735 = CARTESIAN_POINT ( 'NONE',  ( -49.51573515180496798, -25.27160265537046513, 4.092660780511780061 ) ) ;
#55736 = DIRECTION ( 'NONE',  ( -1.000000000000000000, -0.000000000000000000, -0.000000000000000000 ) ) ;
#55737 = CARTESIAN_POINT ( 'NONE',  ( -35.62287095715005592, -29.50247984919015209, -1.443849546365060466 ) ) ;
#55738 = CARTESIAN_POINT ( 'NONE',  ( 18.11909884760711975, -12.84011383348296853, -1.500000000000002220 ) ) ;
#55739 = AXIS2_PLACEMENT_3D ( 'NONE', #39257, #85938, #30652 ) ;
#55740 = CARTESIAN_POINT ( 'NONE',  ( -114.5168412745318278, -24.34968618360934300, 0.1864209137778971848 ) ) ;
#55741 = B_SPLINE_CURVE_WITH_KNOTS ( 'NONE', 3,
 ( #11674, #50756, #58375, #27419, #19782, #81701 ),
 .UNSPECIFIED., .F., .F.,
 ( 4, 2, 4 ),
 ( 3.087040877776988824E-09, 0.002715410320741953962, 0.005430817554443030659 ),
 .UNSPECIFIED. ) ;
#55742 = ORIENTED_EDGE ( 'NONE', *, *, #53006, .F. ) ;
#55743 = CARTESIAN_POINT ( 'NONE',  ( -110.5228709571500616, -23.47596703998600631, 11.44779298504228038 ) ) ;
#55744 = CARTESIAN_POINT ( 'NONE',  ( 1.000208336950358934, 0.000000000000000000, 0.000000000000000000 ) ) ;
#55745 = CARTESIAN_POINT ( 'NONE',  ( -126.5204133787001268, -24.65952944569306027, 1.056160979905708786 ) ) ;
#55746 = EDGE_CURVE ( 'NONE', #97499, #69556, #10121, .T. ) ;
#55747 = CARTESIAN_POINT ( 'NONE',  ( -41.82789317813108454, -25.25077454730569571, 3.845825085393474563 ) ) ;
#55748 = CARTESIAN_POINT ( 'NONE',  ( -0.1490749075164066184, -21.12010817310450861, 11.44779298504228038 ) ) ;
#55749 = CARTESIAN_POINT ( 'NONE',  ( -2.678125609936932605, 19.29598960679622976, 11.49999999999998934 ) ) ;
#55750 = CARTESIAN_POINT ( 'NONE',  ( -13.99230614532761052, -16.21612836239924960, -1.500000000000002220 ) ) ;
#55751 = CARTESIAN_POINT ( 'NONE',  ( -126.6228709571500843, -24.65952944569305316, 1.056160979905707675 ) ) ;
#55752 = CARTESIAN_POINT ( 'NONE',  ( -60.52202393459451457, -23.48786465467241413, 11.44779295918254824 ) ) ;
#55753 = CARTESIAN_POINT ( 'NONE',  ( -51.58228013677727120, -24.51314013834315730, 0.6176544820404110681 ) ) ;
#55754 = CARTESIAN_POINT ( 'NONE',  ( -38.55620429048340014, -24.65952944569303895, 1.056160979905691688 ) ) ;
#55755 = CARTESIAN_POINT ( 'NONE',  ( 15.23092229589061830, -16.91372389758942418, -1.500000000000002220 ) ) ;
#55756 = DIRECTION ( 'NONE',  ( 1.000000000000000000, 0.000000000000000000, 0.000000000000000000 ) ) ;
#55757 = DIRECTION ( 'NONE',  ( 3.773278334444167608E-23, -1.000000000000000000, 0.000000000000000000 ) ) ;
#55758 = CARTESIAN_POINT ( 'NONE',  ( -2.735935421901279696, -19.66989661884619522, 11.49999999999999645 ) ) ;
#55759 = CARTESIAN_POINT ( 'NONE',  ( -123.5538537614054917, -24.66019654487200441, 8.947790411086106843 ) ) ;
#55760 = CARTESIAN_POINT ( 'NONE',  ( -89.81226385320383088, -25.22391155068715207, 6.409327647370969494 ) ) ;
#55761 = DIRECTION ( 'NONE',  ( -0.6392559695863496705, 6.845827386180411947E-16, -0.7689940216596069522 ) ) ;
#55762 = EDGE_CURVE ( 'NONE', #92089, #78003, #62754, .T. ) ;
#55763 = ORIENTED_EDGE ( 'NONE', *, *, #50954, .F. ) ;
#55764 = PLANE ( 'NONE',  #68816 ) ;
#55765 = CARTESIAN_POINT ( 'NONE',  ( -6.487934372591614540, -5.876774720514411854, 19.49432735726520605 ) ) ;
#55766 = VECTOR ( 'NONE', #93450, 1000.000000000000114 ) ;
#55767 = CARTESIAN_POINT ( 'NONE',  ( -51.04701396381788925, -25.27412261295166829, 2.986905721224212495 ) ) ;
#55768 = CARTESIAN_POINT ( 'NONE',  ( -17.90551237062050305, -12.20792721910736667, -1.500000000000002220 ) ) ;
#55769 = CYLINDRICAL_SURFACE ( 'NONE', #9137, 91.74549126261076992 ) ;
#55770 = CARTESIAN_POINT ( 'NONE',  ( -7.499459838998954631, -17.95702976299720532, -1.500000000000002220 ) ) ;
#55771 = FACE_OUTER_BOUND ( 'NONE', #78708, .T. ) ;
#55772 = ORIENTED_EDGE ( 'NONE', *, *, #36047, .F. ) ;
#55773 = VECTOR ( 'NONE', #38681, 1000.000000000000114 ) ;
#55774 = CARTESIAN_POINT ( 'NONE',  ( 12.15263457413992576, -16.39098610538439615, 11.49999999999999645 ) ) ;
#55775 = DIRECTION ( 'NONE',  ( -0.6599726524652352877, 0.000000000000000000, 0.7512896232465892110 ) ) ;
#55776 = EDGE_CURVE ( 'NONE', #35863, #45042, #30781, .T. ) ;
#55777 = LINE ( 'NONE', #16688, #33506 ) ;
#55778 = EDGE_CURVE ( 'NONE', #63083, #40447, #26717, .T. ) ;
#55779 = VERTEX_POINT ( 'NONE', #86568 ) ;
#55780 = CARTESIAN_POINT ( 'NONE',  ( -0.1426030150137709285, -21.20389190742572083, 11.50200000000000422 ) ) ;
#55781 = CARTESIAN_POINT ( 'NONE',  ( 33.37790122608239329, 4.268345726061002487, -11.54778842029335806 ) ) ;
#55782 = CARTESIAN_POINT ( 'NONE',  ( -39.04762117679405264, -25.27985297379428786, 4.358277487482919987 ) ) ;
#55783 = CARTESIAN_POINT ( 'NONE',  ( 7.749999999999998224, 23.99999999999999289, 0.000000000000000000 ) ) ;
#55784 = LINE ( 'NONE', #35805, #8975 ) ;
#55785 = CARTESIAN_POINT ( 'NONE',  ( 7.746586651691365510, 18.53313339873204058, -1.500000000000002220 ) ) ;
#55786 = EDGE_CURVE ( 'NONE', #5789, #32299, #92173, .T. ) ;
#55787 = B_SPLINE_CURVE_WITH_KNOTS ( 'NONE', 3,
 ( #43538, #11570, #42549, #90200 ),
 .UNSPECIFIED., .F., .F.,
 ( 4, 4 ),
 ( 0.000000000000000000, 0.0002088004239042353695 ),
 .UNSPECIFIED. ) ;
#55788 = DIRECTION ( 'NONE',  ( 0.06975647374412523305, 0.9975640502598241977, 0.000000000000000000 ) ) ;
#55789 = EDGE_LOOP ( 'NONE', ( #24735, #46426, #83118, #74014 ) ) ;
#55790 = DIRECTION ( 'NONE',  ( -3.773278334453079618E-23, 0.9999999999976377785, 2.173523156925979975E-06 ) ) ;
#55791 = ADVANCED_FACE ( 'NONE', ( #93167 ), #92669, .T. ) ;
#55792 = CARTESIAN_POINT ( 'NONE',  ( -16.88208375265294237, -15.58181570610299715, 11.49999999999999645 ) ) ;
#55793 = CARTESIAN_POINT ( 'NONE',  ( 22.67573665902413182, 1.879276792517311501, -1.500000000000002220 ) ) ;
#55794 = ORIENTED_EDGE ( 'NONE', *, *, #53489, .F. ) ;
#55795 = CARTESIAN_POINT ( 'NONE',  ( -53.62287095715007013, -23.96177878511307568, 10.65340807706330217 ) ) ;
#55796 = CARTESIAN_POINT ( 'NONE',  ( -91.52287095715006160, -23.48786465467241769, 11.44779295918254292 ) ) ;
#55797 = CARTESIAN_POINT ( 'NONE',  ( -90.63293755609211644, -24.40034930558990922, 0.3402023900116054045 ) ) ;
#55798 = CARTESIAN_POINT ( 'NONE',  ( -61.35927065337961039, -25.05684680783174656, 7.499198447843678395 ) ) ;
#55799 = CARTESIAN_POINT ( 'NONE',  ( -128.5894277638150243, -24.66019654487200441, 8.947790411086108620 ) ) ;
#55800 = PLANE ( 'NONE',  #54164 ) ;
#55801 = CARTESIAN_POINT ( 'NONE',  ( 0.3000000000000007661, 18.50000000000000000, 0.000000000000000000 ) ) ;
#55802 = LINE ( 'NONE', #32952, #16084 ) ;
#55803 = EDGE_LOOP ( 'NONE', ( #96347, #33927, #98486, #47955 ) ) ;
#55804 = CARTESIAN_POINT ( 'NONE',  ( 14.85214116200856083, 13.97194181870810326, 11.49999999999998934 ) ) ;
#55805 = ORIENTED_EDGE ( 'NONE', *, *, #23694, .F. ) ;
#55806 = ORIENTED_EDGE ( 'NONE', *, *, #99542, .F. ) ;
#55807 = CARTESIAN_POINT ( 'NONE',  ( -22.94451526424785115, -1.264959178018935315, -1.500000000000002220 ) ) ;
#55808 = CARTESIAN_POINT ( 'NONE',  ( -6.989144439031651501, -5.876774720514410966, 19.51167604195716621 ) ) ;
#55809 = ORIENTED_EDGE ( 'NONE', *, *, #51494, .F. ) ;
#55810 = CARTESIAN_POINT ( 'NONE',  ( -110.2414688702968135, -25.26454195069187136, 6.186385695411759755 ) ) ;
#55811 = CARTESIAN_POINT ( 'NONE',  ( -101.5228709571500616, -24.50216790748205042, 0.6166512839542561686 ) ) ;
#55812 = CARTESIAN_POINT ( 'NONE',  ( -19.80875734969026425, -0.3587747205144265483, 31.02402280011862246 ) ) ;
#55813 = CARTESIAN_POINT ( 'NONE',  ( -29.58953762381673869, -24.58133133125748060, 1.056161285064568078 ) ) ;
#55815 = VERTEX_POINT ( 'NONE', #77933 ) ;
#55814 = CARTESIAN_POINT ( 'NONE',  ( -10.68834330497911189, 18.46263264838738039, 11.49999999999999645 ) ) ;
#55816 = VERTEX_POINT ( 'NONE', #17052 ) ;
#55817 = CARTESIAN_POINT ( 'NONE',  ( 1.019757120859956512, 22.21710203930399175, -1.500000000000002220 ) ) ;
#55818 = CARTESIAN_POINT ( 'NONE',  ( 11.79242832063081892, -16.95861370568002613, -1.500000000000002220 ) ) ;
#55819 = AXIS2_PLACEMENT_3D ( 'NONE', #85204, #8086, #98926 ) ;
#55820 = ORIENTED_EDGE ( 'NONE', *, *, #86622, .T. ) ;
#55821 = EDGE_CURVE ( 'NONE', #84008, #628, #9442, .T. ) ;
#55822 = CARTESIAN_POINT ( 'NONE',  ( -5.837039262820512775, -6.376774720514413630, 19.76512419871795245 ) ) ;
#55823 = CARTESIAN_POINT ( 'NONE',  ( -95.60349243063225799, -23.48786465467241058, 11.44779295918254469 ) ) ;
#55824 = ORIENTED_EDGE ( 'NONE', *, *, #62022, .F. ) ;
#55825 = CARTESIAN_POINT ( 'NONE',  ( -112.2228709571500644, -23.47593901973090524, -1.443836447538996648 ) ) ;
#55826 = VERTEX_POINT ( 'NONE', #70348 ) ;
#55827 = CARTESIAN_POINT ( 'NONE',  ( -129.6228709571500417, -24.65952944569305316, 1.056160979905706121 ) ) ;
#55828 = CARTESIAN_POINT ( 'NONE',  ( -71.30293871510559711, -25.23939882842460847, 6.270859370734599203 ) ) ;
#55829 = CARTESIAN_POINT ( 'NONE',  ( 11.28189403632909915, 17.58240144430209995, -1.500000000000002220 ) ) ;
#55830 = CARTESIAN_POINT ( 'NONE',  ( -12.45635911906152771, -17.91357634596933934, 11.49999999999999645 ) ) ;
#55831 = CIRCLE ( 'NONE', #97945, 24.00000000000000000 ) ;
#55832 = CARTESIAN_POINT ( 'NONE',  ( 25.40723128797996822, -4.683802162961660187, -10.80818206156904537 ) ) ;
#55833 = DIRECTION ( 'NONE',  ( 0.8323003000060928969, 0.000000000000000000, 0.5543250044962501066 ) ) ;
#55834 = CARTESIAN_POINT ( 'NONE',  ( 8.413247042826936806, 20.86129769029627923, 11.49999999999998934 ) ) ;
#55835 = CARTESIAN_POINT ( 'NONE',  ( -118.6267491325727406, -23.96169478059713853, 10.65365249895717170 ) ) ;
#55836 = CARTESIAN_POINT ( 'NONE',  ( 21.57151214508649772, 3.625915217019311583E-15, -1.699999999999999956 ) ) ;
#55837 = CARTESIAN_POINT ( 'NONE',  ( -31.55620429048339304, -24.64965694238574656, 8.947790433994208925 ) ) ;
#55838 = VERTEX_POINT ( 'NONE', #831 ) ;
#55839 = ORIENTED_EDGE ( 'NONE', *, *, #96034, .T. ) ;
#55840 = ORIENTED_EDGE ( 'NONE', *, *, #69008, .F. ) ;
#55841 = DIRECTION ( 'NONE',  ( 0.000000000000000000, -1.478457507934778393E-16, -1.000000000000000000 ) ) ;
#55842 = ORIENTED_EDGE ( 'NONE', *, *, #85741, .F. ) ;
#55843 = ADVANCED_FACE ( 'NONE', ( #31785 ), #93672, .T. ) ;
#55844 = CARTESIAN_POINT ( 'NONE',  ( -2.881439591185620319, 21.19155266312798958, -1.500000000000002220 ) ) ;
#55845 = CARTESIAN_POINT ( 'NONE',  ( 3.752539591237177508, -22.04708138622333635, 11.49999999999999645 ) ) ;
#55846 = EDGE_LOOP ( 'NONE', ( #74130, #2052, #10153, #13890 ) ) ;
#55847 = CARTESIAN_POINT ( 'NONE',  ( 32.70752563734568952, -3.536205085657706082, -3.307643893017725212 ) ) ;
#55848 = CARTESIAN_POINT ( 'NONE',  ( 12.48895993392301307, -16.95307763291877379, -1.500000000000002220 ) ) ;
#55849 = CARTESIAN_POINT ( 'NONE',  ( -30.59773033261084763, -24.76236165402489675, 8.640462295247353097 ) ) ;
#55850 = CARTESIAN_POINT ( 'NONE',  ( -7.573260116017839216, 18.43532004384545786, -1.500000000000002220 ) ) ;
#55851 = CARTESIAN_POINT ( 'NONE',  ( -50.62375381348867620, -25.00182538069146432, 7.747789668545041586 ) ) ;
#55852 = ADVANCED_FACE ( 'NONE', ( #78442 ), #10951, .F. ) ;
#55853 = LINE ( 'NONE', #93382, #11004 ) ;
#55854 = CARTESIAN_POINT ( 'NONE',  ( -14.46940225681120396, -16.66540133702554272, -1.500000000000002220 ) ) ;
#55855 = PLANE ( 'NONE',  #86860 ) ;
#55856 = ORIENTED_EDGE ( 'NONE', *, *, #11961, .T. ) ;
#55857 = CARTESIAN_POINT ( 'NONE',  ( -65.62561620482574654, -24.92592662359561473, 8.075495903017998245 ) ) ;
#55858 = ADVANCED_FACE ( 'NONE', ( #73356 ), #18057, .T. ) ;
#55859 = DIRECTION ( 'NONE',  ( -0.000000000000000000, 1.000000000000000000, -0.000000000000000000 ) ) ;
#55860 = CARTESIAN_POINT ( 'NONE',  ( 9.770152518076534065, 18.40777400073588410, 11.49999999999999645 ) ) ;
#55861 = EDGE_CURVE ( 'NONE', #63898, #22592, #47200, .T. ) ;
#55862 = EDGE_CURVE ( 'NONE', #95252, #20296, #50511, .T. ) ;
#55863 = CARTESIAN_POINT ( 'NONE',  ( 29.58897068672300179, -4.307329379639823763, 29.06043472499518643 ) ) ;
#55864 = CARTESIAN_POINT ( 'NONE',  ( -128.6228709571500417, -23.47596703998600631, 11.44779298504227860 ) ) ;
#55865 = EDGE_CURVE ( 'NONE', #16459, #22648, #34394, .T. ) ;
#55866 = CIRCLE ( 'NONE', #36428, 19.30000000000000071 ) ;
#55867 = DIRECTION ( 'NONE',  ( 0.000000000000000000, -1.000000000000000000, 0.000000000000000000 ) ) ;
#55868 = CARTESIAN_POINT ( 'NONE',  ( -18.83571791729191958, -9.990160686573538840, -1.500000000000002220 ) ) ;
#55869 = CARTESIAN_POINT ( 'NONE',  ( -73.62287095715005592, -29.50250243563736774, 8.947779886222143375 ) ) ;
#55870 = CARTESIAN_POINT ( 'NONE',  ( -124.5228709571500616, -23.47593901973090524, -1.443836447538996204 ) ) ;
#55871 = CARTESIAN_POINT ( 'NONE',  ( -68.62287095715004170, -24.66019654487199020, 8.947790411086131712 ) ) ;
#55872 = CARTESIAN_POINT ( 'NONE',  ( -95.62287095715005592, -29.50248789122583659, 2.256150453626215580 ) ) ;
#55873 = CARTESIAN_POINT ( 'NONE',  ( 20.52096793114426276, -9.243637136814692568, -1.500000000000002220 ) ) ;
#55874 = CARTESIAN_POINT ( 'NONE',  ( -112.5562042904833930, -23.47593901973091235, -1.443836447538999312 ) ) ;
#55875 = ORIENTED_EDGE ( 'NONE', *, *, #46789, .F. ) ;
#55876 = CARTESIAN_POINT ( 'NONE',  ( -79.47058872164218712, -25.30399138793138292, 4.798136881959892186 ) ) ;
#55877 = CARTESIAN_POINT ( 'NONE',  ( 7.356505681210999015, -10.77121780415745711, 1.154761385154459585 ) ) ;
#55878 = CARTESIAN_POINT ( 'NONE',  ( 10.64064036176630879, -16.58286410872727146, 11.49999999999999645 ) ) ;
#55879 = LINE ( 'NONE', #86804, #92558 ) ;
#55880 = CARTESIAN_POINT ( 'NONE',  ( -39.62287095715005592, -24.64898659630366851, 1.056161002820819261 ) ) ;
#55881 = ADVANCED_FACE ( 'NONE', ( #49025 ), #40897, .F. ) ;
#55882 = ADVANCED_FACE ( 'NONE', ( #64263 ), #2347, .F. ) ;
#55883 = ORIENTED_EDGE ( 'NONE', *, *, #68587, .F. ) ;
#55884 = DIRECTION ( 'NONE',  ( 0.000000000000000000, -1.478457507934778393E-16, -1.000000000000000000 ) ) ;
#55885 = LINE ( 'NONE', #33529, #54567 ) ;
#55886 = CARTESIAN_POINT ( 'NONE',  ( -101.6228709571500559, -29.50248528299804818, 1.056150453629042030 ) ) ;
#55887 = CARTESIAN_POINT ( 'NONE',  ( -95.52287095715010423, -25.00182538069145366, 7.747789668545101982 ) ) ;
#55888 = DIRECTION ( 'NONE',  ( -0.000000000000000000, -1.000000000000000000, 0.000000000000000000 ) ) ;
#55889 = CARTESIAN_POINT ( 'NONE',  ( 19.74453702311487646, -0.1846442961375113490, -1.500000000000002220 ) ) ;
#55890 = ORIENTED_EDGE ( 'NONE', *, *, #67772, .F. ) ;
#55891 = CARTESIAN_POINT ( 'NONE',  ( -5.148175472751820081, -19.54457232503198227, 11.49999999999999645 ) ) ;
#55892 = CARTESIAN_POINT ( 'NONE',  ( 5.654871928786437074, -5.876774720514420736, 20.64717925217163952 ) ) ;
#55893 = AXIS2_PLACEMENT_3D ( 'NONE', #55159, #56159, #81351 ) ;
#55894 = EDGE_CURVE ( 'NONE', #85639, #1549, #26679, .T. ) ;
#55895 = EDGE_LOOP ( 'NONE', ( #43466, #41470, #42700, #8928, #84198, #47840, #20329, #4046 ) ) ;
#55896 = DIRECTION ( 'NONE',  ( 0.000000000000000000, 2.173523156925980399E-06, -0.9999999999976378895 ) ) ;
#55897 = CARTESIAN_POINT ( 'NONE',  ( -70.29603126573300642, -25.30156935299296350, 5.315006326144771087 ) ) ;
#55898 = DIRECTION ( 'NONE',  ( 0.000000000000000000, -1.000000000000000000, -4.336808689942018722E-16 ) ) ;
#55899 = DIRECTION ( 'NONE',  ( 0.000000000000000000, -1.000000000000000000, 0.000000000000000000 ) ) ;
#55900 = CARTESIAN_POINT ( 'NONE',  ( -124.5228709571500616, -23.47593901973090524, -1.443836447538996204 ) ) ;
#55901 = CARTESIAN_POINT ( 'NONE',  ( -61.52287095715006160, -24.65952944569304606, 1.056160979905695463 ) ) ;
#55902 = CARTESIAN_POINT ( 'NONE',  ( 19.27460657395150889, -5.330843762518559181, 11.49999999999998934 ) ) ;
#55903 = EDGE_CURVE ( 'NONE', #47315, #37803, #43607, .T. ) ;
#55904 = VECTOR ( 'NONE', #55061, 1000.000000000000000 ) ;
#55905 = CARTESIAN_POINT ( 'NONE',  ( -67.62287095715005592, -23.48783264082478794, -1.443836473390067265 ) ) ;
#55906 = CARTESIAN_POINT ( 'NONE',  ( -116.5166189026680570, -24.51419770103160189, 9.386484678747169852 ) ) ;
#55907 = ORIENTED_EDGE ( 'NONE', *, *, #30882, .F. ) ;
#55908 = EDGE_CURVE ( 'NONE', #65310, #79871, #25161, .T. ) ;
#55909 = EDGE_CURVE ( 'NONE', #3731, #24383, #56138, .T. ) ;
#55910 = CARTESIAN_POINT ( 'NONE',  ( -79.64188460053713925, -23.73791477778911840, 11.05961554403170943 ) ) ;
#55911 = CARTESIAN_POINT ( 'NONE',  ( -35.57399695948890184, -24.92564183028978775, 1.928384488918258199 ) ) ;
#55912 = CARTESIAN_POINT ( 'NONE',  ( 29.73860345376319003, -1.477225279485574028, 19.84760796525321780 ) ) ;
#55913 = FACE_OUTER_BOUND ( 'NONE', #62959, .T. ) ;
#55914 = CARTESIAN_POINT ( 'NONE',  ( -45.62287095715004881, -29.50248789122583659, 2.256150453626215580 ) ) ;
#55915 = DIRECTION ( 'NONE',  ( 1.000000000000000000, 3.773278334444167608E-23, 8.201307833595939069E-29 ) ) ;
#55916 = EDGE_CURVE ( 'NONE', #60171, #26914, #49037, .T. ) ;
#55917 = CARTESIAN_POINT ( 'NONE',  ( -59.62287095715004881, -29.50247984919015209, -1.443849546365056913 ) ) ;
#55918 = ORIENTED_EDGE ( 'NONE', *, *, #49822, .F. ) ;
#55919 = CARTESIAN_POINT ( 'NONE',  ( 9.670762957215185196, 17.83519281925787325, -1.500000000000002220 ) ) ;
#55920 = CARTESIAN_POINT ( 'NONE',  ( 31.69157588030356010, 3.540801019308528197, 29.47507166493026176 ) ) ;
#55921 = CARTESIAN_POINT ( 'NONE',  ( -34.58067719238572124, -24.51314013834315375, 0.6176544820404091807 ) ) ;
#55922 = CARTESIAN_POINT ( 'NONE',  ( 282.9764569301858046, -5.965225279485572685, 20.79159422840526616 ) ) ;
#55923 = VERTEX_POINT ( 'NONE', #2854 ) ;
#55924 = DIRECTION ( 'NONE',  ( 0.000000000000000000, -2.173523156925979552E-06, 0.9999999999976378895 ) ) ;
#55925 = CARTESIAN_POINT ( 'NONE',  ( -4.116507902937485142, 19.75820112358731251, -1.500000000000002220 ) ) ;
#55926 = CARTESIAN_POINT ( 'NONE',  ( 8.100108036306837178, -19.54698220168213041, 11.49999999999999645 ) ) ;
#55927 = VECTOR ( 'NONE', #57018, 1000.000000000000000 ) ;
#55928 = CARTESIAN_POINT ( 'NONE',  ( 21.13975321936677787, -6.629177502137091338, 11.49999999999998934 ) ) ;
#55929 = CARTESIAN_POINT ( 'NONE',  ( -19.86366060283327784, 5.362777492974458049, -1.500000000000002220 ) ) ;
#55930 = CARTESIAN_POINT ( 'NONE',  ( 16.89397143409390623, -6.376774720514426953, 16.89397143409405899 ) ) ;
#55931 = ORIENTED_EDGE ( 'NONE', *, *, #64959, .T. ) ;
#55932 = CARTESIAN_POINT ( 'NONE',  ( -94.58953762381672448, -24.66019654487198665, 8.947790411086135265 ) ) ;
#55933 = VERTEX_POINT ( 'NONE', #95686 ) ;
#55934 = CARTESIAN_POINT ( 'NONE',  ( 8.971512145086528278, -9.528487854913501920, 4.500000000000002665 ) ) ;
#55935 = CARTESIAN_POINT ( 'NONE',  ( -34.52287095715006160, -29.50248528299804818, 1.056150453629029817 ) ) ;
#55936 = ORIENTED_EDGE ( 'NONE', *, *, #31323, .F. ) ;
#55937 = ORIENTED_EDGE ( 'NONE', *, *, #67515, .T. ) ;
#55938 = ORIENTED_EDGE ( 'NONE', *, *, #6852, .F. ) ;
#55939 = CARTESIAN_POINT ( 'NONE',  ( -110.4120913896815352, -25.12089013549993410, 2.834570756958135540 ) ) ;
#55940 = FACE_OUTER_BOUND ( 'NONE', #22605, .T. ) ;
#55941 = CARTESIAN_POINT ( 'NONE',  ( 5.367993895751241418, -5.876774720514418071, 20.45854982692612722 ) ) ;
#55942 = CARTESIAN_POINT ( 'NONE',  ( -1.268444833121266546, 20.69640364028325052, -1.500000000000002220 ) ) ;
#55943 = CARTESIAN_POINT ( 'NONE',  ( -1.126084586642228436, -21.63456646517454729, 11.49999999999999645 ) ) ;
#55944 = ORIENTED_EDGE ( 'NONE', *, *, #87000, .T. ) ;
#55945 = DIRECTION ( 'NONE',  ( 0.000000000000000000, 1.000000000000000000, 0.000000000000000000 ) ) ;
#55946 = CARTESIAN_POINT ( 'NONE',  ( 2.591645189881369493, -5.876774720514412742, 19.84288601127407148 ) ) ;
#55947 = CARTESIAN_POINT ( 'NONE',  ( 5.309366582633749054, -21.77581755331916824, 11.49999999999998934 ) ) ;
#55948 = FACE_OUTER_BOUND ( 'NONE', #76985, .T. ) ;
#55949 = CARTESIAN_POINT ( 'NONE',  ( -2.749999999999999112, 27.59999999999999432, 0.000000000000000000 ) ) ;
#55950 = ORIENTED_EDGE ( 'NONE', *, *, #97273, .T. ) ;
#55951 = PLANE ( 'NONE',  #32307 ) ;
#55952 = CARTESIAN_POINT ( 'NONE',  ( -35.47953491189426956, -24.63419186844611630, 9.035850630976925757 ) ) ;
#55953 = ORIENTED_EDGE ( 'NONE', *, *, #38850, .T. ) ;
#55954 = EDGE_LOOP ( 'NONE', ( #81488, #92514, #89062, #13112 ) ) ;
#55955 = CIRCLE ( 'NONE', #47835, 11.85241003308276042 ) ;
#55956 = PLANE ( 'NONE',  #50655 ) ;
#55957 = VERTEX_POINT ( 'NONE', #17559 ) ;
#55958 = CARTESIAN_POINT ( 'NONE',  ( -11.64875734969026233, 0.3587747205144265483, 31.02402280011862246 ) ) ;
#55959 = ADVANCED_FACE ( 'NONE', ( #42424 ), #11445, .F. ) ;
#55960 = CARTESIAN_POINT ( 'NONE',  ( -1.563627757057377110, -21.15500258984412696, -1.500000000000002220 ) ) ;
#55961 = ORIENTED_EDGE ( 'NONE', *, *, #56225, .T. ) ;
#55962 = CARTESIAN_POINT ( 'NONE',  ( -50.51069548810792753, -23.85016227208580020, -0.8807180028928345283 ) ) ;
#55963 = ADVANCED_FACE ( 'NONE', ( #96678 ), #27179, .F. ) ;
#55964 = B_SPLINE_CURVE_WITH_KNOTS ( 'NONE', 3,
 ( #57012, #87949, #80328, #3232, #1714, #34165, #47889, #32650 ),
 .UNSPECIFIED., .F., .F.,
 ( 4, 2, 2, 4 ),
 ( 6.391158118975384497E-06, 0.002007136338672933090, 0.003007508928949907765, 0.004007881519226881573 ),
 .UNSPECIFIED. ) ;
#55965 = CARTESIAN_POINT ( 'NONE',  ( 8.287826148123016878, -20.17477452812186201, 11.49999999999998934 ) ) ;
#55966 = CARTESIAN_POINT ( 'NONE',  ( -103.6267837749912957, -24.35071581493543391, 9.817618358456027039 ) ) ;
#55967 = EDGE_CURVE ( 'NONE', #13730, #85108, #68935, .T. ) ;
#55968 = CARTESIAN_POINT ( 'NONE',  ( -62.58953762381672448, -24.66019654487198665, 8.947790411086129936 ) ) ;
#55969 = CARTESIAN_POINT ( 'NONE',  ( -35.52287095715008292, -23.84081130425356676, 10.88220057483159309 ) ) ;
#55970 = CARTESIAN_POINT ( 'NONE',  ( 4.989390281198801347, -21.28523531580253803, -1.500000000000002220 ) ) ;
#55971 = DIRECTION ( 'NONE',  ( 0.1489078231574191002, 6.845827386180410961E-16, -0.9888510809027407644 ) ) ;
#55972 = ORIENTED_EDGE ( 'NONE', *, *, #44864, .T. ) ;
#55973 = CARTESIAN_POINT ( 'NONE',  ( -40.43756433397305017, -25.12049752546737835, 2.832404795212222659 ) ) ;
#55974 = CARTESIAN_POINT ( 'NONE',  ( -85.65008588651460286, -23.48786465467240703, 11.44779295918254647 ) ) ;
#55975 = ORIENTED_EDGE ( 'NONE', *, *, #64015, .F. ) ;
#55976 = CIRCLE ( 'NONE', #60827, 1.699999999999996625 ) ;
#55977 = ADVANCED_FACE ( 'NONE', ( #35297 ), #98165, .T. ) ;
#55978 = EDGE_CURVE ( 'NONE', #79255, #86407, #67246, .T. ) ;
#55979 = AXIS2_PLACEMENT_3D ( 'NONE', #46428, #77359, #48439 ) ;
#55980 = ORIENTED_EDGE ( 'NONE', *, *, #95147, .T. ) ;
#55981 = EDGE_CURVE ( 'NONE', #55313, #70518, #27781, .T. ) ;
#55982 = ORIENTED_EDGE ( 'NONE', *, *, #56096, .T. ) ;
#55983 = CARTESIAN_POINT ( 'NONE',  ( 29.73860345376319358, -5.356774720496559894, 1.647607965253213846 ) ) ;
#55984 = EDGE_CURVE ( 'NONE', #82993, #67077, #13431, .T. ) ;
#55985 = CARTESIAN_POINT ( 'NONE',  ( -31.24388727629349560, -25.13054166897875774, 2.818273575189820690 ) ) ;
#55986 = CARTESIAN_POINT ( 'NONE',  ( 15.87343765641381665, 14.11872912734625274, 11.49999999999998934 ) ) ;
#55987 = CARTESIAN_POINT ( 'NONE',  ( -122.5228709571500616, -24.64965694238408034, 8.947790433994191162 ) ) ;
#55988 = CARTESIAN_POINT ( 'NONE',  ( -130.5728709571501156, -25.57033040079278763, 6.142048374048878046 ) ) ;
#55989 = DIRECTION ( 'NONE',  ( 0.000000000000000000, -0.9999999999976377785, -2.173523156925979128E-06 ) ) ;
#55990 = CARTESIAN_POINT ( 'NONE',  ( -20.77875734969026311, 3.316774720514426456, 27.45402280011862572 ) ) ;
#55991 = CARTESIAN_POINT ( 'NONE',  ( 12.39309347844599252, 14.90900669795185252, 11.49999999999998934 ) ) ;
#55992 = CARTESIAN_POINT ( 'NONE',  ( -117.6235066768902016, -24.66019654487200441, 8.947790411086110396 ) ) ;
#55993 = ORIENTED_EDGE ( 'NONE', *, *, #69635, .T. ) ;
#55994 = CARTESIAN_POINT ( 'NONE',  ( 19.46547125265945155, -1.073068822128883104, 11.49999999999999645 ) ) ;
#55995 = CARTESIAN_POINT ( 'NONE',  ( 31.62974406627585466, -4.069828902950619387, 27.10097837741100335 ) ) ;
#55996 = DIRECTION ( 'NONE',  ( -7.960204194457801640E-17, -1.000000000000000000, 1.571307496355802463E-16 ) ) ;
#55997 = EDGE_CURVE ( 'NONE', #53720, #22015, #35162, .T. ) ;
#55998 = ORIENTED_EDGE ( 'NONE', *, *, #80542, .T. ) ;
#55999 = CARTESIAN_POINT ( 'NONE',  ( 4.736659488006659480, -6.376774720514420736, 21.25082490164487581 ) ) ;
#56000 = FACE_OUTER_BOUND ( 'NONE', #95729, .T. ) ;
#56001 = CARTESIAN_POINT ( 'NONE',  ( -51.52287095715009002, -23.48783264082477018, -1.443836473390092578 ) ) ;
#56002 = CARTESIAN_POINT ( 'NONE',  ( -81.87824661256287584, -25.24813725404296960, 6.339755482797981401 ) ) ;
#56004 = EDGE_CURVE ( 'NONE', #76864, #11608, #94457, .T. ) ;
#56003 = CARTESIAN_POINT ( 'NONE',  ( -17.62174901100306101, -8.731699659924187173, 11.49999999999998934 ) ) ;
#56005 = ORIENTED_EDGE ( 'NONE', *, *, #87511, .T. ) ;
#56006 = AXIS2_PLACEMENT_3D ( 'NONE', #28191, #43917, #63401 ) ;
#56007 = LINE ( 'NONE', #86932, #99063 ) ;
#56008 = CARTESIAN_POINT ( 'NONE',  ( -22.63574357292403860, -4.499050354539342322, -1.500000000000002220 ) ) ;
#56009 = DATE_TIME_ROLE ( 'creation_date' ) ;
#56010 = CARTESIAN_POINT ( 'NONE',  ( -106.5895376238167529, -24.64965694238407679, 8.947790433994649462 ) ) ;
#56011 = CARTESIAN_POINT ( 'NONE',  ( 3.825768195983636044, -6.376774720514424288, 21.47884071039599618 ) ) ;
#56012 = CARTESIAN_POINT ( 'NONE',  ( -97.62752127768544597, -24.35071581493544102, 9.817618358456025263 ) ) ;
#56013 = CYLINDRICAL_SURFACE ( 'NONE', #98525, 11.85241003308275864 ) ;
#56014 = CARTESIAN_POINT ( 'NONE',  ( 5.981014360695730225, -5.876774720514425177, 21.36744920115099333 ) ) ;
#56015 = CARTESIAN_POINT ( 'NONE',  ( -129.5217893627370245, -24.65952944569305316, 1.056160979905705899 ) ) ;
#56016 = CARTESIAN_POINT ( 'NONE',  ( -99.12822588951706848, -25.31565927954684625, 4.142262207320525746 ) ) ;
#56017 = CARTESIAN_POINT ( 'NONE',  ( -19.52388446859773552, -3.948942086532154061, -1.500000000000002220 ) ) ;
#56018 = CARTESIAN_POINT ( 'NONE',  ( -68.52287095715006160, -23.48786465467241058, 11.44779295918254647 ) ) ;
#56019 = CARTESIAN_POINT ( 'NONE',  ( -4.105667982141768313, -19.37954422259287668, -1.500000000000002220 ) ) ;
#56020 = ORIENTED_EDGE ( 'NONE', *, *, #12908, .T. ) ;
#56021 = CARTESIAN_POINT ( 'NONE',  ( 1.095236984349686749, 8.494825072090636198, 1.700000000000008393 ) ) ;
#56022 = EDGE_CURVE ( 'NONE', #91581, #23237, #53310, .T. ) ;
#56023 = B_SPLINE_CURVE_WITH_KNOTS ( 'NONE', 3,
 ( #3331, #33249, #80931, #58113, #64229, #25640 ),
 .UNSPECIFIED., .F., .F.,
 ( 4, 2, 4 ),
 ( 0.000000000000000000, 0.001380901958385395700, 0.002761803916770791401 ),
 .UNSPECIFIED. ) ;
#56024 = DIRECTION ( 'NONE',  ( -1.000000000000000000, -0.000000000000000000, -0.000000000000000000 ) ) ;
#56025 = DIRECTION ( 'NONE',  ( -0.000000000000000000, 2.173523156925979552E-06, -0.9999999999976378895 ) ) ;
#56026 = CARTESIAN_POINT ( 'NONE',  ( -14.56105648253378781, -14.73650127990469016, 11.49999999999999645 ) ) ;
#56027 = DIRECTION ( 'NONE',  ( -1.000000000000000000, -3.491481338843132961E-15, -2.352173255807796056E-16 ) ) ;
#56028 = EDGE_CURVE ( 'NONE', #69852, #97596, #99162, .T. ) ;
#56029 = CARTESIAN_POINT ( 'NONE',  ( -126.5895376238167529, -24.64898659630529565, 1.056161002820836359 ) ) ;
#56030 = CARTESIAN_POINT ( 'NONE',  ( 22.20067557195093855, 5.203973054738295190, 11.49999999999999645 ) ) ;
#56031 = AXIS2_PLACEMENT_3D ( 'NONE', #49704, #42088, #10624 ) ;
#56032 = ORIENTED_EDGE ( 'NONE', *, *, #16995, .F. ) ;
#56033 = CARTESIAN_POINT ( 'NONE',  ( -69.50623498437037995, -24.15543982623907482, -0.2315651400026648155 ) ) ;
#56034 = CARTESIAN_POINT ( 'NONE',  ( -89.58953762381671027, -23.47596703998600631, 11.44779298504227683 ) ) ;
#56035 = ORIENTED_EDGE ( 'NONE', *, *, #7420, .T. ) ;
#56036 = VECTOR ( 'NONE', #36005, 1000.000000000000000 ) ;
#56037 = CARTESIAN_POINT ( 'NONE',  ( 11.17094659993960803, -16.83544227557131023, -1.500000000000002220 ) ) ;
#56038 = CARTESIAN_POINT ( 'NONE',  ( -89.92287095715005307, -23.47596703998600631, 11.44779298504227860 ) ) ;
#56039 = VECTOR ( 'NONE', #26329, 1000.000000000000000 ) ;
#56040 = CARTESIAN_POINT ( 'NONE',  ( -41.22892028381910734, -25.30353790740849007, 4.765619386710907790 ) ) ;
#56041 = VECTOR ( 'NONE', #75133, 1000.000000000000000 ) ;
#56042 = EDGE_LOOP ( 'NONE', ( #2379, #9235, #69752, #71927 ) ) ;
#56043 = DIRECTION ( 'NONE',  ( -0.6392559695863496705, -6.845827386180411947E-16, -0.7689940216596069522 ) ) ;
#56044 = CARTESIAN_POINT ( 'NONE',  ( -84.52287095715006160, -23.47596703998600631, 11.44779298504228571 ) ) ;
#56045 = CARTESIAN_POINT ( 'NONE',  ( -18.22994410263883225, 8.285605901428201747, -1.500000000000002220 ) ) ;
#56046 = CARTESIAN_POINT ( 'NONE',  ( -110.3139465455115129, -25.11033443737754212, 2.832404817301930056 ) ) ;
#56047 = CARTESIAN_POINT ( 'NONE',  ( 18.03207908435136986, 10.65457695745678457, 11.49999999999999645 ) ) ;
#56048 = CARTESIAN_POINT ( 'NONE',  ( -54.62287095715005592, -23.48786465467240347, 11.44779295918255180 ) ) ;
#56049 = DIRECTION ( 'NONE',  ( -1.000000000000000000, -0.000000000000000000, -0.000000000000000000 ) ) ;
#56050 = CARTESIAN_POINT ( 'NONE',  ( 20.57837473233041692, -7.934362236255416256, -1.500000000000002220 ) ) ;
#56051 = CARTESIAN_POINT ( 'NONE',  ( -8.978253834636468866, -5.876774720514426953, 0.000000000000000000 ) ) ;
#56052 = ORIENTED_EDGE ( 'NONE', *, *, #67527, .F. ) ;
#56053 = LINE ( 'NONE', #10867, #71131 ) ;
#56054 = CARTESIAN_POINT ( 'NONE',  ( 0.000000000000000000, 1.826774720514426464, 6.000000000000000888 ) ) ;
#56055 = DIRECTION ( 'NONE',  ( 1.000000000000000000, 3.773278334444166432E-23, 8.201307841325785021E-29 ) ) ;
#56056 = ORIENTED_EDGE ( 'NONE', *, *, #40107, .T. ) ;
#56057 = CARTESIAN_POINT ( 'NONE',  ( 2.598318274922708060, -6.376774720514413630, 19.68966562063331693 ) ) ;
#56058 = ORIENTED_EDGE ( 'NONE', *, *, #56796, .T. ) ;
#56059 = ORIENTED_EDGE ( 'NONE', *, *, #4977, .F. ) ;
#56060 = CARTESIAN_POINT ( 'NONE',  ( -78.62287095715005592, -23.47593901973091235, -1.443836447539004642 ) ) ;
#56061 = DIRECTION ( 'NONE',  ( 1.000000000000000000, 0.000000000000000000, 0.000000000000000000 ) ) ;
#56062 = CARTESIAN_POINT ( 'NONE',  ( -96.62287095715005592, -29.50250786944525672, 11.44777988621623166 ) ) ;
#56063 = CARTESIAN_POINT ( 'NONE',  ( -19.72667040167412722, -5.651925516699977337, -1.500000000000002220 ) ) ;
#56064 = VERTEX_POINT ( 'NONE', #53017 ) ;
#56065 = CARTESIAN_POINT ( 'NONE',  ( -116.6228709571500417, -24.66019654487199730, 8.947790411086121054 ) ) ;
#56066 = CARTESIAN_POINT ( 'NONE',  ( 6.792576760808763936, -5.876774720514415407, 20.16775508794004779 ) ) ;
#56067 = LINE ( 'NONE', #3289, #23707 ) ;
#56068 = CARTESIAN_POINT ( 'NONE',  ( 21.15698459081360383, -7.064864530413820454, 11.49999999999998934 ) ) ;
#56069 = DIRECTION ( 'NONE',  ( -3.773278334453079618E-23, 0.9999999999976377785, 2.173523156925979975E-06 ) ) ;
#56070 = CARTESIAN_POINT ( 'NONE',  ( -125.6228709571500559, -23.48786465467241769, 11.44779295918253403 ) ) ;
#56071 = ORIENTED_EDGE ( 'NONE', *, *, #95620, .T. ) ;
#56072 = LINE ( 'NONE', #87004, #54989 ) ;
#56073 = PLANE ( 'NONE',  #58871 ) ;
#56074 = CARTESIAN_POINT ( 'NONE',  ( 4.135342931496230001, -20.44547621892628797, 11.49999999999998934 ) ) ;
#56075 = ORIENTED_EDGE ( 'NONE', *, *, #26355, .F. ) ;
#56077 = ORIENTED_EDGE ( 'NONE', *, *, #51159, .T. ) ;
#56076 = DIRECTION ( 'NONE',  ( -0.000000000000000000, -0.000000000000000000, -1.000000000000000000 ) ) ;
#56078 = ORIENTED_EDGE ( 'NONE', *, *, #64247, .F. ) ;
#56079 = ADVANCED_FACE ( 'NONE', ( #36783 ), #66759, .T. ) ;
#56080 = LINE ( 'NONE', #10896, #22782 ) ;
#56081 = CARTESIAN_POINT ( 'NONE',  ( -1.999300432013352058, 20.99099883833691749, -1.500000000000002220 ) ) ;
#56082 = ORIENTED_EDGE ( 'NONE', *, *, #99474, .T. ) ;
#56083 = CARTESIAN_POINT ( 'NONE',  ( 22.02124265030973760, -6.376774720514428729, 13.20402280011862395 ) ) ;
#56085 = EDGE_CURVE ( 'NONE', #2131, #43884, #18238, .T. ) ;
#56084 = FACE_OUTER_BOUND ( 'NONE', #77290, .T. ) ;
#56086 = CARTESIAN_POINT ( 'NONE',  ( -120.5922445377380114, -23.85049219812686871, 10.88485053497526778 ) ) ;
#56087 = CARTESIAN_POINT ( 'NONE',  ( -86.55452498666917904, -23.96169478059713498, 10.65365249895717881 ) ) ;
#56088 = CARTESIAN_POINT ( 'NONE',  ( -59.54826027102925678, -24.15543982623906416, -0.2315651400026668416 ) ) ;
#56089 = CARTESIAN_POINT ( 'NONE',  ( -73.52287095715007581, -29.50248528299804818, 1.056150453629036701 ) ) ;
#56090 = PLANE ( 'NONE',  #15736 ) ;
#56092 = EDGE_LOOP ( 'NONE', ( #75387, #52146, #12100, #83375 ) ) ;
#56091 = CARTESIAN_POINT ( 'NONE',  ( -21.14055147415990277, -6.693858341896442354, 11.49999999999999645 ) ) ;
#56093 = CARTESIAN_POINT ( 'NONE',  ( -99.00614725376551917, -25.30400258354788434, 5.550674214932294959 ) ) ;
#56094 = DIRECTION ( 'NONE',  ( -1.000000000000000000, 0.000000000000000000, -1.226388327005079762E-16 ) ) ;
#56095 = ORIENTED_EDGE ( 'NONE', *, *, #71207, .T. ) ;
#56096 = EDGE_CURVE ( 'NONE', #17609, #26067, #43899, .T. ) ;
#56097 = CARTESIAN_POINT ( 'NONE',  ( -21.51096707683950626, -7.176001652309477841, 11.49999999999998934 ) ) ;
#56098 = EDGE_CURVE ( 'NONE', #23800, #77005, #37776, .T. ) ;
#56099 = AXIS2_PLACEMENT_3D ( 'NONE', #39399, #70353, #61757 ) ;
#56101 = ORIENTED_EDGE ( 'NONE', *, *, #46286, .F. ) ;
#56100 = CARTESIAN_POINT ( 'NONE',  ( -76.62287095715007013, -23.47593901973091235, -1.443836447539004642 ) ) ;
#56102 = EDGE_CURVE ( 'NONE', #73050, #61311, #15540, .T. ) ;
#56103 = EDGE_LOOP ( 'NONE', ( #64339, #46582, #40735, #76638 ) ) ;
#56104 = ADVANCED_FACE ( 'NONE', ( #16420 ), #51499, .T. ) ;
#56105 = DIRECTION ( 'NONE',  ( 0.000000000000000000, -1.020425574104004369E-16, 1.000000000000000000 ) ) ;
#56106 = AXIS2_PLACEMENT_3D ( 'NONE', #53047, #30689, #61166 ) ;
#56107 = CARTESIAN_POINT ( 'NONE',  ( 1.109688723463823301, -20.12803150795971874, 11.49999999999998934 ) ) ;
#56108 = CYLINDRICAL_SURFACE ( 'NONE', #63579, 1.325999999999990298 ) ;
#56109 = ORIENTED_EDGE ( 'NONE', *, *, #48770, .T. ) ;
#56110 = CIRCLE ( 'NONE', #26907, 10.49999999999999112 ) ;
#56111 = DIRECTION ( 'NONE',  ( 0.000000000000000000, -1.000000000000000000, 0.000000000000000000 ) ) ;
#56112 = CARTESIAN_POINT ( 'NONE',  ( -18.94483701893047467, 11.91932228829616669, -1.500000000000002220 ) ) ;
#56113 = VECTOR ( 'NONE', #46257, 1000.000000000000114 ) ;
#56114 = B_SPLINE_CURVE_WITH_KNOTS ( 'NONE', 3,
 ( #30927, #53279, #77589, #91824 ),
 .UNSPECIFIED., .F., .F.,
 ( 4, 4 ),
 ( 0.000000000000000000, 1.000000000000000000 ),
 .UNSPECIFIED. ) ;
#56115 = VECTOR ( 'NONE', #1586, 1000.000000000000114 ) ;
#56116 = VERTEX_POINT ( 'NONE', #30662 ) ;
#56117 = ORIENTED_EDGE ( 'NONE', *, *, #97955, .F. ) ;
#56118 = CARTESIAN_POINT ( 'NONE',  ( -112.5918939201014553, -23.96169478059713498, 10.65365249895717348 ) ) ;
#56119 = CARTESIAN_POINT ( 'NONE',  ( -4.465079497292244959, -5.876774720514410077, 19.29815762497054976 ) ) ;
#56120 = CARTESIAN_POINT ( 'NONE',  ( -39.49513710205338413, -25.30491637845361552, 4.489908266797987935 ) ) ;
#56121 = CARTESIAN_POINT ( 'NONE',  ( 31.74473449900405697, 4.976825198871215328, -4.259190951192157293 ) ) ;
#56122 = AXIS2_PLACEMENT_3D ( 'NONE', #48042, #86092, #2370 ) ;
#56123 = FACE_OUTER_BOUND ( 'NONE', #93493, .T. ) ;
#56124 = CARTESIAN_POINT ( 'NONE',  ( -5.392953615240748455, 18.82278424538476713, -1.500000000000002220 ) ) ;
#56125 = CARTESIAN_POINT ( 'NONE',  ( -46.56050886298546487, -23.73766607897669800, -1.055555164236460230 ) ) ;
#56126 = ORIENTED_EDGE ( 'NONE', *, *, #23680, .F. ) ;
#56127 = CARTESIAN_POINT ( 'NONE',  ( 8.900169022907615357, -19.58186849131130813, 11.49999999999998934 ) ) ;
#56128 = CARTESIAN_POINT ( 'NONE',  ( -128.5217325982747241, -24.15543982623908548, -0.2315651400026392803 ) ) ;
#56129 = FACE_OUTER_BOUND ( 'NONE', #2564, .T. ) ;
#56130 = CARTESIAN_POINT ( 'NONE',  ( -101.5391830360295558, -25.20975163562174259, 3.394848129468846842 ) ) ;
#56131 = CARTESIAN_POINT ( 'NONE',  ( -13.89275734969026388, 5.965225279485572685, 30.51402280011862089 ) ) ;
#56132 = CARTESIAN_POINT ( 'NONE',  ( -9.034649315346676701, 21.08484869742704504, -1.500000000000002220 ) ) ;
#56133 = APPROVAL_STATUS ( 'not_yet_approved' ) ;
#56134 = CARTESIAN_POINT ( 'NONE',  ( -71.30261592386577263, -25.26164592712893509, 6.148532042880709980 ) ) ;
#56135 = CARTESIAN_POINT ( 'NONE',  ( -16.75416981316412190, 10.96944243606782443, 11.49999999999999645 ) ) ;
#56136 = CARTESIAN_POINT ( 'NONE',  ( -11.64875734969026233, 5.965225279485572685, 31.02402280011862246 ) ) ;
#56137 = CARTESIAN_POINT ( 'NONE',  ( -76.62287095715007013, -29.50250786944525672, 11.44777988621623521 ) ) ;
#56138 = LINE ( 'NONE', #41403, #57156 ) ;
#56139 = PLANE ( 'NONE',  #40762 ) ;
#56140 = CARTESIAN_POINT ( 'NONE',  ( -50.62287095715007013, -24.15516710230294350, 10.28746687063725673 ) ) ;
#56141 = CARTESIAN_POINT ( 'NONE',  ( -19.53060160647804722, 3.385818350044136338, 11.49999999999998934 ) ) ;
#56142 = CARTESIAN_POINT ( 'NONE',  ( 20.57166443188586769, -7.073620337204646447, 11.49999999999998934 ) ) ;
#56143 = CARTESIAN_POINT ( 'NONE',  ( -107.6228709571500701, -29.50248528299804818, 1.056150453629043584 ) ) ;
#56144 = CARTESIAN_POINT ( 'NONE',  ( -9.385407830382300531, 17.29636241635495608, -1.500000000000002220 ) ) ;
#56145 = VECTOR ( 'NONE', #51758, 1000.000000000000000 ) ;
#56146 = CARTESIAN_POINT ( 'NONE',  ( -42.60798218881454602, -23.73766607897670156, -1.055555164236442689 ) ) ;
#56147 = CARTESIAN_POINT ( 'NONE',  ( -41.62287095715006302, -23.48786465467240703, 11.44779295918255180 ) ) ;
#56148 = CALENDAR_DATE ( 2026, 9, 10 ) ;
#56149 = CARTESIAN_POINT ( 'NONE',  ( -115.6228709571500275, -23.84047902841603772, -0.8780736468305494480 ) ) ;
#56150 = DIRECTION ( 'NONE',  ( -0.000000000000000000, 1.000000000000000000, -0.000000000000000000 ) ) ;
#56151 = CARTESIAN_POINT ( 'NONE',  ( 17.26003113218828489, 11.23261964116016642, 11.49999999999999645 ) ) ;
#56152 = DIRECTION ( 'NONE',  ( 0.000000000000000000, 0.9999999999976377785, 2.173523156925979975E-06 ) ) ;
#56153 = ADVANCED_FACE ( 'NONE', ( #54011 ), #74975, .T. ) ;
#56154 = CARTESIAN_POINT ( 'NONE',  ( -120.6258288809107029, -24.40034930558991633, 0.3402023900116107336 ) ) ;
#56155 = CARTESIAN_POINT ( 'NONE',  ( -7.157701736792966507, -21.45640540170154509, 11.49999999999999645 ) ) ;
#56156 = ORIENTED_EDGE ( 'NONE', *, *, #90223, .F. ) ;
#56157 = EDGE_CURVE ( 'NONE', #56235, #66681, #17432, .T. ) ;
#56158 = CARTESIAN_POINT ( 'NONE',  ( -100.3574794290996266, -25.31296445282071161, 4.711073526889959062 ) ) ;
#56159 = DIRECTION ( 'NONE',  ( 1.000000000000000000, 0.000000000000000000, 0.000000000000000000 ) ) ;
#56160 = CARTESIAN_POINT ( 'NONE',  ( -97.62356136723437317, -24.65952944569304961, 1.056160979905703456 ) ) ;
#56161 = CARTESIAN_POINT ( 'NONE',  ( -27.40053816590288704, -24.76668234067835783, 2.305505410589911985 ) ) ;
#56162 = CARTESIAN_POINT ( 'NONE',  ( 30.93860345374796594, -5.965225279485572685, 28.07639619989136293 ) ) ;
#56163 = B_SPLINE_CURVE_WITH_KNOTS ( 'NONE', 3,
 ( #52251, #83178, #73590, #50257, #13662, #11673 ),
 .UNSPECIFIED., .F., .F.,
 ( 4, 2, 4 ),
 ( 1.570755371634013412E-05, 0.001396183895866086669, 0.002776660238015832977 ),
 .UNSPECIFIED. ) ;
#56164 = CARTESIAN_POINT ( 'NONE',  ( -125.6228709571500559, -23.47596703998600631, 11.44779298504227860 ) ) ;
#56165 = CIRCLE ( 'NONE', #2710, 7.652410033082763796 ) ;
#56166 = EDGE_LOOP ( 'NONE', ( #33999, #47352, #3792, #99570 ) ) ;
#56167 = CARTESIAN_POINT ( 'NONE',  ( -79.41916052885848387, -25.31596350975968335, 5.559759362272460592 ) ) ;
#56168 = CARTESIAN_POINT ( 'NONE',  ( -2.521034868938843765, 22.70145277337256218, -1.500000000000002220 ) ) ;
#56169 = DIRECTION ( 'NONE',  ( -2.682707457723910108E-15, 0.000000000000000000, -1.000000000000000000 ) ) ;
#56170 = LINE ( 'NONE', #63286, #49594 ) ;
#56171 = CARTESIAN_POINT ( 'NONE',  ( -82.58824230787639920, -24.35071581493543036, 9.817618358456032368 ) ) ;
#56172 = CARTESIAN_POINT ( 'NONE',  ( -11.50411854321151672, 19.32100693743031528, 11.49999999999999645 ) ) ;
#56173 = EDGE_LOOP ( 'NONE', ( #19328, #51082, #2026, #56101 ) ) ;
#56174 = DIRECTION ( 'NONE',  ( 0.8219392559241307517, -0.08114015731558921196, 0.5637660281018073150 ) ) ;
#56175 = CARTESIAN_POINT ( 'NONE',  ( -16.59477544326466969, -14.39948450415919723, 11.49999999999998934 ) ) ;
#56176 = B_SPLINE_CURVE_WITH_KNOTS ( 'NONE', 3,
 ( #38846, #37366, #67824, #100220 ),
 .UNSPECIFIED., .F., .F.,
 ( 4, 4 ),
 ( 0.000000000000000000, 9.999999999998897304E-05 ),
 .UNSPECIFIED. ) ;
#56177 = EDGE_CURVE ( 'NONE', #65451, #90447, #81716, .T. ) ;
#56178 = CARTESIAN_POINT ( 'NONE',  ( -114.5228709571500332, -24.50321055353804667, 9.387540953477513384 ) ) ;
#56179 = CIRCLE ( 'NONE', #36669, 1.249999999999998446 ) ;
#56180 = CARTESIAN_POINT ( 'NONE',  ( -44.54660971391017199, -24.15620529776628089, 10.23563542870660470 ) ) ;
#56181 = CARTESIAN_POINT ( 'NONE',  ( -68.97952899265784765, -25.20747150332676867, 6.546521981683093294 ) ) ;
#56182 = ORIENTED_EDGE ( 'NONE', *, *, #48073, .F. ) ;
#56183 = CARTESIAN_POINT ( 'NONE',  ( -48.58718991420165878, -24.35071581493542681, 9.817618358456027039 ) ) ;
#56184 = CARTESIAN_POINT ( 'NONE',  ( -9.383883476483159569, 17.86611652351680846, 2.100000000000000089 ) ) ;
#56185 = ORIENTED_EDGE ( 'NONE', *, *, #31794, .F. ) ;
#56186 = AXIS2_PLACEMENT_3D ( 'NONE', #53580, #36344, #36846 ) ;
#56187 = CARTESIAN_POINT ( 'NONE',  ( 20.39306652673287701, -2.074774109220689500, 11.49999999999998934 ) ) ;
#56188 = ORIENTED_EDGE ( 'NONE', *, *, #40627, .T. ) ;
#56189 = TOROIDAL_SURFACE ( 'NONE', #48066, 132.8284398600581540, 3.060000000000000053 ) ;
#56190 = ORIENTED_EDGE ( 'NONE', *, *, #43272, .F. ) ;
#56191 = ORIENTED_EDGE ( 'NONE', *, *, #64285, .T. ) ;
#56192 = ORIENTED_EDGE ( 'NONE', *, *, #35149, .F. ) ;
#56193 = CARTESIAN_POINT ( 'NONE',  ( 21.72910700495702230, 7.846448622349001312, 11.49999999999998934 ) ) ;
#56194 = CARTESIAN_POINT ( 'NONE',  ( 22.02124265030973760, 3.456774720514426136, 16.20402280011862217 ) ) ;
#56195 = CARTESIAN_POINT ( 'NONE',  ( 20.34676669208793953, -0.1217515720461415790, -1.500000000000002220 ) ) ;
#56196 = VERTEX_POINT ( 'NONE', #97919 ) ;
#56197 = CARTESIAN_POINT ( 'NONE',  ( -84.52287095715006160, -29.50250243563736774, 8.947779886222141599 ) ) ;
#56198 = CARTESIAN_POINT ( 'NONE',  ( -92.51227642707885934, -24.15543982623908192, -0.2315651400026453588 ) ) ;
#56199 = CIRCLE ( 'NONE', #17279, 0.3000000000000016542 ) ;
#56200 = CARTESIAN_POINT ( 'NONE',  ( 32.73857899460460175, 1.684774720514424118, -13.20677013500359820 ) ) ;
#56201 = CARTESIAN_POINT ( 'NONE',  ( 3.825970207471427020, -5.876774720514403860, 18.52126221587801780 ) ) ;
#56203 = EDGE_LOOP ( 'NONE', ( #97386, #35603, #18502, #19076 ) ) ;
#56202 = CARTESIAN_POINT ( 'NONE',  ( -10.19830463584622571, -18.94658877215714909, 11.49999999999999645 ) ) ;
#56204 = CARTESIAN_POINT ( 'NONE',  ( -75.54003180113411986, -24.73486907724918282, 1.287355809206967683 ) ) ;
#56205 = CARTESIAN_POINT ( 'NONE',  ( -49.59506520832605503, -25.26385825920966610, 4.856709818570129400 ) ) ;
#56206 = ORIENTED_EDGE ( 'NONE', *, *, #71322, .T. ) ;
#56207 = CARTESIAN_POINT ( 'NONE',  ( -10.32638548400381673, 17.97674989526738898, -1.500000000000002220 ) ) ;
#56208 = ORIENTED_EDGE ( 'NONE', *, *, #49467, .F. ) ;
#56210 = EDGE_LOOP ( 'NONE', ( #61453, #53426, #3982, #18379 ) ) ;
#56209 = CARTESIAN_POINT ( 'NONE',  ( -125.5556659931842347, -24.15503026093915295, -0.2815557561904348804 ) ) ;
#56211 = CARTESIAN_POINT ( 'NONE',  ( -4.993225604111834137, -0.3587747205143964613, -29.11654937215279304 ) ) ;
#56212 = CARTESIAN_POINT ( 'NONE',  ( -48.52287095715004739, -24.51283580621457858, 0.6167428607047514832 ) ) ;
#56213 = ORIENTED_EDGE ( 'NONE', *, *, #52487, .T. ) ;
#56214 = ORIENTED_EDGE ( 'NONE', *, *, #45266, .F. ) ;
#56215 = CARTESIAN_POINT ( 'NONE',  ( -5.877732331298974877, -5.876774720514411854, 19.69174559449349005 ) ) ;
#56216 = DIRECTION ( 'NONE',  ( 0.000000000000000000, -2.173523156925979552E-06, 0.9999999999976378895 ) ) ;
#56217 = DIRECTION ( 'NONE',  ( 0.000000000000000000, 1.000000000000000000, 0.000000000000000000 ) ) ;
#56219 = VERTEX_POINT ( 'NONE', #59380 ) ;
#56218 = CARTESIAN_POINT ( 'NONE',  ( -18.71521858236628333, -11.60751834597489740, 11.49999999999999645 ) ) ;
#56220 = CARTESIAN_POINT ( 'NONE',  ( -103.5871832607983976, -24.51314013834315375, 0.6176544820404142877 ) ) ;
#56221 = ADVANCED_FACE ( 'NONE', ( #47895 ), #33155, .T. ) ;
#56222 = CARTESIAN_POINT ( 'NONE',  ( -22.56969522194696509, -0.6267768857631424995, 11.49999999999998934 ) ) ;
#56223 = VECTOR ( 'NONE', #89383, 1000.000000000000114 ) ;
#56224 = CARTESIAN_POINT ( 'NONE',  ( 16.30764028314251846, 13.22082560946828522, 11.49999999999998934 ) ) ;
#56225 = EDGE_CURVE ( 'NONE', #25080, #65405, #76102, .T. ) ;
#56227 = ORIENTED_EDGE ( 'NONE', *, *, #6473, .F. ) ;
#56226 = DIRECTION ( 'NONE',  ( -0.000000000000000000, -0.7071067811865513475, 0.7071067811865437980 ) ) ;
#56228 = B_SPLINE_CURVE_WITH_KNOTS ( 'NONE', 3,
 ( #64976, #49739, #64479, #50724 ),
 .UNSPECIFIED., .F., .F.,
 ( 4, 4 ),
 ( 0.000000000000000000, 1.000000000000000000 ),
 .UNSPECIFIED. ) ;
#56229 = EDGE_CURVE ( 'NONE', #57678, #85295, #71230, .T. ) ;
#56230 = VERTEX_POINT ( 'NONE', #71732 ) ;
#56231 = VECTOR ( 'NONE', #69185, 1000.000000000000000 ) ;
#56232 = EDGE_CURVE ( 'NONE', #88005, #79117, #13201, .T. ) ;
#56233 = PLANE ( 'NONE',  #67728 ) ;
#56234 = DIRECTION ( 'NONE',  ( -3.773278334453080206E-23, 0.9999999999976377785, 2.173523156925979975E-06 ) ) ;
#56235 = VERTEX_POINT ( 'NONE', #12690 ) ;
#56236 = CARTESIAN_POINT ( 'NONE',  ( 13.25904570721172604, 16.46799385432867169, 11.49999999999998934 ) ) ;
#56237 = CARTESIAN_POINT ( 'NONE',  ( -66.62287095715005592, -24.64965695001468404, 8.947790433994184056 ) ) ;
#56238 = CARTESIAN_POINT ( 'NONE',  ( -51.83680534327738343, -25.03148548991196520, 6.675008763280794177 ) ) ;
#56239 = CARTESIAN_POINT ( 'NONE',  ( -75.62287095715004170, -24.91544648472620693, 1.928969306349227919 ) ) ;
#56240 = CARTESIAN_POINT ( 'NONE',  ( -7.234140626586239797, -6.376774720514411854, 19.72789237585158162 ) ) ;
#56241 = CARTESIAN_POINT ( 'NONE',  ( -23.62875734969026453, 6.143225279485574397, 23.50402280011862288 ) ) ;
#56242 = CARTESIAN_POINT ( 'NONE',  ( 19.92104321119709098, 9.795001720801039369, -1.500000000000002220 ) ) ;
#56243 = CARTESIAN_POINT ( 'NONE',  ( -114.6235148628036882, -24.65952944569305316, 1.056160979905706343 ) ) ;
#56244 = EDGE_CURVE ( 'NONE', #63151, #60911, #37516, .T. ) ;
#56245 = VERTEX_POINT ( 'NONE', #36034 ) ;
#56246 = CARTESIAN_POINT ( 'NONE',  ( -112.5228709571501184, -24.34917612407046761, 0.1852690917481127075 ) ) ;
#56247 = CARTESIAN_POINT ( 'NONE',  ( -28.98875734969026041, 5.965225279485572685, 23.37402280011862743 ) ) ;
#56248 = CARTESIAN_POINT ( 'NONE',  ( -8.724563080612403709, -17.33930400145671413, 11.49999999999999645 ) ) ;
#56249 = DIRECTION ( 'NONE',  ( -1.000000000000000000, -3.773278334444166432E-23, -8.201307841325785021E-29 ) ) ;
#56250 = DIRECTION ( 'NONE',  ( 0.000000000000000000, -1.000000000000000000, 0.000000000000000000 ) ) ;
#56251 = B_SPLINE_CURVE_WITH_KNOTS ( 'NONE', 3,
 ( #80552, #65362, #42511, #95283, #97278, #3450, #25768, #96776, #73449, #35391, #56740, #58231, #3942, #27275, #89170, #19643 ),
 .UNSPECIFIED., .F., .F.,
 ( 4, 2, 2, 2, 2, 2, 2, 4 ),
 ( 0.000000000000000000, 0.0002653022231966347061, 0.0005306044463932694123, 0.001061208892786539692, 0.001326511115983166483, 0.001591813339179793492, 0.001857115562376420283, 0.002122417785573047291 ),
 .UNSPECIFIED. ) ;
#56252 = CARTESIAN_POINT ( 'NONE',  ( -18.70048401425367501, 5.426029767813830063, 11.49999999999998934 ) ) ;
#56253 = CARTESIAN_POINT ( 'NONE',  ( 21.39645853268639186, 0.3907444525687319703, -1.500000000000002220 ) ) ;
#56254 = DIRECTION ( 'NONE',  ( 0.000000000000000000, -1.000000000000000000, 0.000000000000000000 ) ) ;
#56255 = CARTESIAN_POINT ( 'NONE',  ( -60.49376913606877793, -24.52399227489757649, 9.353111116819363247 ) ) ;
#56256 = CARTESIAN_POINT ( 'NONE',  ( -51.51436549635971573, -23.73766607897669445, -1.055555164236457788 ) ) ;
#56257 = FACE_OUTER_BOUND ( 'NONE', #43740, .T. ) ;
#56258 = CARTESIAN_POINT ( 'NONE',  ( 10.97283692364161922, -19.94330716608196852, -1.500000000000002220 ) ) ;
#56259 = AXIS2_PLACEMENT_3D ( 'NONE', #35064, #96954, #89349 ) ;
#56260 = VECTOR ( 'NONE', #63571, 1000.000000000000000 ) ;
#56261 = CARTESIAN_POINT ( 'NONE',  ( -106.5874605220203364, -24.51419770103158768, 9.386484678747164523 ) ) ;
#56262 = CYLINDRICAL_SURFACE ( 'NONE', #31369, 1.836000000000000743 ) ;
#56263 = CARTESIAN_POINT ( 'NONE',  ( -16.51628311069853083, -11.03946451426814690, 11.49999999999999645 ) ) ;
#56264 = CARTESIAN_POINT ( 'NONE',  ( 15.32643653063177958, 2.682774720514426559, -27.14485409495429380 ) ) ;
#56265 = VECTOR ( 'NONE', #16376, 1000.000000000000114 ) ;
#56267 = B_SPLINE_CURVE_WITH_KNOTS ( 'NONE', 3,
 ( #59628, #74830, #90560, #14425 ),
 .UNSPECIFIED., .F., .F.,
 ( 4, 4 ),
 ( 0.4000716058185329049, 0.4090780370906481611 ),
 .UNSPECIFIED. ) ;
#56266 = DIRECTION ( 'NONE',  ( 0.000000000000000000, 2.173523156925980399E-06, -0.9999999999976378895 ) ) ;
#56268 = PLANE ( 'NONE',  #37507 ) ;
#56269 = VERTEX_POINT ( 'NONE', #83195 ) ;
#56270 = CARTESIAN_POINT ( 'NONE',  ( -49.74068094892759007, -25.14920433696932633, 6.948203997227099471 ) ) ;
#56271 = CARTESIAN_POINT ( 'NONE',  ( -5.926585084595196840, -6.376774720514415407, 20.19722303762275573 ) ) ;
#56272 = CARTESIAN_POINT ( 'NONE',  ( -51.66021737866784491, -25.27412416137573459, 3.699308556398079428 ) ) ;
#56273 = CARTESIAN_POINT ( 'NONE',  ( -6.031157642910047301, -20.80930661755759203, -1.500000000000002220 ) ) ;
#56274 = CARTESIAN_POINT ( 'NONE',  ( -50.50587993032255696, -25.04358547397666968, 7.560798279822890322 ) ) ;
#56275 = CARTESIAN_POINT ( 'NONE',  ( -3.338044803349280443, -19.22079736023769669, -1.500000000000002220 ) ) ;
#56276 = CARTESIAN_POINT ( 'NONE',  ( -123.6228709571500417, -23.73934037231757799, 11.05740245334328264 ) ) ;
#56277 = EDGE_CURVE ( 'NONE', #56961, #85635, #34971, .T. ) ;
#56278 = ORIENTED_EDGE ( 'NONE', *, *, #84868, .F. ) ;
#56279 = CARTESIAN_POINT ( 'NONE',  ( -8.611577853089924517, -18.50786853157798006, 11.49999999999999645 ) ) ;
#56280 = CARTESIAN_POINT ( 'NONE',  ( 8.160000000000000142, -6.754662360505033547, 7.925641719537452445 ) ) ;
#56281 = EDGE_CURVE ( 'NONE', #49859, #5012, #7581, .T. ) ;
#56282 = CARTESIAN_POINT ( 'NONE',  ( -41.62287095715006302, -23.47593901973091235, -1.443836447539011525 ) ) ;
#56283 = VERTEX_POINT ( 'NONE', #6582 ) ;
#56284 = DIRECTION ( 'NONE',  ( 1.000000000000000000, 0.000000000000000000, 0.000000000000000000 ) ) ;
#56285 = CARTESIAN_POINT ( 'NONE',  ( 33.61752870511805469, 3.456547803086276183, -11.38123630260511199 ) ) ;
#56286 = CARTESIAN_POINT ( 'NONE',  ( -39.04454818115137016, -25.27985276553044969, 4.262458935199855858 ) ) ;
#56287 = CARTESIAN_POINT ( 'NONE',  ( -49.40320226356282518, -25.25138784447102225, 5.711994385046795131 ) ) ;
#56288 = CARTESIAN_POINT ( 'NONE',  ( -86.52287095715001897, -24.51283580621457148, 0.6167428607047598099 ) ) ;
#56289 = B_SPLINE_CURVE_WITH_KNOTS ( 'NONE', 3,
 ( #83073, #21669, #15072, #46040, #74964, #30292 ),
 .UNSPECIFIED., .F., .F.,
 ( 4, 2, 4 ),
 ( 0.000000000000000000, 0.001380901958385387894, 0.002761803916770775788 ),
 .UNSPECIFIED. ) ;
#56290 = CARTESIAN_POINT ( 'NONE',  ( -89.58953762381671027, -24.66019654487199730, 8.947790411086124607 ) ) ;
#56291 = EDGE_LOOP ( 'NONE', ( #84387, #67918, #83121, #35281 ) ) ;
#56292 = CARTESIAN_POINT ( 'NONE',  ( -42.62287095715004881, -24.65952944569303895, 1.056160979905691688 ) ) ;
#56293 = AXIS2_PLACEMENT_3D ( 'NONE', #31233, #38845, #69803 ) ;
#56294 = CARTESIAN_POINT ( 'NONE',  ( -1.334576548209915225, -22.92891363262047832, 11.49999999999999645 ) ) ;
#56295 = CARTESIAN_POINT ( 'NONE',  ( 18.51665531608540860, 13.21585733361752801, 11.49999999999998934 ) ) ;
#56296 = EDGE_LOOP ( 'NONE', ( #80004, #55156, #64931, #89745 ) ) ;
#56297 = CARTESIAN_POINT ( 'NONE',  ( 4.910384361841649614, -6.376774720514420736, 20.73924463800384643 ) ) ;
#56298 = B_SPLINE_SURFACE_WITH_KNOTS ( 'NONE', 3, 1, ( 
 ( #52697, #61324 ),
 ( #84638, #15624 ),
 ( #83636, #13616 ),
 ( #100339, #7514 ),
 ( #92249, #52200 ),
 ( #23227, #38965 ),
 ( #30855, #67934 ),
 ( #98856, #6521 ),
 ( #37966, #44586 ),
 ( #14118, #91250 ),
 ( #76017, #53710 ),
 ( #68423, #68917 ),
 ( #405, #29351 ),
 ( #45592, #85137 ),
 ( #75514, #22720 ),
 ( #29852, #15128 ),
 ( #93248, #99356 ),
 ( #60324, #37473 ),
 ( #21723, #54213 ),
 ( #8016, #53206 ),
 ( #45093, #60823 ),
 ( #83128, #46091 ),
 ( #84135, #7017 ),
 ( #6013, #69420 ),
 ( #14624, #69920 ),
 ( #31356, #91743 ),
 ( #61821, #22225 ) ),
 .UNSPECIFIED., .F., .F., .F.,
 ( 4, 1, 1, 1, 1, 1, 1, 1, 1, 1, 1, 1, 1, 1, 1, 1, 1, 1, 1, 1, 1, 1, 1, 1, 4 ),
 ( 2, 2 ),
 ( 0.000000000000000000, 0.03374242470187671650, 0.06653347536929221651, 0.09915346175681749585, 0.1315397542107091811, 0.1640870483339715857, 0.1965627449807513250, 0.2297068306392113790, 0.2633146464865417924, 0.2975043287136188708, 0.3316856488303484563, 0.3664815111438048945, 0.4020997606356003784, 0.4389576272716395611, 0.4767476992267967173, 0.5159851313836553155, 0.5565892450615084197, 0.5995194112260104902, 0.6457650933466750898, 0.6954865607436527819, 0.7487207768830330679, 0.8056874135317430019, 0.8667539575566982624, 0.9314053777412569790, 1.000000000000000000 ),
 ( 0.000000000000000000, 1.000000000000000000 ),
 .UNSPECIFIED. ) ;
#56299 = CARTESIAN_POINT ( 'NONE',  ( -75.62287095715005592, -24.52323809116984776, 9.355190652339420154 ) ) ;
#56300 = CARTESIAN_POINT ( 'NONE',  ( -123.5228709571501184, -24.66019654487200441, 8.947790411086105067 ) ) ;
#56301 = CIRCLE ( 'NONE', #1232, 2.040000000000000036 ) ;
#56302 = CARTESIAN_POINT ( 'NONE',  ( -30.57287095715006231, -25.26620738237330954, 3.875798415478208359 ) ) ;
#56303 = APPROVAL ( #82561, 'UNSPECIFIED' ) ;
#56304 = FACE_OUTER_BOUND ( 'NONE', #3824, .T. ) ;
#56305 = CARTESIAN_POINT ( 'NONE',  ( -26.99091393574990150, -24.76286136825473250, 2.476735171210982411 ) ) ;
#56306 = CARTESIAN_POINT ( 'NONE',  ( -76.92287095715005307, -23.47596703998600631, 11.44779298504227860 ) ) ;
#56307 = CARTESIAN_POINT ( 'NONE',  ( -34.58953762381672448, -24.65952944569304250, 1.056160979905690134 ) ) ;
#56308 = EDGE_LOOP ( 'NONE', ( #17121, #74630, #58301, #83232, #41145 ) ) ;
#56309 = PRODUCT_DEFINITION_SHAPE ( 'NONE', 'NONE',  #70488 ) ;
#56310 = CARTESIAN_POINT ( 'NONE',  ( -10.90597124047809530, 17.21661415904998904, 11.49999999999998934 ) ) ;
#56311 = VERTEX_POINT ( 'NONE', #13683 ) ;
#56312 = ORIENTED_EDGE ( 'NONE', *, *, #37587, .F. ) ;
#56313 = CARTESIAN_POINT ( 'NONE',  ( -22.55714481399219906, -4.634528848986672500, 11.49999999999998934 ) ) ;
#56314 = CARTESIAN_POINT ( 'NONE',  ( -1.318699232124953324, -6.376774720514411854, 19.74039977944280722 ) ) ;
#56316 = ORIENTED_EDGE ( 'NONE', *, *, #78278, .F. ) ;
#56315 = ADVANCED_FACE ( 'NONE', ( #91812 ), #13182, .F. ) ;
#56317 = DIRECTION ( 'NONE',  ( 0.000000000000000000, 0.000000000000000000, -1.000000000000000000 ) ) ;
#56318 = CARTESIAN_POINT ( 'NONE',  ( -32.52287095715004739, -24.34917612407030774, 0.1852690917476929044 ) ) ;
#56319 = CARTESIAN_POINT ( 'NONE',  ( -95.59440297368489325, -24.15503026093913874, -0.2815557561904519224 ) ) ;
#56320 = FACE_OUTER_BOUND ( 'NONE', #58315, .T. ) ;
#56322 = ORIENTED_EDGE ( 'NONE', *, *, #31110, .T. ) ;
#56321 = CARTESIAN_POINT ( 'NONE',  ( -14.93283513470682067, -15.21490397768744529, 11.49999999999999645 ) ) ;
#56323 = ORIENTED_EDGE ( 'NONE', *, *, #2603, .T. ) ;
#56324 = CARTESIAN_POINT ( 'NONE',  ( -19.85906585229243504, 9.992431322412627992, 11.49999999999998934 ) ) ;
#56325 = CARTESIAN_POINT ( 'NONE',  ( 20.50092990308456464, -2.467789585553555654, 11.49999999999998934 ) ) ;
#56326 = AXIS2_PLACEMENT_3D ( 'NONE', #85493, #45954, #55565 ) ;
#56327 = ORIENTED_EDGE ( 'NONE', *, *, #70427, .T. ) ;
#56328 = CARTESIAN_POINT ( 'NONE',  ( -125.5228709571500616, -29.50248528299804818, 1.056150453629047137 ) ) ;
#56329 = CARTESIAN_POINT ( 'NONE',  ( -71.72497398431139004, -25.25978459231412288, 3.590539514744167437 ) ) ;
#56330 = ORIENTED_EDGE ( 'NONE', *, *, #19760, .T. ) ;
#56331 = CARTESIAN_POINT ( 'NONE',  ( -95.52287095715004739, -23.84047902841604127, -0.8780736468305392339 ) ) ;
#56332 = VECTOR ( 'NONE', #24377, 1000.000000000000114 ) ;
#56333 = ORIENTED_EDGE ( 'NONE', *, *, #26175, .F. ) ;
#56334 = CARTESIAN_POINT ( 'NONE',  ( -58.59294932955677382, -24.15620529776628089, 10.23563542870660470 ) ) ;
#56335 = CARTESIAN_POINT ( 'NONE',  ( 11.03981094302168842, 0.3587747205144256601, -28.06140118199223465 ) ) ;
#56336 = CARTESIAN_POINT ( 'NONE',  ( -20.82246440549779720, 1.468558417816581807, -1.500000000000002220 ) ) ;
#56337 = ADVANCED_FACE ( 'NONE', ( #44152 ), #45651, .F. ) ;
#56338 = CARTESIAN_POINT ( 'NONE',  ( 19.20967809413044236, -10.42350525531561978, 11.49999999999999645 ) ) ;
#56339 = CARTESIAN_POINT ( 'NONE',  ( -37.52287095715006870, -24.64898659630367206, 1.056161002820819261 ) ) ;
#56340 = DIRECTION ( 'NONE',  ( -1.000000000000000000, -3.491481338843133355E-15, -2.352173255807796056E-16 ) ) ;
#56341 = CARTESIAN_POINT ( 'NONE',  ( -18.88510386880526326, 12.19974334031638641, 11.49999999999998934 ) ) ;
#56342 = CARTESIAN_POINT ( 'NONE',  ( -38.59385446322277602, -24.15543982623906771, -0.2315651400026570161 ) ) ;
#56343 = DIRECTION ( 'NONE',  ( -1.000000000000000000, 0.000000000000000000, 0.000000000000000000 ) ) ;
#56344 = CARTESIAN_POINT ( 'NONE',  ( 4.115044103975469270, -5.876774720514427841, 21.79213183355573946 ) ) ;
#56345 = ORIENTED_EDGE ( 'NONE', *, *, #9303, .T. ) ;
#56346 = ADVANCED_FACE ( 'NONE', ( #68981 ), #75087, .F. ) ;
#56347 = ORIENTED_EDGE ( 'NONE', *, *, #62216, .F. ) ;
#56348 = ORIENTED_EDGE ( 'NONE', *, *, #50464, .T. ) ;
#56349 = ADVANCED_FACE ( 'NONE', ( #59890 ), #44635, .T. ) ;
#56350 = CARTESIAN_POINT ( 'NONE',  ( -52.63306204174769221, -24.34968618360933945, 0.1864209137778880532 ) ) ;
#56351 = VERTEX_POINT ( 'NONE', #76083 ) ;
#56352 = CARTESIAN_POINT ( 'NONE',  ( 18.99370601119529312, 9.851043883551550806, -1.500000000000002220 ) ) ;
#56353 = CARTESIAN_POINT ( 'NONE',  ( -16.90645664988545249, 14.66980924573920397, 11.49999999999999645 ) ) ;
#56354 = ORIENTED_EDGE ( 'NONE', *, *, #48087, .F. ) ;
#56355 = CARTESIAN_POINT ( 'NONE',  ( -68.52287095715006160, -24.65952944569304606, 1.056160979905697239 ) ) ;
#56356 = CARTESIAN_POINT ( 'NONE',  ( -20.60145385712877797, -4.430719527714695793, -1.500000000000002220 ) ) ;
#56357 = CARTESIAN_POINT ( 'NONE',  ( -30.58829336780489072, -23.48332523652080539, 11.44779287168131710 ) ) ;
#56358 = CARTESIAN_POINT ( 'NONE',  ( 14.81759351585047391, 13.34335055255382052, -1.500000000000002220 ) ) ;
#56359 =( REPRESENTATION_RELATIONSHIP ('NONE','NONE', #96270, #91803 ) REPRESENTATION_RELATIONSHIP_WITH_TRANSFORMATION ( #16055 )SHAPE_REPRESENTATION_RELATIONSHIP( ) );
#56360 = CARTESIAN_POINT ( 'NONE',  ( -113.6228709571500559, -23.47593901973091235, -1.443836447538999312 ) ) ;
#56361 = CARTESIAN_POINT ( 'NONE',  ( -101.5528341795800316, -24.15543982623907482, -0.2315651400026588758 ) ) ;
#56362 = CARTESIAN_POINT ( 'NONE',  ( -20.26759042640731323, -8.618136523154847239, -1.500000000000002220 ) ) ;
#56363 = ORIENTED_EDGE ( 'NONE', *, *, #83668, .F. ) ;
#56364 = CARTESIAN_POINT ( 'NONE',  ( -116.5185805412094311, -24.15543982623908548, -0.2315651400026407236 ) ) ;
#56365 = EDGE_CURVE ( 'NONE', #86751, #17712, #68486, .T. ) ;
#56366 = DIRECTION ( 'NONE',  ( -3.773278334453079618E-23, 0.9999999999976377785, 2.173523156925979975E-06 ) ) ;
#56367 = CARTESIAN_POINT ( 'NONE',  ( -20.64841573231975147, 3.066018724555340746, 11.49999999999999645 ) ) ;
#56368 = AXIS2_PLACEMENT_3D ( 'NONE', #1294, #2299, #78891 ) ;
#56369 = CARTESIAN_POINT ( 'NONE',  ( -62.49922300485171434, -24.35071581493542681, 9.817618358456032368 ) ) ;
#56370 = CARTESIAN_POINT ( 'NONE',  ( -125.5228709571500616, -24.62285846331435835, 9.038163153548284257 ) ) ;
#56371 = CARTESIAN_POINT ( 'NONE',  ( -117.5228709571500900, -23.96127896941632685, -0.6493128931037944751 ) ) ;
#56372 = CARTESIAN_POINT ( 'NONE',  ( -11.06822068739258391, -18.21809710261049275, -1.500000000000002220 ) ) ;
#56373 = CARTESIAN_POINT ( 'NONE',  ( 6.150000000000003908, 1.999999999999998224, 19.19609335255483629 ) ) ;
#56374 = CARTESIAN_POINT ( 'NONE',  ( 30.53060340732036337, 5.297812262124996785, 1.539714685317421505 ) ) ;
#56375 = CARTESIAN_POINT ( 'NONE',  ( -96.52287095715009002, -23.96177878511310055, 10.65340807706329507 ) ) ;
#56376 = CARTESIAN_POINT ( 'NONE',  ( -5.574014511416001127, -5.876774720514415407, 20.24089781925592391 ) ) ;
#56377 = CARTESIAN_POINT ( 'NONE',  ( 22.54279463279464579, 0.6884863543687869125, -1.500000000000002220 ) ) ;
#56378 = B_SPLINE_SURFACE_WITH_KNOTS ( 'NONE', 3, 1, ( 
 ( #88780, #79646 ),
 ( #94872, #2543 ),
 ( #49726, #12130 ),
 ( #19246, #64966 ),
 ( #73547, #3543 ),
 ( #64468, #56842 ),
 ( #63964, #87774 ),
 ( #18256, #65960 ),
 ( #95877, #81156 ),
 ( #57344, #43102 ),
 ( #74046, #88277 ) ),
 .UNSPECIFIED., .F., .F., .F.,
 ( 4, 1, 1, 1, 1, 1, 1, 1, 4 ),
 ( 2, 2 ),
 ( 0.000000000000000000, 0.1105883385953354281, 0.2245417540535955825, 0.3425034940501039959, 0.4643240984173586106, 0.5907560327017663537, 0.7222274753555145699, 0.8588428362087243695, 1.000000000000000000 ),
 ( 0.000000000000000000, 1.000000000000000000 ),
 .UNSPECIFIED. ) ;
#56379 = CARTESIAN_POINT ( 'NONE',  ( -123.5228709571500616, -24.64898659630368627, 1.056161002820833028 ) ) ;
#56380 = ORIENTED_EDGE ( 'NONE', *, *, #80360, .T. ) ;
#56381 = CARTESIAN_POINT ( 'NONE',  ( 6.646494591716556322, 3.316774720514426900, -28.33840132637671161 ) ) ;
#56382 = CARTESIAN_POINT ( 'NONE',  ( -31.61990752757089140, -23.48786465467240347, 11.44779295918255535 ) ) ;
#56383 = CARTESIAN_POINT ( 'NONE',  ( -3.718233408413001762, 19.32670252783854536, 11.49999999999999645 ) ) ;
#56384 = CARTESIAN_POINT ( 'NONE',  ( -49.52287095715007581, -23.47593901973090169, -1.443836447538997092 ) ) ;
#56385 = LINE ( 'NONE', #87307, #67479 ) ;
#56386 = ORIENTED_EDGE ( 'NONE', *, *, #99154, .T. ) ;
#56387 = CARTESIAN_POINT ( 'NONE',  ( -89.52287095715000476, -24.33927499327855060, 9.819080762295811837 ) ) ;
#56388 = CARTESIAN_POINT ( 'NONE',  ( -55.62287095715002749, -24.51163499207175533, 0.6490370598554264792 ) ) ;
#56389 = CARTESIAN_POINT ( 'NONE',  ( -124.6242025155618478, -24.35071581493544457, 9.817618358456016381 ) ) ;
#56390 = CARTESIAN_POINT ( 'NONE',  ( 17.51792015816173986, -0.3587747205144265483, 29.01255224319336889 ) ) ;
#56391 = TOROIDAL_SURFACE ( 'NONE', #82291, 19.00000000000000000, 1.000000000000000000 ) ;
#56392 = LINE ( 'NONE', #72605, #10691 ) ;
#56393 = CARTESIAN_POINT ( 'NONE',  ( -48.62287095715004881, -29.50250243563736774, 8.947779886222146928 ) ) ;
#56394 = CARTESIAN_POINT ( 'NONE',  ( 8.221391366598689743, 17.94232518691122635, -1.500000000000002220 ) ) ;
#56395 = ORIENTED_EDGE ( 'NONE', *, *, #86690, .F. ) ;
#56396 = B_SPLINE_CURVE_WITH_KNOTS ( 'NONE', 3,
 ( #4246, #41821, #28081, #4743, #74734, #98064, #67156, #97086, #3261, #89476, #80868, #18959, #96583, #73748, #28571, #5234, #59531, #72766 ),
 .UNSPECIFIED., .F., .F.,
 ( 4, 2, 2, 2, 2, 2, 2, 2, 4 ),
 ( 0.000000000000000000, 0.0002842996626774647244, 0.0005685993253549294487, 0.0008528989880323941189, 0.001137198650709858897, 0.001421498313387323676, 0.001705797976064788238, 0.001990097638742253233, 0.002274397301419717795 ),
 .UNSPECIFIED. ) ;
#56397 = CARTESIAN_POINT ( 'NONE',  ( -5.512817753899047268, 19.46650688538001361, 11.49999999999999645 ) ) ;
#56398 = CARTESIAN_POINT ( 'NONE',  ( 14.02639803017889086, 6.376774720514426065, -25.20535965011783119 ) ) ;
#56399 = AXIS2_PLACEMENT_3D ( 'NONE', #67554, #42726, #37087 ) ;
#56400 = EDGE_CURVE ( 'NONE', #57117, #27752, #11959, .T. ) ;
#56401 = ORIENTED_EDGE ( 'NONE', *, *, #86105, .F. ) ;
#56402 = CARTESIAN_POINT ( 'NONE',  ( -115.6228709571500559, -23.48786465467242479, 11.44779295918253759 ) ) ;
#56403 = CARTESIAN_POINT ( 'NONE',  ( -72.58953762381672448, -23.47596703998600276, 11.44779298504227683 ) ) ;
#56404 = DIRECTION ( 'NONE',  ( -1.000000000000000000, 0.000000000000000000, 0.000000000000000000 ) ) ;
#56405 = DIRECTION ( 'NONE',  ( -0.000000000000000000, 1.000000000000000000, -0.000000000000000000 ) ) ;
#56406 = VECTOR ( 'NONE', #55063, 1000.000000000000000 ) ;
#56407 = CARTESIAN_POINT ( 'NONE',  ( 9.402885806365684829, -0.3587747205144265483, 29.04108526060719342 ) ) ;
#56408 = CARTESIAN_POINT ( 'NONE',  ( -86.58953762381671027, -24.66019654487199730, 8.947790411086121054 ) ) ;
#56409 = CARTESIAN_POINT ( 'NONE',  ( -19.87929632332335927, 2.386914507623989490, 11.49999999999998934 ) ) ;
#56410 = LINE ( 'NONE', #78695, #54797 ) ;
#56411 = CARTESIAN_POINT ( 'NONE',  ( -87.62287095715004170, -29.50248528299804818, 1.056150453629040253 ) ) ;
#56412 = ORIENTED_EDGE ( 'NONE', *, *, #35938, .F. ) ;
#56413 = B_SPLINE_CURVE_WITH_KNOTS ( 'NONE', 3,
 ( #95743, #65329, #73415, #58193 ),
 .UNSPECIFIED., .F., .F.,
 ( 4, 4 ),
 ( 0.000000000000000000, 9.999999999998897304E-05 ),
 .UNSPECIFIED. ) ;
#56414 = CARTESIAN_POINT ( 'NONE',  ( -79.54656511345403658, -24.35071581493543036, 9.817618358456028815 ) ) ;
#56415 = CARTESIAN_POINT ( 'NONE',  ( 0.000000000000000000, 1.682774720514426114, -1.352392034746782823 ) ) ;
#56416 = CARTESIAN_POINT ( 'NONE',  ( -100.5228709571500616, -24.99156044556120904, 7.747789690856173195 ) ) ;
#56417 = CARTESIAN_POINT ( 'NONE',  ( -116.4728709570019731, -25.40556190190858032, 4.804048521347548117 ) ) ;
#56418 = CARTESIAN_POINT ( 'NONE',  ( -73.55905801038284153, -23.73766607897670511, -1.055555164236457344 ) ) ;
#56419 = EDGE_CURVE ( 'NONE', #26998, #59330, #8081, .T. ) ;
#56420 = CARTESIAN_POINT ( 'NONE',  ( 14.43441819135533777, 3.316774720514426900, -28.36222020317639192 ) ) ;
#56421 = CARTESIAN_POINT ( 'NONE',  ( -100.9375798325987716, -25.25978491487772004, 3.590542621692357717 ) ) ;
#56422 = ORIENTED_EDGE ( 'NONE', *, *, #18510, .F. ) ;
#56423 = EDGE_CURVE ( 'NONE', #9985, #15254, #93817, .T. ) ;
#56424 = CARTESIAN_POINT ( 'NONE',  ( 14.61151973098085222, 14.07909450314327771, -1.500000000000002220 ) ) ;
#56425 = CARTESIAN_POINT ( 'NONE',  ( -7.160000000000000142, -6.754662360505034435, 7.925641719537454222 ) ) ;
#56426 = CARTESIAN_POINT ( 'NONE',  ( -127.5558934889587448, -23.96169478059714208, 10.65365249895716282 ) ) ;
#56427 = EDGE_CURVE ( 'NONE', #24488, #70415, #31926, .T. ) ;
#56428 = CARTESIAN_POINT ( 'NONE',  ( -59.53835329446878433, -24.51419770103156281, 9.386484678747184063 ) ) ;
#56429 = ADVANCED_FACE ( 'NONE', ( #24306 ), #54275, .T. ) ;
#56430 = CARTESIAN_POINT ( 'NONE',  ( 31.44923352942285177, -5.094381739198088788, -4.378347922178638107 ) ) ;
#56431 = DIRECTION ( 'NONE',  ( 0.000000000000000000, -0.000000000000000000, -1.000000000000000000 ) ) ;
#56432 = CARTESIAN_POINT ( 'NONE',  ( 9.152908845159860363, 19.05633030926415472, 11.49999999999999645 ) ) ;
#56433 = EDGE_CURVE ( 'NONE', #15795, #76129, #61886, .T. ) ;
#56434 = CARTESIAN_POINT ( 'NONE',  ( 5.777647480883832287, 21.37485705712154171, -1.500000000000002220 ) ) ;
#56435 = CARTESIAN_POINT ( 'NONE',  ( -20.44794078217315558, 2.270689272194197805, -1.500000000000002220 ) ) ;
#56436 = EDGE_LOOP ( 'NONE', ( #39550, #100332, #65045, #74306 ) ) ;
#56437 = CARTESIAN_POINT ( 'NONE',  ( 1.876957540558651605, -5.558144974487054135, 0.000000000000000000 ) ) ;
#56438 = VERTEX_POINT ( 'NONE', #32423 ) ;
#56439 = CARTESIAN_POINT ( 'NONE',  ( -70.62287095715005592, -29.50247984919015209, -1.443849546365055359 ) ) ;
#56440 = DIRECTION ( 'NONE',  ( 0.000000000000000000, 0.000000000000000000, 1.000000000000000000 ) ) ;
#56441 = EDGE_LOOP ( 'NONE', ( #51294, #62100, #63834, #29730 ) ) ;
#56442 = ORIENTED_EDGE ( 'NONE', *, *, #4776, .T. ) ;
#56443 = ORIENTED_EDGE ( 'NONE', *, *, #29059, .T. ) ;
#56444 = CARTESIAN_POINT ( 'NONE',  ( -81.62287095715012697, -23.95044443724992789, 10.65354141964649592 ) ) ;
#56445 = CARTESIAN_POINT ( 'NONE',  ( -55.58953762381671737, -24.99156044556120193, 7.747789690856344613 ) ) ;
#56446 = CARTESIAN_POINT ( 'NONE',  ( -55.52287095715006870, -29.50250786944525672, 11.44777988621623876 ) ) ;
#56447 = CARTESIAN_POINT ( 'NONE',  ( -19.59449498831206782, -6.737714454370689054, -1.500000000000002220 ) ) ;
#56448 = ADVANCED_FACE ( 'NONE', ( #63395 ), #24798, .T. ) ;
#56449 = CARTESIAN_POINT ( 'NONE',  ( 20.55956107658784404, -6.795330137259728787, 11.49999999999999645 ) ) ;
#56450 = VERTEX_POINT ( 'NONE', #55273 ) ;
#56451 = CARTESIAN_POINT ( 'NONE',  ( -110.6228709571500559, -25.00158670708909625, 2.256160236439165967 ) ) ;
#56452 = LINE ( 'NONE', #78746, #7483 ) ;
#56453 = CARTESIAN_POINT ( 'NONE',  ( 0.2029947971921062799, -22.41465419638480228, -1.500000000000002220 ) ) ;
#56454 = VECTOR ( 'NONE', #14057, 1000.000000000000114 ) ;
#56455 = CARTESIAN_POINT ( 'NONE',  ( -47.56853656710128320, -23.48786465467240347, 11.44779295918255002 ) ) ;
#56456 = CARTESIAN_POINT ( 'NONE',  ( -102.5228709571501042, -24.35013146730204170, 9.818937971375097717 ) ) ;
#56457 = ORIENTED_EDGE ( 'NONE', *, *, #67198, .F. ) ;
#56458 = CARTESIAN_POINT ( 'NONE',  ( -31.62287095715005947, -24.51387760970723662, 9.387446482453421837 ) ) ;
#56459 = CARTESIAN_POINT ( 'NONE',  ( -35.64594292568924772, -24.40133493613049609, 9.663955038902800609 ) ) ;
#56460 = ORIENTED_EDGE ( 'NONE', *, *, #29430, .T. ) ;
#56461 = ORIENTED_EDGE ( 'NONE', *, *, #35399, .F. ) ;
#56463 = EDGE_CURVE ( 'NONE', #64065, #86743, #93307, .T. ) ;
#56462 = CARTESIAN_POINT ( 'NONE',  ( -109.9228709571500531, -23.47596703998600631, 11.44779298504227860 ) ) ;
#56464 = EDGE_LOOP ( 'NONE', ( #10730, #54369, #97275, #12646 ) ) ;
#56465 = FACE_OUTER_BOUND ( 'NONE', #75648, .T. ) ;
#56466 = CARTESIAN_POINT ( 'NONE',  ( 17.81766572339076404, -11.58780717566545526, -1.500000000000002220 ) ) ;
#56467 = EDGE_CURVE ( 'NONE', #35231, #83907, #55777, .T. ) ;
#56468 = ORIENTED_EDGE ( 'NONE', *, *, #69398, .T. ) ;
#56469 = FACE_OUTER_BOUND ( 'NONE', #47107, .T. ) ;
#56470 = CARTESIAN_POINT ( 'NONE',  ( 6.711561834375728175, -20.75310922853297058, 11.49999999999998934 ) ) ;
#56471 = CARTESIAN_POINT ( 'NONE',  ( -103.5574460374484289, -23.73791477778911840, 11.05961554403170410 ) ) ;
#56472 = AXIS2_PLACEMENT_3D ( 'NONE', #94441, #73616, #80224 ) ;
#56473 = FACE_BOUND ( 'NONE', #20868, .T. ) ;
#56474 = CARTESIAN_POINT ( 'NONE',  ( -35.52287095715006870, -24.99156044556120193, 7.747789690856173195 ) ) ;
#56475 = CARTESIAN_POINT ( 'NONE',  ( -18.33957545910867282, 11.93505917737106259, -1.500000000000002220 ) ) ;
#56476 = CARTESIAN_POINT ( 'NONE',  ( -30.57287095715007297, -24.48748619694336881, 9.410756961485560623 ) ) ;
#56477 = VERTEX_POINT ( 'NONE', #47658 ) ;
#56478 = CARTESIAN_POINT ( 'NONE',  ( -69.62287095715004170, -23.96127896941632685, -0.6493128931037859264 ) ) ;
#56479 = B_SPLINE_CURVE_WITH_KNOTS ( 'NONE', 3,
 ( #2110, #16810, #25427, #8709, #64528, #10207, #33544, #47775 ),
 .UNSPECIFIED., .F., .F.,
 ( 4, 2, 2, 4 ),
 ( 1.390486644391990834E-17, 0.0002557425425658982343, 0.0005114850851317825908, 0.001022970170263591419 ),
 .UNSPECIFIED. ) ;
#56480 = CARTESIAN_POINT ( 'NONE',  ( -85.50609027866678957, -24.40133493613049964, 9.663955038902802386 ) ) ;
#56482 = ORIENTED_EDGE ( 'NONE', *, *, #49730, .F. ) ;
#56481 = ADVANCED_FACE ( 'NONE', ( #79592 ), #10084, .F. ) ;
#56483 = EDGE_CURVE ( 'NONE', #80790, #20207, #39810, .T. ) ;
#56484 = VERTEX_POINT ( 'NONE', #465 ) ;
#56485 = EDGE_CURVE ( 'NONE', #94122, #79731, #32925, .T. ) ;
#56486 = VECTOR ( 'NONE', #8591, 1000.000000000000114 ) ;
#56487 = ORIENTED_EDGE ( 'NONE', *, *, #52029, .T. ) ;
#56488 = CARTESIAN_POINT ( 'NONE',  ( -83.52287095715007581, -23.48783264082477018, -1.443836473390090802 ) ) ;
#56489 = CARTESIAN_POINT ( 'NONE',  ( -82.54713402157328517, -24.34968618360933945, 0.1864209137778926328 ) ) ;
#56490 = CARTESIAN_POINT ( 'NONE',  ( 12.23393567461250697, 17.36540613969008007, 11.49999999999998934 ) ) ;
#56491 = FACE_OUTER_BOUND ( 'NONE', #64236, .T. ) ;
#56492 = CARTESIAN_POINT ( 'NONE',  ( -130.5728709571500588, -24.77158516743338623, 8.907023374642852431 ) ) ;
#56493 = CARTESIAN_POINT ( 'NONE',  ( 29.73860345376319714, 4.772774720514425972, -4.021250162519585558 ) ) ;
#56494 = CARTESIAN_POINT ( 'NONE',  ( -99.52287095715010423, -23.94994826722565406, -0.6494450866342716955 ) ) ;
#56495 = CARTESIAN_POINT ( 'NONE',  ( 19.38287969867323213, 0.6573286442255052986, 11.49999999999998934 ) ) ;
#56496 = CARTESIAN_POINT ( 'NONE',  ( -45.47440205232901889, -24.92564183028978775, 1.928384488918256645 ) ) ;
#56497 = ORIENTED_EDGE ( 'NONE', *, *, #59124, .F. ) ;
#56498 = CARTESIAN_POINT ( 'NONE',  ( 18.45204572605500104, 6.281640480902235701, 11.49999999999999645 ) ) ;
#56499 = CARTESIAN_POINT ( 'NONE',  ( -5.000686017310577824, -6.376774720514411854, 19.46274624311237034 ) ) ;
#56500 = PLANE ( 'NONE',  #54431 ) ;
#56501 = VERTEX_POINT ( 'NONE', #16187 ) ;
#56502 = CARTESIAN_POINT ( 'NONE',  ( 4.638796026491669444, -6.376774720514424288, 21.40644651702305268 ) ) ;
#56503 = DIRECTION ( 'NONE',  ( 0.000000000000000000, 0.000000000000000000, -1.000000000000000000 ) ) ;
#56504 = CARTESIAN_POINT ( 'NONE',  ( -90.52287095715006160, -24.15431212366388181, -0.2830839119429129913 ) ) ;
#56505 = CYLINDRICAL_SURFACE ( 'NONE', #80185, 1.325999999999943446 ) ;
#56506 = CARTESIAN_POINT ( 'NONE',  ( 19.58216393897113505, 1.562425146961006650, 11.49999999999998934 ) ) ;
#56507 = ORIENTED_EDGE ( 'NONE', *, *, #63892, .T. ) ;
#56508 = DIRECTION ( 'NONE',  ( -1.000000000000000000, -3.773278334444167608E-23, -8.201307833595939069E-29 ) ) ;
#56509 = CARTESIAN_POINT ( 'NONE',  ( 11.81885653190370888, -19.86314957129924608, -1.500000000000002220 ) ) ;
#56510 = PERSON_AND_ORGANIZATION_ROLE ( 'creator' ) ;
#56511 = CARTESIAN_POINT ( 'NONE',  ( -106.5228709571500758, -24.64965694238408034, 8.947790433994192938 ) ) ;
#56512 = DIRECTION ( 'NONE',  ( -1.000000000000000000, 0.000000000000000000, 5.238131417152343399E-15 ) ) ;
#56513 = CARTESIAN_POINT ( 'NONE',  ( -115.6228709571500417, -25.00182538069145721, 7.747789668545097541 ) ) ;
#56514 = DIRECTION ( 'NONE',  ( -3.773278334453079618E-23, 0.9999999999976377785, 2.173523156925979975E-06 ) ) ;
#56515 = CARTESIAN_POINT ( 'NONE',  ( -79.92244018840227682, -25.03722721891040948, 7.590183713343858329 ) ) ;
#56516 = AXIS2_PLACEMENT_3D ( 'NONE', #30493, #46732, #77658 ) ;
#56517 = CARTESIAN_POINT ( 'NONE',  ( -44.52287095715004028, -23.73907113216988307, -1.053371485793254347 ) ) ;
#56518 = DIRECTION ( 'NONE',  ( -1.257682986112628661E-16, 0.000000000000000000, -1.000000000000000000 ) ) ;
#56519 = DIRECTION ( 'NONE',  ( -0.000000000000000000, -1.000000000000000000, -0.000000000000000000 ) ) ;
#56520 = CARTESIAN_POINT ( 'NONE',  ( -16.62890364678930410, -10.96057169749504645, 11.49999999999998934 ) ) ;
#56521 = CARTESIAN_POINT ( 'NONE',  ( -75.58919500596368835, -24.52399227489127043, 9.353111116836526406 ) ) ;
#56522 = CARTESIAN_POINT ( 'NONE',  ( -10.02925392579303576, -17.20239368982820238, -1.500000000000002220 ) ) ;
#56523 = VERTEX_POINT ( 'NONE', #79083 ) ;
#56524 = VECTOR ( 'NONE', #17349, 1000.000000000000000 ) ;
#56525 = CARTESIAN_POINT ( 'NONE',  ( -122.5228709571500616, -23.47596703998600631, 11.44779298504227860 ) ) ;
#56526 = CARTESIAN_POINT ( 'NONE',  ( -101.6228709571500559, -24.64898659630368627, 1.056161002820829697 ) ) ;
#56527 = CARTESIAN_POINT ( 'NONE',  ( -35.62287095715007013, -24.14406661707770496, 10.28769366152060982 ) ) ;
#56528 = CARTESIAN_POINT ( 'NONE',  ( 18.03836333725549324, -10.36167025447706713, 11.49999999999999645 ) ) ;
#56529 = CARTESIAN_POINT ( 'NONE',  ( -6.818021687177533430, -5.876774720514408301, 19.14905311829361167 ) ) ;
#56530 = AXIS2_PLACEMENT_3D ( 'NONE', #56659, #32806, #63784 ) ;
#56531 = CARTESIAN_POINT ( 'NONE',  ( -106.5562042904834072, -24.66019654487199730, 8.947790411086124607 ) ) ;
#56532 = CARTESIAN_POINT ( 'NONE',  ( 17.57702471007113232, 14.52005670271990034, 11.49999999999999645 ) ) ;
#56534 = EDGE_CURVE ( 'NONE', #80860, #81148, #2268, .T. ) ;
#56533 = ORIENTED_EDGE ( 'NONE', *, *, #73141, .F. ) ;
#56535 = LINE ( 'NONE', #9838, #70546 ) ;
#56536 = CARTESIAN_POINT ( 'NONE',  ( -127.6248233915099917, -23.48783264082477018, -1.443836473390083919 ) ) ;
#56537 = ORIENTED_EDGE ( 'NONE', *, *, #60097, .F. ) ;
#56538 = CIRCLE ( 'NONE', #67839, 6.594667762285751245 ) ;
#56539 = CARTESIAN_POINT ( 'NONE',  ( -19.33604739795523741, 5.927148246271303655, -1.500000000000002220 ) ) ;
#56540 = CARTESIAN_POINT ( 'NONE',  ( 7.403636664866980688, -5.876774720514424288, 21.18544102487025782 ) ) ;
#56541 = CARTESIAN_POINT ( 'NONE',  ( -10.24059822343757808, -5.876774720514426953, 22.08128695274315945 ) ) ;
#56542 = EDGE_CURVE ( 'NONE', #55431, #57803, #64324, .T. ) ;
#56543 = EDGE_CURVE ( 'NONE', #77715, #40322, #17695, .T. ) ;
#56544 = CARTESIAN_POINT ( 'NONE',  ( -84.52287095715004739, -23.94994826722565406, -0.6494450866342729167 ) ) ;
#56545 = EDGE_CURVE ( 'NONE', #57700, #11900, #89423, .T. ) ;
#56546 = VERTEX_POINT ( 'NONE', #42552 ) ;
#56547 = CARTESIAN_POINT ( 'NONE',  ( -0.1469190486835098564, -21.14801745985730719, -1.461890965025842704 ) ) ;
#56548 = LINE ( 'NONE', #49434, #66540 ) ;
#56549 = CARTESIAN_POINT ( 'NONE',  ( -7.473237707827510512, 18.53023608995856009, -1.500000000000002220 ) ) ;
#56550 = CARTESIAN_POINT ( 'NONE',  ( 31.41423154468143153, -2.682774720514426559, -0.3119954678742140053 ) ) ;
#56551 = CARTESIAN_POINT ( 'NONE',  ( 16.30764028314251846, 13.22082560946828522, 11.49999999999999645 ) ) ;
#56552 = ADVANCED_FACE ( 'NONE', ( #11084 ), #57772, .F. ) ;
#56553 = DIRECTION ( 'NONE',  ( 0.7071067811865476838, 0.000000000000000000, -0.7071067811865474617 ) ) ;
#56554 = CARTESIAN_POINT ( 'NONE',  ( -70.53235729249159647, -25.00182538069146787, 7.747789668545044250 ) ) ;
#56555 = CARTESIAN_POINT ( 'NONE',  ( -10.28628152547328511, -19.52461415289770130, 11.49999999999998934 ) ) ;
#56556 = LINE ( 'NONE', #71769, #36528 ) ;
#56557 = EDGE_LOOP ( 'NONE', ( #69433, #24842, #8588, #377 ) ) ;
#56558 = CARTESIAN_POINT ( 'NONE',  ( -28.98875734969026396, -5.965225279485572685, 2.362022800118626531 ) ) ;
#56559 = CARTESIAN_POINT ( 'NONE',  ( -25.92875734969026524, -5.356774720514425603, 0.7300228001186309656 ) ) ;
#56560 = DIRECTION ( 'NONE',  ( 0.000000000000000000, -0.9967269304714136968, -0.08084198211964954695 ) ) ;
#56561 = ORIENTED_EDGE ( 'NONE', *, *, #1862, .F. ) ;
#56562 = DIRECTION ( 'NONE',  ( 0.000000000000000000, -0.9999999999976377785, -2.173523156925979128E-06 ) ) ;
#56563 = ORIENTED_EDGE ( 'NONE', *, *, #1901, .T. ) ;
#56564 = ORIENTED_EDGE ( 'NONE', *, *, #52896, .T. ) ;
#56565 = CARTESIAN_POINT ( 'NONE',  ( -90.52287095715006160, -29.50250243563736774, 8.947779886222139822 ) ) ;
#56566 = DIRECTION ( 'NONE',  ( -1.000000000000000000, -3.773278334444167608E-23, -8.201307833595939069E-29 ) ) ;
#56567 = CARTESIAN_POINT ( 'NONE',  ( -94.62287095715011276, -23.95044443724992789, 10.65354141964649592 ) ) ;
#56568 = CARTESIAN_POINT ( 'NONE',  ( 7.908618202329199320, -18.92053725880622039, -1.500000000000002220 ) ) ;
#56569 = EDGE_CURVE ( 'NONE', #6577, #27644, #70003, .T. ) ;
#56570 = ORIENTED_EDGE ( 'NONE', *, *, #25796, .T. ) ;
#56571 = CARTESIAN_POINT ( 'NONE',  ( 9.071512145086501278, -0.9000000000000000222, -3.687490859131162591 ) ) ;
#56572 = DIRECTION ( 'NONE',  ( -1.000000000000000000, 0.000000000000000000, 0.000000000000000000 ) ) ;
#56573 = DIRECTION ( 'NONE',  ( -3.773278334453079618E-23, 0.9999999999976377785, 2.173523156925979975E-06 ) ) ;
#56574 = CARTESIAN_POINT ( 'NONE',  ( -15.79502933763849271, 15.79022959414610661, -1.500000000000002220 ) ) ;
#56575 = CARTESIAN_POINT ( 'NONE',  ( -0.02085506613324774119, -22.78001478014103398, 7.291654623549858272 ) ) ;
#56576 = CARTESIAN_POINT ( 'NONE',  ( -90.58953762381671027, -24.99156044556120193, 7.747789690856343725 ) ) ;
#56577 = ADVANCED_FACE ( 'NONE', ( #73482 ), #72495, .F. ) ;
#56578 = ORIENTED_EDGE ( 'NONE', *, *, #66991, .T. ) ;
#56579 = CARTESIAN_POINT ( 'NONE',  ( -42.62287095715004881, -23.72747288104441665, -1.053458166803663110 ) ) ;
#56580 = PLANE ( 'NONE',  #15107 ) ;
#56581 = CARTESIAN_POINT ( 'NONE',  ( -0.6367455441941621830, -20.85161220577290919, -1.500000000000002220 ) ) ;
#56582 = B_SPLINE_CURVE_WITH_KNOTS ( 'NONE', 3,
 ( #29034, #5205, #13801, #44776, #90441, #59010 ),
 .UNSPECIFIED., .F., .F.,
 ( 4, 2, 4 ),
 ( 1.570887131794333942E-05, 0.001396322306279759555, 0.002776935741241575838 ),
 .UNSPECIFIED. ) ;
#56583 = ORIENTED_EDGE ( 'NONE', *, *, #38247, .F. ) ;
#56586 = VERTEX_POINT ( 'NONE', #33926 ) ;
#56585 = ADVANCED_FACE ( 'NONE', ( #50648 ), #73986, .T. ) ;
#56584 = DIRECTION ( 'NONE',  ( 0.000000000000000000, 0.000000000000000000, 1.000000000000000000 ) ) ;
#56587 = ORIENTED_EDGE ( 'NONE', *, *, #66535, .F. ) ;
#56588 = LINE ( 'NONE', #40838, #77826 ) ;
#56589 = CARTESIAN_POINT ( 'NONE',  ( -20.60145385712877797, -4.430719527714695793, -1.500000000000002220 ) ) ;
#56590 = ORIENTED_EDGE ( 'NONE', *, *, #39138, .F. ) ;
#56591 = CARTESIAN_POINT ( 'NONE',  ( -93.62287095715014118, -24.35013146730204525, 9.818937971375106599 ) ) ;
#56592 = CIRCLE ( 'NONE', #12803, 2.040000000000000036 ) ;
#56593 = CARTESIAN_POINT ( 'NONE',  ( -49.62788239718302918, -25.30563260921435997, 5.001563845361221894 ) ) ;
#56594 = PLANE ( 'NONE',  #83747 ) ;
#56595 = VECTOR ( 'NONE', #24065, 1000.000000000000000 ) ;
#56596 = CARTESIAN_POINT ( 'NONE',  ( -86.52215071448813433, -23.48786465467241058, 11.44779295918254647 ) ) ;
#56597 = PLANE ( 'NONE',  #96764 ) ;
#56598 = CARTESIAN_POINT ( 'NONE',  ( 16.98214085172422827, 13.50221961261776293, -1.500000000000002220 ) ) ;
#56599 = CARTESIAN_POINT ( 'NONE',  ( -64.52287095715009002, -23.72773821059535848, 11.05748984161097503 ) ) ;
#56601 = VERTEX_POINT ( 'NONE', #18684 ) ;
#56600 = CARTESIAN_POINT ( 'NONE',  ( 10.78255534502030777, 19.45608938089507234, 11.49999999999999645 ) ) ;
#56602 = CARTESIAN_POINT ( 'NONE',  ( -28.98875734969026396, 0.3587747205144265483, 10.11402280011862587 ) ) ;
#56603 = FACE_OUTER_BOUND ( 'NONE', #45225, .T. ) ;
#56604 = ORIENTED_EDGE ( 'NONE', *, *, #22669, .T. ) ;
#56605 = AXIS2_PLACEMENT_3D ( 'NONE', #26851, #42092, #27353 ) ;
#56606 = EDGE_CURVE ( 'NONE', #35091, #68548, #64906, .T. ) ;
#56608 = ORIENTED_EDGE ( 'NONE', *, *, #44426, .T. ) ;
#56607 = CARTESIAN_POINT ( 'NONE',  ( -5.960145391809922089, -6.376774720514415407, 20.04104409779160534 ) ) ;
#56609 = ORIENTED_EDGE ( 'NONE', *, *, #75870, .F. ) ;
#56610 = VECTOR ( 'NONE', #44177, 1000.000000000000114 ) ;
#56611 = CARTESIAN_POINT ( 'NONE',  ( 31.60906425211781823, -3.844812497472038793, -2.545713913898462799 ) ) ;
#56612 = EDGE_CURVE ( 'NONE', #5380, #48796, #12576, .T. ) ;
#56613 = CARTESIAN_POINT ( 'NONE',  ( -17.93149374516376682, -9.230432107326475233, 11.49999999999998934 ) ) ;
#56614 = CARTESIAN_POINT ( 'NONE',  ( -28.47875734969026240, 5.965225279485572685, 26.43402280011862615 ) ) ;
#56615 = ORIENTED_EDGE ( 'NONE', *, *, #19463, .F. ) ;
#56616 = VECTOR ( 'NONE', #54183, 1000.000000000000114 ) ;
#56617 = CARTESIAN_POINT ( 'NONE',  ( -130.5728709571500588, -25.16880041465311990, 7.429836627804590421 ) ) ;
#56618 = CARTESIAN_POINT ( 'NONE',  ( 15.34105849444754455, 16.31744944422920440, -1.500000000000002220 ) ) ;
#56619 = ORIENTED_EDGE ( 'NONE', *, *, #26447, .T. ) ;
#56620 = VERTEX_POINT ( 'NONE', #95815 ) ;
#56621 = DIRECTION ( 'NONE',  ( -1.000000000000000000, -0.000000000000000000, 0.000000000000000000 ) ) ;
#56622 = CARTESIAN_POINT ( 'NONE',  ( -101.5168322432302261, -23.96169478059713853, 10.65365249895717881 ) ) ;
#56623 = CARTESIAN_POINT ( 'NONE',  ( -39.99371170946986354, -25.31560150972321921, 5.007528838953862582 ) ) ;
#56624 = DIRECTION ( 'NONE',  ( -1.000000000000000000, 0.000000000000000000, 0.000000000000000000 ) ) ;
#56625 = CARTESIAN_POINT ( 'NONE',  ( -63.90635932737072267, -25.30557784678704181, 3.856996771331004048 ) ) ;
#56626 = CARTESIAN_POINT ( 'NONE',  ( -18.23851433863309879, 7.102826447048048664, -1.500000000000002220 ) ) ;
#56627 = FACE_OUTER_BOUND ( 'NONE', #52927, .T. ) ;
#56628 = ORIENTED_EDGE ( 'NONE', *, *, #93777, .T. ) ;
#56629 = CARTESIAN_POINT ( 'NONE',  ( -11.74548148041400708, 18.04809798412036059, -1.500000000000002220 ) ) ;
#56630 = DIRECTION ( 'NONE',  ( 0.000000000000000000, 1.000000000000000000, 0.000000000000000000 ) ) ;
#56631 = CARTESIAN_POINT ( 'NONE',  ( -71.23336565260535735, -25.25639482125388824, 6.552467071241729002 ) ) ;
#56632 = DIRECTION ( 'NONE',  ( -3.773278334453079618E-23, 0.9999999999976377785, 2.173523156925979975E-06 ) ) ;
#56633 = DIRECTION ( 'NONE',  ( 1.000000000000000000, 0.000000000000000000, 0.000000000000000000 ) ) ;
#56634 = CARTESIAN_POINT ( 'NONE',  ( -10.62949710387652758, 20.32685691788189075, -1.500000000000002220 ) ) ;
#56635 = APPLICATION_PROTOCOL_DEFINITION ( 'international standard', 'config_control_design', 1994, #97813 ) ;
#56636 = CARTESIAN_POINT ( 'NONE',  ( -92.55620429048339304, -23.47593901973091235, -1.443836447539002865 ) ) ;
#56637 = CARTESIAN_POINT ( 'NONE',  ( -2.457093156980370452, -5.876774720514412742, 19.51167604195716976 ) ) ;
#56638 = CARTESIAN_POINT ( 'NONE',  ( -20.09103079077430820, 1.113595961413322177, 11.49999999999999645 ) ) ;
#56639 = CARTESIAN_POINT ( 'NONE',  ( -110.1676456071266870, -25.10927397016051543, 2.835829822663707755 ) ) ;
#56640 = CARTESIAN_POINT ( 'NONE',  ( -31.52287095715006870, -24.34917612407033261, 0.1852690917477747279 ) ) ;
#56641 = CARTESIAN_POINT ( 'NONE',  ( -121.6228709571499706, -24.33927499327854704, 9.819080762295808285 ) ) ;
#56642 = CARTESIAN_POINT ( 'NONE',  ( -54.62287095715005592, -29.50250243563736774, 8.947779886222146928 ) ) ;
#56643 = B_SPLINE_CURVE_WITH_KNOTS ( 'NONE', 3,
 ( #66029, #41168, #98424, #66529 ),
 .UNSPECIFIED., .F., .F.,
 ( 4, 4 ),
 ( 0.000000000000000000, 9.999999999998897304E-05 ),
 .UNSPECIFIED. ) ;
#56644 = CARTESIAN_POINT ( 'NONE',  ( -126.5562042904833930, -24.64965694238575011, 8.947790433994191162 ) ) ;
#56645 = CARTESIAN_POINT ( 'NONE',  ( 13.50462702941046977, 14.53317887778067252, 11.49999999999998934 ) ) ;
#56646 = CARTESIAN_POINT ( 'NONE',  ( -4.700032041049139409, -6.144890974841530351, 8.999999999999998224 ) ) ;
#56647 = CARTESIAN_POINT ( 'NONE',  ( 16.91694316922610497, -9.995573847407506207, -1.500000000000002220 ) ) ;
#56648 = LINE ( 'NONE', #48535, #54055 ) ;
#56649 = CARTESIAN_POINT ( 'NONE',  ( -24.55517127435777525, 0.3587747205143967943, -15.44180958690143157 ) ) ;
#56650 = COORDINATED_UNIVERSAL_TIME_OFFSET ( 0, 0, .AHEAD. ) ;
#56651 = CARTESIAN_POINT ( 'NONE',  ( -60.52287095715005449, -24.51254535375846189, 9.355368624242151654 ) ) ;
#56652 = DIRECTION ( 'NONE',  ( -3.773278334453079030E-23, 0.9999999999976377785, 2.173523156925979128E-06 ) ) ;
#56653 = CARTESIAN_POINT ( 'NONE',  ( 4.765357849511589805, 20.07956653139741121, 11.49999999999999645 ) ) ;
#56654 = FACE_OUTER_BOUND ( 'NONE', #7110, .T. ) ;
#56655 = DIRECTION ( 'NONE',  ( 0.000000000000000000, 1.000000000000000000, 0.000000000000000000 ) ) ;
#56656 = CARTESIAN_POINT ( 'NONE',  ( -2.075279548881721947, -22.52154899835045043, 11.49999999999999645 ) ) ;
#56657 = ORIENTED_EDGE ( 'NONE', *, *, #91014, .F. ) ;
#56658 = CARTESIAN_POINT ( 'NONE',  ( -69.34303308397305443, -25.25639407517101276, 6.209207384461285173 ) ) ;
#56660 = EDGE_CURVE ( 'NONE', #64167, #100229, #79707, .T. ) ;
#56659 = CARTESIAN_POINT ( 'NONE',  ( 9.402885806365684829, 5.965225279485572685, 29.04108526060719342 ) ) ;
#56661 = CARTESIAN_POINT ( 'NONE',  ( -100.6814946224345846, -25.31401921878175898, 5.197788989978544549 ) ) ;
#56662 = CIRCLE ( 'NONE', #84221, 1.500000000000000666 ) ;
#56663 = ADVANCED_FACE ( 'NONE', ( #80592 ), #42053, .T. ) ;
#56664 = CARTESIAN_POINT ( 'NONE',  ( 282.9764569301858046, -6.376774720514426953, 20.79159422840526616 ) ) ;
#56665 = EDGE_CURVE ( 'NONE', #65090, #61812, #84555, .T. ) ;
#56666 = CARTESIAN_POINT ( 'NONE',  ( -2.794793911895765870, -6.376774720514417183, 20.33046051580616265 ) ) ;
#56667 = AXIS2_PLACEMENT_3D ( 'NONE', #60453, #27988, #91373 ) ;
#56668 = EDGE_CURVE ( 'NONE', #48696, #39695, #36232, .T. ) ;
#56669 = VERTEX_POINT ( 'NONE', #27308 ) ;
#56670 = CARTESIAN_POINT ( 'NONE',  ( -80.43221577628075636, -25.31596222142643171, 4.967019754985606106 ) ) ;
#56671 = CARTESIAN_POINT ( 'NONE',  ( -0.7673284989158746239, 22.82873350090251918, 11.49999999999998934 ) ) ;
#56672 = CARTESIAN_POINT ( 'NONE',  ( -91.62287095715004170, -29.50247984919015209, -1.443849546365051806 ) ) ;
#56673 = CIRCLE ( 'NONE', #67968, 25.90800000000000125 ) ;
#56674 = LINE ( 'NONE', #18091, #31751 ) ;
#56675 = DIRECTION ( 'NONE',  ( 0.000000000000000000, 1.000000000000000000, 0.000000000000000000 ) ) ;
#56676 = CARTESIAN_POINT ( 'NONE',  ( -6.716530693746936898, -21.44081863256500142, 11.49999999999999645 ) ) ;
#56677 = ORIENTED_EDGE ( 'NONE', *, *, #62081, .T. ) ;
#56678 = AXIS2_PLACEMENT_3D ( 'NONE', #52788, #60908, #490 ) ;
#56679 = DIRECTION ( 'NONE',  ( 0.000000000000000000, 1.000000000000000000, 0.000000000000000000 ) ) ;
#56680 = B_SPLINE_CURVE_WITH_KNOTS ( 'NONE', 3,
 ( #37552, #99437, #12204, #84213, #81340, #23818 ),
 .UNSPECIFIED., .F., .F.,
 ( 4, 2, 4 ),
 ( 0.000000000000000000, 0.001380764517853246432, 0.002761529035706492864 ),
 .UNSPECIFIED. ) ;
#56681 = CARTESIAN_POINT ( 'NONE',  ( 1.410849576418898632, -21.91845101833037290, -1.500000000000002220 ) ) ;
#56682 = LINE ( 'NONE', #94716, #93239 ) ;
#56684 = CARTESIAN_POINT ( 'NONE',  ( -34.65814782573328046, -23.73791477778911485, 11.05961554403171299 ) ) ;
#56683 = VECTOR ( 'NONE', #49874, 1000.000000000000114 ) ;
#56685 = CARTESIAN_POINT ( 'NONE',  ( -112.5228709571500616, -24.64965694238408034, 8.947790433994192938 ) ) ;
#56686 = EDGE_LOOP ( 'NONE', ( #19883, #14727, #50536, #71806 ) ) ;
#56687 = EDGE_CURVE ( 'NONE', #43471, #14228, #65909, .T. ) ;
#56688 = CARTESIAN_POINT ( 'NONE',  ( -112.5562042904834072, -23.48786465467241769, 11.44779295918253581 ) ) ;
#56689 = DIRECTION ( 'NONE',  ( -3.773278334453079030E-23, 0.9999999999976377785, 2.173523156925979128E-06 ) ) ;
#56690 = ORIENTED_EDGE ( 'NONE', *, *, #97429, .T. ) ;
#56691 = CARTESIAN_POINT ( 'NONE',  ( -105.6228709571500559, -23.48783264082479150, -1.443836473390060160 ) ) ;
#56692 = CARTESIAN_POINT ( 'NONE',  ( 19.83930831332124001, -5.160774681608516268, -1.500000000000002220 ) ) ;
#56693 = ORIENTED_EDGE ( 'NONE', *, *, #70392, .T. ) ;
#56694 = VERTEX_POINT ( 'NONE', #26810 ) ;
#56695 = VERTEX_POINT ( 'NONE', #19679 ) ;
#56696 = ORIENTED_EDGE ( 'NONE', *, *, #18083, .F. ) ;
#56697 = CARTESIAN_POINT ( 'NONE',  ( -28.32169924589829080, 5.965225279485592225, -8.244178532169447848 ) ) ;
#56698 = CARTESIAN_POINT ( 'NONE',  ( 21.06059016766346659, 9.494407541345388779, 11.49999999999998934 ) ) ;
#56699 = CARTESIAN_POINT ( 'NONE',  ( -104.5858001345268349, -24.66019654487200441, 8.947790411086108620 ) ) ;
#56700 = CARTESIAN_POINT ( 'NONE',  ( 8.409737122318338365, 18.51778827956368190, -1.500000000000002220 ) ) ;
#56701 = ORIENTED_EDGE ( 'NONE', *, *, #38202, .T. ) ;
#56702 = DIRECTION ( 'NONE',  ( 0.000000000000000000, 0.000000000000000000, 1.000000000000000000 ) ) ;
#56703 = CARTESIAN_POINT ( 'NONE',  ( -50.54485904939332386, -25.12158324412746424, 2.838362104969525124 ) ) ;
#56704 = CARTESIAN_POINT ( 'NONE',  ( -101.5468792378191836, -25.25287247409163527, 6.236250661346386615 ) ) ;
#56705 = CARTESIAN_POINT ( 'NONE',  ( 4.214857194124448370, -6.376774720514402972, 18.65898740197609840 ) ) ;
#56706 = ORIENTED_EDGE ( 'NONE', *, *, #40806, .T. ) ;
#56707 = CARTESIAN_POINT ( 'NONE',  ( -29.24636659181000198, -25.21532237603348037, 4.940287017762114985 ) ) ;
#56708 = CARTESIAN_POINT ( 'NONE',  ( -49.14050969713319716, -25.31573689518325310, 4.284284265464324726 ) ) ;
#56709 = ORIENTED_EDGE ( 'NONE', *, *, #98216, .T. ) ;
#56710 = CARTESIAN_POINT ( 'NONE',  ( -18.78340662496949776, 8.880393494302802893, 11.49999999999998934 ) ) ;
#56711 = VERTEX_POINT ( 'NONE', #14062 ) ;
#56713 = ORIENTED_EDGE ( 'NONE', *, *, #90659, .T. ) ;
#56712 = CARTESIAN_POINT ( 'NONE',  ( -125.5194286696376338, -24.92564183028979485, 1.928384488918254425 ) ) ;
#56714 = LINE ( 'NONE', #40974, #1731 ) ;
#56715 = CARTESIAN_POINT ( 'NONE',  ( 2.100208336950355914, 0.000000000000000000, 1.249999999999996003 ) ) ;
#56716 = ORIENTED_EDGE ( 'NONE', *, *, #2074, .F. ) ;
#56717 = ORIENTED_EDGE ( 'NONE', *, *, #66528, .T. ) ;
#56718 = DIRECTION ( 'NONE',  ( 0.000000000000000000, 0.000000000000000000, 1.000000000000000000 ) ) ;
#56719 = CARTESIAN_POINT ( 'NONE',  ( -98.55620429048339304, -23.48786465467241769, 11.44779295918253759 ) ) ;
#56720 = CARTESIAN_POINT ( 'NONE',  ( -78.52287095715006160, -23.72747288104470087, -1.053458166803226126 ) ) ;
#56722 = ORIENTED_EDGE ( 'NONE', *, *, #96979, .T. ) ;
#56721 = CARTESIAN_POINT ( 'NONE',  ( -0.5447568859041533873, -22.05808898580190558, 11.49999999999999645 ) ) ;
#56723 = CARTESIAN_POINT ( 'NONE',  ( -108.6335339856925799, -23.48783264082478794, -1.443836473390062825 ) ) ;
#56724 = CARTESIAN_POINT ( 'NONE',  ( 15.88279217892459094, 16.07415641707351384, 11.49999999999998934 ) ) ;
#56725 = B_SPLINE_CURVE_WITH_KNOTS ( 'NONE', 3,
 ( #12307, #96555, #10828, #88956, #95562, #49407 ),
 .UNSPECIFIED., .F., .F.,
 ( 4, 2, 4 ),
 ( 0.000000000000000000, 0.001380764517854764749, 0.002761529035709529498 ),
 .UNSPECIFIED. ) ;
#56726 = ADVANCED_FACE ( 'NONE', ( #76457 ), #45536, .F. ) ;
#56728 = VERTEX_POINT ( 'NONE', #29298 ) ;
#56727 = DIRECTION ( 'NONE',  ( -1.000000000000000000, -0.000000000000000000, -0.000000000000000000 ) ) ;
#56729 = VERTEX_POINT ( 'NONE', #22170 ) ;
#56730 = DIRECTION ( 'NONE',  ( 1.000000000000000000, 3.773278334444167608E-23, 8.201307833595939069E-29 ) ) ;
#56732 = EDGE_CURVE ( 'NONE', #61820, #37466, #8364, .T. ) ;
#56731 = AXIS2_PLACEMENT_3D ( 'NONE', #32390, #56250, #16157 ) ;
#56733 = CARTESIAN_POINT ( 'NONE',  ( -94.62287095715005592, -24.64898659630528854, 1.056161002820827921 ) ) ;
#56734 = VERTEX_POINT ( 'NONE', #67875 ) ;
#56735 = CARTESIAN_POINT ( 'NONE',  ( -4.955175619359221351, 20.59750927568439138, -1.500000000000002220 ) ) ;
#56736 = CARTESIAN_POINT ( 'NONE',  ( -66.62287095715005592, -23.72773821059535493, 11.05748984161097681 ) ) ;
#56737 = DIRECTION ( 'NONE',  ( 0.000000000000000000, 0.000000000000000000, 1.000000000000000000 ) ) ;
#56738 = VECTOR ( 'NONE', #31072, 1000.000000000000000 ) ;
#56739 = CARTESIAN_POINT ( 'NONE',  ( -7.234140626586239797, -5.876774720514411854, 19.72789237585158162 ) ) ;
#56740 = CARTESIAN_POINT ( 'NONE',  ( -41.73352883455704898, -25.30440811136059764, 4.814461953015128692 ) ) ;
#56741 = CARTESIAN_POINT ( 'NONE',  ( -7.359855604737914447, 20.98419016808480109, -1.500000000000002220 ) ) ;
#56742 = B_SPLINE_CURVE_WITH_KNOTS ( 'NONE', 3,
 ( #59831, #21241, #91261, #91752 ),
 .UNSPECIFIED., .F., .F.,
 ( 4, 4 ),
 ( 0.000000000000000000, 9.999999999998897304E-05 ),
 .UNSPECIFIED. ) ;
#56743 = CARTESIAN_POINT ( 'NONE',  ( -114.5511112493029344, -24.65952944569305316, 1.056160979905706121 ) ) ;
#56744 = ORIENTED_EDGE ( 'NONE', *, *, #38707, .F. ) ;
#56745 = DIRECTION ( 'NONE',  ( -3.773278334453079030E-23, 0.9999999999976377785, 2.173523156925978705E-06 ) ) ;
#56746 = CARTESIAN_POINT ( 'NONE',  ( -7.326923076923074873, -5.876774720514426953, 21.75000000000001066 ) ) ;
#56747 = CARTESIAN_POINT ( 'NONE',  ( -7.246369895950522277, -17.95243785538732340, 11.49999999999999645 ) ) ;
#56748 = VECTOR ( 'NONE', #18394, 1000.000000000000000 ) ;
#56749 = CARTESIAN_POINT ( 'NONE',  ( -71.55620429048339304, -23.48783264082478084, -1.443836473390067265 ) ) ;
#56750 = CARTESIAN_POINT ( 'NONE',  ( -116.6228709571500559, -24.64898659630368627, 1.056161002820833028 ) ) ;
#56751 = AXIS2_PLACEMENT_3D ( 'NONE', #30960, #85244, #40591 ) ;
#56752 = CARTESIAN_POINT ( 'NONE',  ( 19.40022266231057202, 1.907866353064612053, -1.500000000000002220 ) ) ;
#56753 = VECTOR ( 'NONE', #82359, 1000.000000000000114 ) ;
#56754 = CARTESIAN_POINT ( 'NONE',  ( 1.185105815240312888, -21.37944065014308848, -1.500000000000002220 ) ) ;
#56755 = CARTESIAN_POINT ( 'NONE',  ( -32.52287095715006160, -24.64965694238575011, 8.947790433994207149 ) ) ;
#56756 = CARTESIAN_POINT ( 'NONE',  ( -60.51213338828525679, -23.85049219812968957, 10.88485053497088728 ) ) ;
#56757 = CARTESIAN_POINT ( 'NONE',  ( -51.49552821830581451, -24.34968618360933590, 0.1864209137778788938 ) ) ;
#56758 = CARTESIAN_POINT ( 'NONE',  ( -120.6228709571500417, -24.99156045073393528, 7.747789690856161648 ) ) ;
#56759 = CARTESIAN_POINT ( 'NONE',  ( 7.533951754900199305, 21.46025436219600024, -1.500000000000002220 ) ) ;
#56760 = VECTOR ( 'NONE', #22993, 1000.000000000000000 ) ;
#56761 = CARTESIAN_POINT ( 'NONE',  ( -98.54623345124143441, -24.65952944569305316, 1.056160979905702124 ) ) ;
#56762 = CARTESIAN_POINT ( 'NONE',  ( -80.52287095715003318, -23.84047902841601996, -0.8780736468305722076 ) ) ;
#56763 = CARTESIAN_POINT ( 'NONE',  ( 11.60740158406642664, -16.16820694497113564, 11.49999999999999645 ) ) ;
#56764 = DIRECTION ( 'NONE',  ( 0.000000000000000000, 0.9999999999976377785, 2.173523156925979128E-06 ) ) ;
#56765 = B_SPLINE_CURVE_WITH_KNOTS ( 'NONE', 3,
 ( #32822, #9480, #92211, #366, #85100, #8484 ),
 .UNSPECIFIED., .F., .F.,
 ( 4, 2, 4 ),
 ( 0.000000000000000000, 0.001380901958385381606, 0.002761803916770763211 ),
 .UNSPECIFIED. ) ;
#56766 = CARTESIAN_POINT ( 'NONE',  ( -39.52823043622210974, -24.66019654487198665, 8.947790411086131712 ) ) ;
#56767 = CARTESIAN_POINT ( 'NONE',  ( -112.5228709571500616, -29.50247984919015209, -1.443849546365048253 ) ) ;
#56768 = ORIENTED_EDGE ( 'NONE', *, *, #94198, .F. ) ;
#56769 = CARTESIAN_POINT ( 'NONE',  ( -93.62287095715005592, -29.50247984919015209, -1.443849546365051806 ) ) ;
#56770 = DIRECTION ( 'NONE',  ( 0.000000000000000000, -1.000000000000000000, 0.000000000000000000 ) ) ;
#56771 = CARTESIAN_POINT ( 'NONE',  ( -12.04083774165243881, -18.01462592983040523, -1.500000000000002220 ) ) ;
#56772 = FACE_OUTER_BOUND ( 'NONE', #67340, .T. ) ;
#56773 = CARTESIAN_POINT ( 'NONE',  ( 8.422564666779264186, -17.53554878399664574, -1.500000000000002220 ) ) ;
#56774 = CARTESIAN_POINT ( 'NONE',  ( -93.52287095715011844, -23.96127896941631974, -0.6493128931038023577 ) ) ;
#56775 = ORIENTED_EDGE ( 'NONE', *, *, #12075, .T. ) ;
#56776 = CYLINDRICAL_SURFACE ( 'NONE', #2998, 2.040000000000000036 ) ;
#56777 = CARTESIAN_POINT ( 'NONE',  ( -20.32544160278596834, -1.370942541838689799, 11.49999999999999645 ) ) ;
#56778 = FACE_OUTER_BOUND ( 'NONE', #23436, .T. ) ;
#56779 = B_SPLINE_CURVE_WITH_KNOTS ( 'NONE', 3,
 ( #57598, #96633, #49989, #26130, #4299, #11901 ),
 .UNSPECIFIED., .F., .F.,
 ( 4, 2, 4 ),
 ( 1.570887131794333942E-05, 0.001396322306279758037, 0.002776935741241572803 ),
 .UNSPECIFIED. ) ;
#56780 = CARTESIAN_POINT ( 'NONE',  ( -86.55620429048339304, -24.64965694238575011, 8.947790433994194714 ) ) ;
#56781 = ORIENTED_EDGE ( 'NONE', *, *, #69201, .T. ) ;
#56782 = CARTESIAN_POINT ( 'NONE',  ( -72.52287095715010423, -23.48783264082476308, -1.443836473390092578 ) ) ;
#56783 = PLANE ( 'NONE',  #29867 ) ;
#56784 = CARTESIAN_POINT ( 'NONE',  ( -39.04303308397306438, -25.31628448545684407, 4.215216869667997024 ) ) ;
#56785 = EDGE_CURVE ( 'NONE', #82541, #59433, #31370, .T. ) ;
#56786 = CARTESIAN_POINT ( 'NONE',  ( -49.45828852499023753, -25.25138767200333589, 5.632645021930186680 ) ) ;
#56787 = CARTESIAN_POINT ( 'NONE',  ( -129.5228709571499905, -23.48783264082477729, -1.443836473390079700 ) ) ;
#56788 = CARTESIAN_POINT ( 'NONE',  ( -109.5167418412546709, -24.15543982623907482, -0.2315651400026587370 ) ) ;
#56790 = ORIENTED_EDGE ( 'NONE', *, *, #20668, .T. ) ;
#56789 = EDGE_CURVE ( 'NONE', #76914, #71823, #61269, .T. ) ;
#56791 = CARTESIAN_POINT ( 'NONE',  ( -66.64101351466018741, -23.96169478059713143, 10.65365249895718058 ) ) ;
#56792 = EDGE_CURVE ( 'NONE', #50913, #70837, #47006, .T. ) ;
#56793 = CARTESIAN_POINT ( 'NONE',  ( 22.85142058292489153, -2.183311388647848350, 11.49999999999999645 ) ) ;
#56794 = CARTESIAN_POINT ( 'NONE',  ( 22.69831151501224298, -1.600861625767590724, -1.500000000000002220 ) ) ;
#56795 = CARTESIAN_POINT ( 'NONE',  ( 4.819673832743241348, -6.376774720514422512, 21.07066438048017076 ) ) ;
#56796 = EDGE_CURVE ( 'NONE', #26222, #46090, #60764, .T. ) ;
#56797 = LINE ( 'NONE', #18213, #25302 ) ;
#56798 = CARTESIAN_POINT ( 'NONE',  ( -90.58310404013386119, -24.92564183028979130, 1.928384488918253536 ) ) ;
#56799 = ADVANCED_FACE ( 'NONE', ( #84078 ), #28801, .F. ) ;
#56800 = CARTESIAN_POINT ( 'NONE',  ( -69.37501441204418029, -25.22917552048557965, 6.451241004143004609 ) ) ;
#56801 = AXIS2_PLACEMENT_3D ( 'NONE', #71277, #32704, #94605 ) ;
#56802 = CARTESIAN_POINT ( 'NONE',  ( -1.606994170628035068, 21.82944698466814870, -1.500000000000002220 ) ) ;
#56803 = CARTESIAN_POINT ( 'NONE',  ( 6.660000000000001030, 0.000000000000000000, 0.000000000000000000 ) ) ;
#56804 = CARTESIAN_POINT ( 'NONE',  ( -26.76057841451696362, -24.78115552336511129, 2.652511023330785367 ) ) ;
#56805 = DIRECTION ( 'NONE',  ( 1.000000000000000000, -0.000000000000000000, 2.417950247244706201E-16 ) ) ;
#56806 = CARTESIAN_POINT ( 'NONE',  ( -58.55359724368977936, -23.96119346886881019, -0.6495511937832116889 ) ) ;
#56807 = ORIENTED_EDGE ( 'NONE', *, *, #43975, .F. ) ;
#56808 = CARTESIAN_POINT ( 'NONE',  ( -14.48729221511043441, 14.40292172154154926, 11.49999999999998934 ) ) ;
#56809 = VERTEX_POINT ( 'NONE', #68370 ) ;
#56810 = VERTEX_POINT ( 'NONE', #82589 ) ;
#56811 = EDGE_CURVE ( 'NONE', #63805, #20892, #4967, .T. ) ;
#56812 = CARTESIAN_POINT ( 'NONE',  ( 3.792298468851710069, -22.70151372599487871, 11.49999999999998934 ) ) ;
#56813 = CARTESIAN_POINT ( 'NONE',  ( -30.64427850938831099, -23.56000036390796382, 11.50200000000000067 ) ) ;
#56814 = ORIENTED_EDGE ( 'NONE', *, *, #78039, .F. ) ;
#56815 = CARTESIAN_POINT ( 'NONE',  ( -108.5593205469241553, -23.48786465467241413, 11.44779295918253759 ) ) ;
#56816 = DIRECTION ( 'NONE',  ( -3.773278334444167608E-23, 1.000000000000000000, 0.000000000000000000 ) ) ;
#56818 = CARTESIAN_POINT ( 'NONE',  ( -62.52287095715006160, -29.50247984919015209, -1.443849546365056913 ) ) ;
#56817 = AXIS2_PLACEMENT_3D ( 'NONE', #96752, #27251, #89147 ) ;
#56819 = CARTESIAN_POINT ( 'NONE',  ( -118.8950128664978507, -25.24724904090927424, 6.200150947452693018 ) ) ;
#56821 = ORIENTED_EDGE ( 'NONE', *, *, #64512, .T. ) ;
#56820 = CARTESIAN_POINT ( 'NONE',  ( -21.27170209485220198, -2.091907790468015005, 11.49999999999999645 ) ) ;
#56822 = AXIS2_PLACEMENT_3D ( 'NONE', #11973, #42941, #73875 ) ;
#56823 = ORIENTED_EDGE ( 'NONE', *, *, #8646, .F. ) ;
#56824 = CARTESIAN_POINT ( 'NONE',  ( -7.359855604737914447, 20.98419016808480109, -1.500000000000002220 ) ) ;
#56825 = CARTESIAN_POINT ( 'NONE',  ( 3.345817365282868217, 20.41450801592841557, -1.500000000000002220 ) ) ;
#56826 = AXIS2_PLACEMENT_3D ( 'NONE', #46744, #52357, #46236 ) ;
#56827 = EDGE_LOOP ( 'NONE', ( #958, #42752, #39466, #20346 ) ) ;
#56828 = CARTESIAN_POINT ( 'NONE',  ( -5.970505764849975527, -6.376774720514411854, 19.55848054040323802 ) ) ;
#56829 = CARTESIAN_POINT ( 'NONE',  ( 2.932009311892267434, -5.876774720514410077, 19.53174284846577891 ) ) ;
#56830 = ORIENTED_EDGE ( 'NONE', *, *, #96630, .T. ) ;
#56831 = DIRECTION ( 'NONE',  ( -9.524068072025174096E-40, -2.173523156925980399E-06, 0.9999999999976378895 ) ) ;
#56832 = ORIENTED_EDGE ( 'NONE', *, *, #27260, .T. ) ;
#56833 = CARTESIAN_POINT ( 'NONE',  ( 12.99736557111424595, -3.316774720514426900, -27.13536621820933448 ) ) ;
#56834 = CARTESIAN_POINT ( 'NONE',  ( -71.17423078786923440, -25.19025574039271831, 6.676846143341355067 ) ) ;
#56835 = CARTESIAN_POINT ( 'NONE',  ( -11.21968731015968856, -17.59241007644406096, -1.500000000000002220 ) ) ;
#56837 = EDGE_CURVE ( 'NONE', #35259, #55090, #92992, .T. ) ;
#56836 = CARTESIAN_POINT ( 'NONE',  ( 21.45948982579844255, -4.128456637845983934, 11.49999999999999645 ) ) ;
#56838 = LINE ( 'NONE', #72057, #65832 ) ;
#56839 = CARTESIAN_POINT ( 'NONE',  ( -37.62287095715007013, -24.51283580621364777, 0.6167428607019709297 ) ) ;
#56840 = CARTESIAN_POINT ( 'NONE',  ( 0.003324065884441271702, 22.49086686382009503, -1.500000000000002220 ) ) ;
#56841 = CARTESIAN_POINT ( 'NONE',  ( -8.531171415479239073, -19.09552649099111221, 11.49999999999998934 ) ) ;
#56842 = CARTESIAN_POINT ( 'NONE',  ( -26.15327376889522526, -24.88148900154536491, 5.797586012370106623 ) ) ;
#56843 = EDGE_CURVE ( 'NONE', #63848, #93973, #75960, .T. ) ;
#56844 = CARTESIAN_POINT ( 'NONE',  ( 30.53060340732035982, 0.6647747205144264315, 20.86760796525322093 ) ) ;
#56845 = LINE ( 'NONE', #74049, #50761 ) ;
#56846 = EDGE_LOOP ( 'NONE', ( #38750, #85992, #3525, #15108 ) ) ;
#56847 = VERTEX_POINT ( 'NONE', #99304 ) ;
#56848 = EDGE_LOOP ( 'NONE', ( #81861, #59417, #83124, #61664 ) ) ;
#56849 = CARTESIAN_POINT ( 'NONE',  ( -5.366453405989236813, 0.000000000000000000, 0.000000000000000000 ) ) ;
#56850 = VERTEX_POINT ( 'NONE', #13065 ) ;
#56851 = CARTESIAN_POINT ( 'NONE',  ( -17.32345979880200204, -12.59856583755568415, -1.500000000000002220 ) ) ;
#56853 = EDGE_CURVE ( 'NONE', #55337, #21700, #10707, .T. ) ;
#56852 = CARTESIAN_POINT ( 'NONE',  ( -15.72835732567950195, 15.92727474065614501, 11.49999999999999645 ) ) ;
#56854 = EDGE_LOOP ( 'NONE', ( #32821, #51713, #98427, #37946, #6383, #4969, #15912, #90748 ) ) ;
#56855 = CARTESIAN_POINT ( 'NONE',  ( -26.12985137885329223, -24.94751919380807692, 5.610999066408565383 ) ) ;
#56856 = CARTESIAN_POINT ( 'NONE',  ( -4.359323203648655998, -20.60729432550360585, -1.500000000000002220 ) ) ;
#56857 = CARTESIAN_POINT ( 'NONE',  ( -30.47189344453343551, -23.47433389951690330, 11.44779287168131710 ) ) ;
#56858 = CARTESIAN_POINT ( 'NONE',  ( 19.82558669001425500, -2.195561414069463702, -1.500000000000002220 ) ) ;
#56859 = CARTESIAN_POINT ( 'NONE',  ( -50.58895421723637043, -24.52399227489127043, 9.353111116836521077 ) ) ;
#56860 = CARTESIAN_POINT ( 'NONE',  ( -88.62287095715004170, -29.50250243563736774, 8.947779886222139822 ) ) ;
#56861 = CARTESIAN_POINT ( 'NONE',  ( -21.70078857174656761, -3.768841730229552045, -1.500000000000002220 ) ) ;
#56862 = VERTEX_POINT ( 'NONE', #83578 ) ;
#56863 = CARTESIAN_POINT ( 'NONE',  ( -65.63574626809028700, -24.52399227489126687, 9.353111116836526406 ) ) ;
#56864 = ADVANCED_FACE ( 'NONE', ( #46037 ), #29798, .F. ) ;
#56865 = CARTESIAN_POINT ( 'NONE',  ( -93.62287095715005592, -29.50248528299804818, 1.056150453629040253 ) ) ;
#56866 = CARTESIAN_POINT ( 'NONE',  ( -41.25901049487872996, -25.27956024727518525, 5.328837458236013624 ) ) ;
#56867 = CARTESIAN_POINT ( 'NONE',  ( -29.83719645772528750, -25.26444761590789767, 6.075536601959948158 ) ) ;
#56868 = CARTESIAN_POINT ( 'NONE',  ( -25.55992647825761566, -24.89300974704809022, 4.202247098034709971 ) ) ;
#56869 = DIRECTION ( 'NONE',  ( 1.334402673828313339E-16, -0.000000000000000000, -1.000000000000000000 ) ) ;
#56870 = CARTESIAN_POINT ( 'NONE',  ( -6.620899627221215944, -20.26055204357936290, -1.500000000000002220 ) ) ;
#56871 = CARTESIAN_POINT ( 'NONE',  ( -104.5228709571501327, -24.51387760970725438, 9.387446482453409402 ) ) ;
#56872 = CARTESIAN_POINT ( 'NONE',  ( 30.53060340732036337, 5.329285123471892760, 3.289350009555732868 ) ) ;
#56873 = B_SPLINE_CURVE_WITH_KNOTS ( 'NONE', 3,
 ( #54900, #92439, #16323, #92938 ),
 .UNSPECIFIED., .F., .F.,
 ( 4, 4 ),
 ( 0.000000000000000000, 0.0004038461538461574074 ),
 .UNSPECIFIED. ) ;
#56874 = CIRCLE ( 'NONE', #92456, 2.249999999999998668 ) ;
#56875 = DIRECTION ( 'NONE',  ( -0.000000000000000000, 1.000000000000000000, -0.000000000000000000 ) ) ;
#56876 = DIRECTION ( 'NONE',  ( 3.773278334444167608E-23, -1.000000000000000000, 0.000000000000000000 ) ) ;
#56877 = APPROVAL ( #58505, 'UNSPECIFIED' ) ;
#56878 = CARTESIAN_POINT ( 'NONE',  ( 20.74359285767136640, 8.971229656761206428, -1.500000000000002220 ) ) ;
#56879 = CARTESIAN_POINT ( 'NONE',  ( -123.6228709571500559, -24.64898659630368627, 1.056161002820833028 ) ) ;
#56880 = ORIENTED_EDGE ( 'NONE', *, *, #99262, .F. ) ;
#56881 = CARTESIAN_POINT ( 'NONE',  ( 4.415069475862049231, -5.876774720514424288, 21.13806644168711557 ) ) ;
#56882 = CARTESIAN_POINT ( 'NONE',  ( -122.6228709571500417, -24.33832256526969218, 0.1851278514119942820 ) ) ;
#56883 = CARTESIAN_POINT ( 'NONE',  ( 3.553741186906278493, -19.43417129498564577, 11.49999999999999645 ) ) ;
#56884 = DIRECTION ( 'NONE',  ( 0.000000000000000000, 0.000000000000000000, 1.000000000000000000 ) ) ;
#56885 = CARTESIAN_POINT ( 'NONE',  ( -73.52287095715013265, -24.33927499327855770, 9.819080762295815390 ) ) ;
#56886 = VERTEX_POINT ( 'NONE', #37914 ) ;
#56887 = DIRECTION ( 'NONE',  ( 0.000000000000000000, -1.000000000000000000, 0.000000000000000000 ) ) ;
#56888 = CARTESIAN_POINT ( 'NONE',  ( -124.4728709594060376, -25.21147767388034566, 8.000950762517446080 ) ) ;
#56889 = CARTESIAN_POINT ( 'NONE',  ( -105.5228709571500758, -24.52323809116984421, 9.355190652339418378 ) ) ;
#56890 = CARTESIAN_POINT ( 'NONE',  ( -9.149999999999996803, -6.376774720514426953, 11.88602120139452012 ) ) ;
#56891 = CARTESIAN_POINT ( 'NONE',  ( -95.52287095715003318, -23.85229601348997264, 10.88205029486208630 ) ) ;
#56892 = CARTESIAN_POINT ( 'NONE',  ( -113.5228709571500616, -24.65952944569304961, 1.056160979905704123 ) ) ;
#56893 = CARTESIAN_POINT ( 'NONE',  ( -18.42202159362721048, -7.168033771007030097, 11.49999999999998934 ) ) ;
#56894 = B_SPLINE_CURVE_WITH_KNOTS ( 'NONE', 3,
 ( #63239, #85050, #31266, #46500 ),
 .UNSPECIFIED., .F., .F.,
 ( 4, 4 ),
 ( 0.000000000000000000, 9.999999999998897304E-05 ),
 .UNSPECIFIED. ) ;
#56895 = VECTOR ( 'NONE', #69198, 1000.000000000000114 ) ;
#56896 = EDGE_LOOP ( 'NONE', ( #53097, #8514, #55097, #20963 ) ) ;
#56897 = AXIS2_PLACEMENT_3D ( 'NONE', #57068, #25597, #89001 ) ;
#56898 = CARTESIAN_POINT ( 'NONE',  ( 8.473373031455752269, -18.34320851062214430, 11.49999999999999645 ) ) ;
#56899 = CARTESIAN_POINT ( 'NONE',  ( 13.25751441563444999, 6.376774720514426065, -25.10777837594209672 ) ) ;
#56900 = ORIENTED_EDGE ( 'NONE', *, *, #11170, .T. ) ;
#56901 = DIRECTION ( 'NONE',  ( 0.09824042138329625029, 2.980407940728111021E-17, -0.9951627101165079203 ) ) ;
#56902 = CARTESIAN_POINT ( 'NONE',  ( -118.6228709571500559, -24.64898659630368627, 1.056161002820833028 ) ) ;
#56903 = DIRECTION ( 'NONE',  ( 0.000000000000000000, 0.000000000000000000, 1.000000000000000000 ) ) ;
#56904 = CARTESIAN_POINT ( 'NONE',  ( -97.62287095715005592, -29.50247984919015209, -1.443849546365050029 ) ) ;
#56905 = CARTESIAN_POINT ( 'NONE',  ( -128.6228709571500417, -23.47593901973091235, -1.443836447538995760 ) ) ;
#56906 = CARTESIAN_POINT ( 'NONE',  ( -96.52287095715001897, -24.34917612406836795, 0.1852690917426570161 ) ) ;
#56908 = EDGE_CURVE ( 'NONE', #15238, #90130, #28651, .T. ) ;
#56907 = CARTESIAN_POINT ( 'NONE',  ( 12.85705330080557829, 15.37097598829428513, -1.500000000000002220 ) ) ;
#56909 = CARTESIAN_POINT ( 'NONE',  ( -39.62287095715005592, -23.47596703998600276, 11.44779298504227505 ) ) ;
#56910 = ORIENTED_EDGE ( 'NONE', *, *, #46466, .T. ) ;
#56911 = FACE_OUTER_BOUND ( 'NONE', #25988, .T. ) ;
#56912 = EDGE_CURVE ( 'NONE', #77838, #7215, #84578, .T. ) ;
#56913 = CARTESIAN_POINT ( 'NONE',  ( -35.51858042511292979, -25.00158670708910336, 2.256160236439224143 ) ) ;
#56914 = CARTESIAN_POINT ( 'NONE',  ( -92.62287095715009855, -23.95044443724992789, 10.65354141964649948 ) ) ;
#56915 = EDGE_CURVE ( 'NONE', #17738, #97857, #59260, .T. ) ;
#56916 = CARTESIAN_POINT ( 'NONE',  ( -113.5228709571500616, -23.47593901973090524, -1.443836447538996204 ) ) ;
#56917 = CARTESIAN_POINT ( 'NONE',  ( -73.54184938391159676, -24.51314013834315375, 0.6176544820404108460 ) ) ;
#56918 = CARTESIAN_POINT ( 'NONE',  ( -89.40841769935767047, -25.22391154813773895, 6.409327647370974823 ) ) ;
#56919 = CARTESIAN_POINT ( 'NONE',  ( -49.56706780694642589, -25.23900318944143706, 3.731069057777267162 ) ) ;
#56920 = ORIENTED_EDGE ( 'NONE', *, *, #65023, .T. ) ;
#56921 = CARTESIAN_POINT ( 'NONE',  ( -20.26613141553852060, -1.498020344548873561, 11.49999999999998934 ) ) ;
#56922 = ORIENTED_EDGE ( 'NONE', *, *, #14594, .T. ) ;
#56923 = B_SPLINE_CURVE_WITH_KNOTS ( 'NONE', 3,
 ( #39087, #62951, #55837, #47719 ),
 .UNSPECIFIED., .F., .F.,
 ( 4, 4 ),
 ( 0.000000000000000000, 9.999999999998897304E-05 ),
 .UNSPECIFIED. ) ;
#56924 = ADVANCED_FACE ( 'NONE', ( #55654 ), #32799, .F. ) ;
#56925 = CARTESIAN_POINT ( 'NONE',  ( -32.52200313167130474, -23.48783264082477729, -1.443836473390076147 ) ) ;
#56926 = CARTESIAN_POINT ( 'NONE',  ( -127.6248241772779437, -23.48786465467242124, 11.44779295918253403 ) ) ;
#56927 = ORIENTED_EDGE ( 'NONE', *, *, #28440, .F. ) ;
#56928 = FACE_OUTER_BOUND ( 'NONE', #6875, .T. ) ;
#56929 = CARTESIAN_POINT ( 'NONE',  ( -49.31927893949910668, -25.26264030274095163, 6.419594040249337219 ) ) ;
#56930 = CARTESIAN_POINT ( 'NONE',  ( -65.62287095715008434, -24.82576562982392687, 8.398263435472971494 ) ) ;
#56931 = CARTESIAN_POINT ( 'NONE',  ( 10.59196434753715010, 18.29633683537252509, 11.49999999999999645 ) ) ;
#56932 = CARTESIAN_POINT ( 'NONE',  ( 22.09269804725545683, -1.632937629565654580, 11.49999999999998934 ) ) ;
#56933 = VECTOR ( 'NONE', #94661, 1000.000000000000000 ) ;
#56934 = CARTESIAN_POINT ( 'NONE',  ( -20.17529555308526668, -4.016306826964139098, 11.49999999999998934 ) ) ;
#56935 = ORIENTED_EDGE ( 'NONE', *, *, #24395, .F. ) ;
#56936 = CARTESIAN_POINT ( 'NONE',  ( -41.49214519350802988, -24.34968618360933590, 0.1864209137778857495 ) ) ;
#56937 = EDGE_LOOP ( 'NONE', ( #31027, #98099, #96156, #19213 ) ) ;
#56938 = DIRECTION ( 'NONE',  ( 0.000000000000000000, 0.9999999999976377785, 2.173523156925979975E-06 ) ) ;
#56939 = CARTESIAN_POINT ( 'NONE',  ( -61.62287095715007013, -24.35013146730203104, 9.818937971375115481 ) ) ;
#56940 = ORIENTED_EDGE ( 'NONE', *, *, #1223, .T. ) ;
#56941 = ORIENTED_EDGE ( 'NONE', *, *, #89217, .F. ) ;
#56942 = B_SPLINE_CURVE_WITH_KNOTS ( 'NONE', 3,
 ( #29514, #93410, #69594, #75682 ),
 .UNSPECIFIED., .F., .F.,
 ( 4, 4 ),
 ( 2.775557561562891043E-17, 9.999999999996124456E-05 ),
 .UNSPECIFIED. ) ;
#56943 = EDGE_LOOP ( 'NONE', ( #38866, #54836, #67814, #80715 ) ) ;
#56944 = DIRECTION ( 'NONE',  ( -0.000000000000000000, 1.000000000000000000, -0.000000000000000000 ) ) ;
#56945 = CARTESIAN_POINT ( 'NONE',  ( 6.963174204274080736, -6.376774720514415407, 20.29202897614545975 ) ) ;
#56946 = CARTESIAN_POINT ( 'NONE',  ( 5.873458226074941280, -6.376774720514413630, 19.84669099281175164 ) ) ;
#56947 = CARTESIAN_POINT ( 'NONE',  ( -6.067718162532647064, 19.77315050736717694, -1.500000000000002220 ) ) ;
#56948 = CARTESIAN_POINT ( 'NONE',  ( -0.4625342273119020797, 21.68341340789531912, 11.49999999999999645 ) ) ;
#56949 = EDGE_LOOP ( 'NONE', ( #87107, #92854, #98610 ) ) ;
#56950 = CARTESIAN_POINT ( 'NONE',  ( 19.75748517575715368, 5.965225279485572685, 28.87153971905864580 ) ) ;
#56951 = CARTESIAN_POINT ( 'NONE',  ( -111.4927656110371714, -25.20245619288051131, 3.420186212457718256 ) ) ;
#56952 = CARTESIAN_POINT ( 'NONE',  ( -3.217810451210200817, -22.18463865543611391, -1.500000000000002220 ) ) ;
#56953 = CARTESIAN_POINT ( 'NONE',  ( -124.6228709571500559, -23.48783264082479505, -1.443836473390058828 ) ) ;
#56954 = CARTESIAN_POINT ( 'NONE',  ( -71.62287095715004170, -23.96127896941632685, -0.6493128931037889240 ) ) ;
#56956 = ORIENTED_EDGE ( 'NONE', *, *, #29886, .T. ) ;
#56955 = EDGE_CURVE ( 'NONE', #27253, #35212, #39412, .T. ) ;
#56957 = LINE ( 'NONE', #26497, #33914 ) ;
#56958 = VECTOR ( 'NONE', #92048, 1000.000000000000000 ) ;
#56959 = CARTESIAN_POINT ( 'NONE',  ( -35.59333913237350089, -24.40133493613049609, 9.663955038902800609 ) ) ;
#56960 = ORIENTED_EDGE ( 'NONE', *, *, #53240, .T. ) ;
#56961 = VERTEX_POINT ( 'NONE', #69362 ) ;
#56962 = DIRECTION ( 'NONE',  ( -0.000000000000000000, 0.7682212795973760722, 0.6401843996644797086 ) ) ;
#56963 = ORIENTED_EDGE ( 'NONE', *, *, #1952, .T. ) ;
#56964 = ADVANCED_FACE ( 'NONE', ( #71373 ), #55152, .F. ) ;
#56965 = DIRECTION ( 'NONE',  ( -0.000000000000000000, -0.000000000000000000, -1.000000000000000000 ) ) ;
#56966 = CARTESIAN_POINT ( 'NONE',  ( -20.47598858559898716, 5.595549388561865456, -1.500000000000002220 ) ) ;
#56967 = ORIENTED_EDGE ( 'NONE', *, *, #996, .F. ) ;
#56968 = DIRECTION ( 'NONE',  ( 0.000000000000000000, -1.000000000000000000, 0.000000000000000000 ) ) ;
#56969 = CARTESIAN_POINT ( 'NONE',  ( -12.45635911906152771, -17.91357634596933934, 11.49999999999998934 ) ) ;
#56970 = CARTESIAN_POINT ( 'NONE',  ( -52.57794027106912438, -24.66019654487198665, 8.947790411086131712 ) ) ;
#56971 = DIRECTION ( 'NONE',  ( 0.000000000000000000, -0.000000000000000000, -1.000000000000000000 ) ) ;
#56972 = PLANE ( 'NONE',  #41726 ) ;
#56973 = CARTESIAN_POINT ( 'NONE',  ( 21.45948982579844255, -4.128456637845983934, -1.500000000000002220 ) ) ;
#56974 = CARTESIAN_POINT ( 'NONE',  ( -109.5228709571500758, -23.96177878511309345, 10.65340807706329329 ) ) ;
#56975 = ORIENTED_EDGE ( 'NONE', *, *, #42811, .F. ) ;
#56976 = CARTESIAN_POINT ( 'NONE',  ( 25.40542801349638680, 4.685157528325373910, -10.80549495980642583 ) ) ;
#56977 = CARTESIAN_POINT ( 'NONE',  ( -85.63196641622515415, -24.52399227489127043, 9.353111116836526406 ) ) ;
#56978 = VERTEX_POINT ( 'NONE', #15565 ) ;
#56979 = CARTESIAN_POINT ( 'NONE',  ( -30.60157315003009515, -24.66735617610590126, 1.103427580892887283 ) ) ;
#56980 = EDGE_LOOP ( 'NONE', ( #45161, #6592 ) ) ;
#56981 = DIRECTION ( 'NONE',  ( 0.000000000000000000, -1.000000000000000000, 0.000000000000000000 ) ) ;
#56982 = CARTESIAN_POINT ( 'NONE',  ( -82.59550824821182857, -23.96119346886881019, -0.6495511937831922600 ) ) ;
#56983 = CARTESIAN_POINT ( 'NONE',  ( 20.85495618715548716, -4.085033163991189653, -1.500000000000002220 ) ) ;
#56984 = LINE ( 'NONE', #87922, #7771 ) ;
#56985 = CARTESIAN_POINT ( 'NONE',  ( -130.5728709571500588, -24.87212640336025871, 1.420893871182737023 ) ) ;
#56986 = EDGE_CURVE ( 'NONE', #86130, #35546, #3531, .T. ) ;
#56987 = FACE_OUTER_BOUND ( 'NONE', #38736, .T. ) ;
#56988 = DIRECTION ( 'NONE',  ( 1.000000000000000000, 3.773278334444166432E-23, 8.201307841325785021E-29 ) ) ;
#56989 = CARTESIAN_POINT ( 'NONE',  ( -1.307668758097810358, 19.38731951181482671, -1.500000000000002220 ) ) ;
#56990 = VECTOR ( 'NONE', #70311, 1000.000000000000000 ) ;
#56991 = CARTESIAN_POINT ( 'NONE',  ( -28.47875734969026240, 5.965225279485572685, 26.43402280011862615 ) ) ;
#56992 = VERTEX_POINT ( 'NONE', #23673 ) ;
#56993 = CARTESIAN_POINT ( 'NONE',  ( -19.08498223313328168, 4.104482590468319536, 11.49999999999999645 ) ) ;
#56994 = DIRECTION ( 'NONE',  ( 0.000000000000000000, 0.000000000000000000, -1.000000000000000000 ) ) ;
#56996 = B_SPLINE_CURVE_WITH_KNOTS ( 'NONE', 3,
 ( #46868, #33137, #685, #32132 ),
 .UNSPECIFIED., .F., .F.,
 ( 4, 4 ),
 ( 0.000000000000000000, 9.999999999998897304E-05 ),
 .UNSPECIFIED. ) ;
#56995 = CARTESIAN_POINT ( 'NONE',  ( -29.52074223362913585, -25.06969336238594792, 6.937538283832196839 ) ) ;
#56997 = ORIENTED_EDGE ( 'NONE', *, *, #16315, .F. ) ;
#56998 = CARTESIAN_POINT ( 'NONE',  ( -58.62287095715006302, -23.95044443724992078, 10.65354141964650125 ) ) ;
#56999 = EDGE_CURVE ( 'NONE', #27856, #22224, #62847, .T. ) ;
#57000 = CARTESIAN_POINT ( 'NONE',  ( -89.62850960197191341, -24.34968618360933945, 0.1864209137778942982 ) ) ;
#57001 = ADVANCED_FACE ( 'NONE', ( #23164 ), #34439, .T. ) ;
#57002 = CYLINDRICAL_SURFACE ( 'NONE', #34262, 130.7884398600581335 ) ;
#57003 = CARTESIAN_POINT ( 'NONE',  ( -80.64549629918748508, -25.24813990744215886, 7.560538059850569148 ) ) ;
#57004 = CARTESIAN_POINT ( 'NONE',  ( -0.7274468246531539117, 19.66889477801398911, -1.500000000000002220 ) ) ;
#57005 = EDGE_CURVE ( 'NONE', #98963, #27719, #56199, .T. ) ;
#57006 = EDGE_LOOP ( 'NONE', ( #18492, #26506, #2688, #39310 ) ) ;
#57007 = AXIS2_PLACEMENT_3D ( 'NONE', #6449, #67861, #37406 ) ;
#57008 = DIRECTION ( 'NONE',  ( 0.000000000000000000, 0.000000000000000000, 1.000000000000000000 ) ) ;
#57009 = CARTESIAN_POINT ( 'NONE',  ( -114.5895376238167387, -23.47596703998600631, 11.44779298504227683 ) ) ;
#57010 = COORDINATED_UNIVERSAL_TIME_OFFSET ( 0, 0, .AHEAD. ) ;
#57011 = ORIENTED_EDGE ( 'NONE', *, *, #58155, .T. ) ;
#57012 = CARTESIAN_POINT ( 'NONE',  ( -125.5228709571500616, -23.48786465467241769, 11.44779295918253581 ) ) ;
#57013 = CARTESIAN_POINT ( 'NONE',  ( -2.188401442307694289, -6.376774720514411854, 19.46153846153846700 ) ) ;
#57014 = CARTESIAN_POINT ( 'NONE',  ( -115.6228709571500133, -24.63345952396256422, 9.038047939301501188 ) ) ;
#57015 = CARTESIAN_POINT ( 'NONE',  ( -97.51107724223938078, -24.35071581493543746, 9.817618358456025263 ) ) ;
#57016 = CARTESIAN_POINT ( 'NONE',  ( -81.90141697262173182, -25.33009845126374771, 4.495758016894969344 ) ) ;
#57017 = CARTESIAN_POINT ( 'NONE',  ( -69.38261850605717029, -25.24515179376014018, 5.944601484458109653 ) ) ;
#57018 = DIRECTION ( 'NONE',  ( -0.000000000000000000, -1.000000000000000000, -0.000000000000000000 ) ) ;
#57020 = ADVANCED_FACE ( 'NONE', ( #80974 ), #89587, .F. ) ;
#57019 = CARTESIAN_POINT ( 'NONE',  ( -18.79874323561663729, 6.599581278811135654, 11.49999999999998934 ) ) ;
#57021 = CARTESIAN_POINT ( 'NONE',  ( -75.64825312942650726, -23.85049219812685806, 10.88485053497527488 ) ) ;
#57022 = CARTESIAN_POINT ( 'NONE',  ( -18.60049703728633474, -6.982253431394513932, -1.500000000000002220 ) ) ;
#57023 = VERTEX_POINT ( 'NONE', #57161 ) ;
#57024 = CARTESIAN_POINT ( 'NONE',  ( -56.48830708450546467, -24.65952944569304250, 1.056160979905696795 ) ) ;
#57025 = CIRCLE ( 'NONE', #13245, 1.500000000000000666 ) ;
#57026 = PRODUCT_DEFINITION_FORMATION_WITH_SPECIFIED_SOURCE ( 'ANY', '', #50676, .NOT_KNOWN. ) ;
#57027 = CARTESIAN_POINT ( 'NONE',  ( -44.62287095715004881, -29.50250786944525672, 11.44777988621624232 ) ) ;
#57028 = CARTESIAN_POINT ( 'NONE',  ( -29.52287095715006870, -24.43005622135203936, 9.387565107222346938 ) ) ;
#57029 = CARTESIAN_POINT ( 'NONE',  ( 12.48433401490028949, -6.376774720514426953, -25.05541855807676299 ) ) ;
#57030 = CARTESIAN_POINT ( 'NONE',  ( -20.13249939377427111, -5.111880259578561514, 11.49999999999999645 ) ) ;
#57031 = CARTESIAN_POINT ( 'NONE',  ( -7.243541020599075786, -5.876774720514408301, 19.27798293355755632 ) ) ;
#57032 = EDGE_CURVE ( 'NONE', #91284, #94825, #39953, .T. ) ;
#57033 = CARTESIAN_POINT ( 'NONE',  ( 31.59111626279633711, 6.376774720514426953, 16.27760796525321751 ) ) ;
#57034 = CARTESIAN_POINT ( 'NONE',  ( 4.459850365305920938, 22.40387240153798487, 11.49999999999999645 ) ) ;
#57035 = ORIENTED_EDGE ( 'NONE', *, *, #88086, .T. ) ;
#57036 = FACE_OUTER_BOUND ( 'NONE', #81712, .T. ) ;
#57037 = EDGE_CURVE ( 'NONE', #49598, #234, #83292, .T. ) ;
#57038 = DIRECTION ( 'NONE',  ( -3.773278334453080206E-23, 0.9999999999976377785, 2.173523156925979975E-06 ) ) ;
#57039 = VERTEX_POINT ( 'NONE', #41418 ) ;
#57040 = CARTESIAN_POINT ( 'NONE',  ( -17.47620107869530770, 10.18187089365592612, -1.500000000000002220 ) ) ;
#57041 = CARTESIAN_POINT ( 'NONE',  ( 14.76093561896379214, -6.475225279485573360, -26.55548769130089681 ) ) ;
#57042 = EDGE_CURVE ( 'NONE', #48508, #42578, #95069, .T. ) ;
#57043 = B_SPLINE_CURVE_WITH_KNOTS ( 'NONE', 3,
 ( #94310, #11082, #49658, #2480 ),
 .UNSPECIFIED., .F., .F.,
 ( 4, 4 ),
 ( 0.000000000000000000, 1.000000000000000000 ),
 .UNSPECIFIED. ) ;
#57044 = CARTESIAN_POINT ( 'NONE',  ( 5.949073730962466833, 6.475225279485573360, -27.94053387008862188 ) ) ;
#57045 = ADVANCED_FACE ( 'NONE', ( #40912 ), #80471, .T. ) ;
#57046 = CARTESIAN_POINT ( 'NONE',  ( -50.52287095715006160, -23.48786465467241058, 11.44779295918255002 ) ) ;
#57047 = VERTEX_POINT ( 'NONE', #50524 ) ;
#57048 = CARTESIAN_POINT ( 'NONE',  ( -40.58953762381673158, -23.48786465467240347, 11.44779295918255180 ) ) ;
#57049 = CARTESIAN_POINT ( 'NONE',  ( -84.52287095715006160, -24.64965694238406613, 8.947790433994198267 ) ) ;
#57050 = CARTESIAN_POINT ( 'NONE',  ( 5.980626343040887249, -19.09133569553460319, -1.500000000000002220 ) ) ;
#57051 = CARTESIAN_POINT ( 'NONE',  ( -20.70934228997045068, 3.328930095467914185, 11.49999999999999645 ) ) ;
#57052 = FACE_OUTER_BOUND ( 'NONE', #19453, .T. ) ;
#57053 = CARTESIAN_POINT ( 'NONE',  ( -113.5228709571500616, -23.47593901973090524, -1.443836447538996204 ) ) ;
#57054 = CARTESIAN_POINT ( 'NONE',  ( 14.91618686576236108, -16.25093855066790738, -1.500000000000002220 ) ) ;
#57055 = B_SPLINE_CURVE_WITH_KNOTS ( 'NONE', 3,
 ( #78401, #85018, #60713, #22606 ),
 .UNSPECIFIED., .F., .F.,
 ( 4, 4 ),
 ( 0.7493128662882344582, 0.7503136133289997067 ),
 .UNSPECIFIED. ) ;
#57056 = CARTESIAN_POINT ( 'NONE',  ( -40.20932372006943467, -25.31589326768515491, 5.067940297764987889 ) ) ;
#57057 = ORIENTED_EDGE ( 'NONE', *, *, #49507, .T. ) ;
#57058 = VECTOR ( 'NONE', #21625, 1000.000000000000000 ) ;
#57059 = CARTESIAN_POINT ( 'NONE',  ( -47.58953762381671737, -24.65952944569304250, 1.056160979905693686 ) ) ;
#57060 = DIRECTION ( 'NONE',  ( 0.000000000000000000, 1.000000000000000000, 0.000000000000000000 ) ) ;
#57061 = DIRECTION ( 'NONE',  ( -0.000000000000000000, -0.000000000000000000, -1.000000000000000000 ) ) ;
#57062 = VERTEX_POINT ( 'NONE', #96207 ) ;
#57063 = CARTESIAN_POINT ( 'NONE',  ( 2.591645189881369493, -6.376774720514411854, 19.84288601127407148 ) ) ;
#57064 = ORIENTED_EDGE ( 'NONE', *, *, #43144, .F. ) ;
#57065 = EDGE_LOOP ( 'NONE', ( #71391, #29299, #27233, #51368 ) ) ;
#57066 = DIRECTION ( 'NONE',  ( 0.000000000000000000, -1.000000000000000000, 0.000000000000000000 ) ) ;
#57067 = DIRECTION ( 'NONE',  ( 0.000000000000000000, -1.000000000000000000, 0.000000000000000000 ) ) ;
#57068 = CARTESIAN_POINT ( 'NONE',  ( 14.76093561896378148, 3.316774720514426456, -26.55548769130088971 ) ) ;
#57069 = CARTESIAN_POINT ( 'NONE',  ( -18.81443736134900035, 8.205417114561466718, -1.500000000000002220 ) ) ;
#57070 = ORIENTED_EDGE ( 'NONE', *, *, #76010, .T. ) ;
#57071 = DIRECTION ( 'NONE',  ( -0.000000000000000000, -0.000000000000000000, -1.000000000000000000 ) ) ;
#57072 = FACE_OUTER_BOUND ( 'NONE', #60417, .T. ) ;
#57073 = CARTESIAN_POINT ( 'NONE',  ( -96.58953762381671027, -24.66019654487199730, 8.947790411086126383 ) ) ;
#57074 = CARTESIAN_POINT ( 'NONE',  ( -10.99827004860668822, -19.42154297629913628, -1.500000000000002220 ) ) ;
#57075 = CARTESIAN_POINT ( 'NONE',  ( 32.76111974776238611, -3.316774720514426900, -3.850861272813261849 ) ) ;
#57077 = EDGE_CURVE ( 'NONE', #26881, #55585, #63924, .T. ) ;
#57076 = CARTESIAN_POINT ( 'NONE',  ( -32.07722060962682775, -25.12026506542016335, 2.831122744435439209 ) ) ;
#57078 = ORIENTED_EDGE ( 'NONE', *, *, #56668, .T. ) ;
#57079 = CARTESIAN_POINT ( 'NONE',  ( -86.62287095715004170, -29.50250243563736774, 8.947779886222139822 ) ) ;
#57080 = CARTESIAN_POINT ( 'NONE',  ( -65.58953762381672448, -24.99132157543084176, 2.256160258750496084 ) ) ;
#57081 = AXIS2_PLACEMENT_3D ( 'NONE', #45636, #28397, #59361 ) ;
#57082 = CARTESIAN_POINT ( 'NONE',  ( -16.98601802344612111, -12.12340321765213069, -1.500000000000002220 ) ) ;
#57083 = AXIS2_PLACEMENT_3D ( 'NONE', #88845, #34553, #57409 ) ;
#57084 = ORIENTED_EDGE ( 'NONE', *, *, #1557, .F. ) ;
#57086 = ORIENTED_EDGE ( 'NONE', *, *, #63082, .F. ) ;
#57085 = CARTESIAN_POINT ( 'NONE',  ( -116.5228709571500474, -24.34917612407043563, 0.1852690917480298016 ) ) ;
#57087 = ORIENTED_EDGE ( 'NONE', *, *, #37970, .T. ) ;
#57088 = EDGE_CURVE ( 'NONE', #16367, #4780, #30236, .T. ) ;
#57089 = CARTESIAN_POINT ( 'NONE',  ( -32.50560601784287229, -24.86181184613565165, 1.747789954104514987 ) ) ;
#57090 = CARTESIAN_POINT ( 'NONE',  ( 20.41947327098772647, -5.118016103960565388, -1.500000000000002220 ) ) ;
#57091 = VERTEX_POINT ( 'NONE', #42434 ) ;
#57092 = CARTESIAN_POINT ( 'NONE',  ( 8.160000000000000142, -10.15233964170348457, 0.003711184059992174607 ) ) ;
#57093 = CARTESIAN_POINT ( 'NONE',  ( -53.52287095715006870, -24.64965694238574656, 8.947790433994203596 ) ) ;
#57094 = CARTESIAN_POINT ( 'NONE',  ( -120.5530840431339925, -24.73531770709095312, 8.716586749053508498 ) ) ;
#57095 = CARTESIAN_POINT ( 'NONE',  ( -101.9401486745561272, -25.03152172299557066, 6.289339500554307349 ) ) ;
#57096 = FACE_OUTER_BOUND ( 'NONE', #73528, .T. ) ;
#57097 = CARTESIAN_POINT ( 'NONE',  ( 9.217229664113554932, 19.63635308506117383, -1.500000000000002220 ) ) ;
#57098 = CARTESIAN_POINT ( 'NONE',  ( -80.72310326078591913, -25.12224386673238286, 7.076933481137675841 ) ) ;
#57100 = ORIENTED_EDGE ( 'NONE', *, *, #62876, .F. ) ;
#57099 = CARTESIAN_POINT ( 'NONE',  ( -10.38793682863964563, 19.71736701935523683, 11.49999999999999645 ) ) ;
#57101 = LINE ( 'NONE', #79912, #42112 ) ;
#57102 = CARTESIAN_POINT ( 'NONE',  ( -25.92875734969025814, 5.356774720514425603, 26.43402280011862615 ) ) ;
#57103 = FACE_OUTER_BOUND ( 'NONE', #26811, .T. ) ;
#57104 = ORIENTED_EDGE ( 'NONE', *, *, #56542, .F. ) ;
#57106 = ORIENTED_EDGE ( 'NONE', *, *, #59623, .F. ) ;
#57105 = CARTESIAN_POINT ( 'NONE',  ( -120.5228709571500616, -29.50247984919015209, -1.443849546365046699 ) ) ;
#57107 = VECTOR ( 'NONE', #14060, 1000.000000000000000 ) ;
#57108 = ORIENTED_EDGE ( 'NONE', *, *, #40335, .T. ) ;
#57109 = APPROVAL_PERSON_ORGANIZATION ( #98030, #92807, #81826 ) ;
#57110 = CARTESIAN_POINT ( 'NONE',  ( -47.52287095715006160, -24.64965694238406613, 8.947790433994203596 ) ) ;
#57111 = EDGE_CURVE ( 'NONE', #71528, #65697, #66253, .T. ) ;
#57112 = DIRECTION ( 'NONE',  ( -0.000000000000000000, -0.000000000000000000, -1.000000000000000000 ) ) ;
#57113 = DIRECTION ( 'NONE',  ( -0.000000000000000000, -1.000000000000000000, -0.000000000000000000 ) ) ;
#57114 = EDGE_LOOP ( 'NONE', ( #97750, #80135, #11970, #79497 ) ) ;
#57115 = CARTESIAN_POINT ( 'NONE',  ( -130.5728709571500588, -24.88728116469533447, 1.475554971460544262 ) ) ;
#57116 = CARTESIAN_POINT ( 'NONE',  ( 11.64234319522276095, -19.14997049866658330, -1.500000000000002220 ) ) ;
#57117 = VERTEX_POINT ( 'NONE', #72375 ) ;
#57118 = FACE_OUTER_BOUND ( 'NONE', #5765, .T. ) ;
#57119 = CARTESIAN_POINT ( 'NONE',  ( -101.5221917529393210, -23.48786465467241413, 11.44779295918254469 ) ) ;
#57120 = LINE ( 'NONE', #8921, #42544 ) ;
#57121 = ADVANCED_FACE ( 'NONE', ( #87592 ), #49542, .T. ) ;
#57122 = EDGE_CURVE ( 'NONE', #11758, #83886, #3866, .T. ) ;
#57123 = CARTESIAN_POINT ( 'NONE',  ( 26.25551457520356635, 500000.0000000000582, -10.59759736550661913 ) ) ;
#57124 = EDGE_CURVE ( 'NONE', #98244, #64840, #2361, .T. ) ;
#57125 = CARTESIAN_POINT ( 'NONE',  ( -130.5728709571500588, -24.37907397113050223, 9.703205396196697308 ) ) ;
#57126 = CARTESIAN_POINT ( 'NONE',  ( -14.26233628608129855, 13.40890954296891024, 11.49999999999998934 ) ) ;
#57127 = B_SPLINE_SURFACE_WITH_KNOTS ( 'NONE', 3, 1, ( 
 ( #8721, #85838 ),
 ( #84829, #69621 ),
 ( #54898, #39657 ),
 ( #63021, #93944 ),
 ( #85326, #16321 ),
 ( #31546, #15816 ),
 ( #46779, #1614 ),
 ( #102, #86341 ),
 ( #77705, #31040 ),
 ( #71122, #70615 ),
 ( #7708, #62007 ),
 ( #92437, #93436 ),
 ( #94450, #16824 ),
 ( #23931, #24932 ),
 ( #70114, #22904 ),
 ( #24432, #53897 ),
 ( #62508, #8218 ),
 ( #47284, #78211 ),
 ( #39157, #1106 ) ),
 .UNSPECIFIED., .F., .F., .F.,
 ( 4, 1, 1, 1, 1, 1, 1, 1, 1, 1, 1, 1, 1, 1, 1, 1, 4 ),
 ( 2, 2 ),
 ( 0.000000000000000000, 0.06196540068706264670, 0.1221219056382944895, 0.1809884968498423341, 0.2399332164519021315, 0.2999058311065245230, 0.3599888474769850633, 0.4217757417416482246, 0.4865758264211246797, 0.5515348046197418030, 0.6150175427599803291, 0.6772586166616564318, 0.7397299623627153764, 0.8030501026629509598, 0.8664951320156968340, 0.9319734741771505959, 1.000000000000000000 ),
 ( 0.000000000000000000, 1.000000000000000000 ),
 .UNSPECIFIED. ) ;
#57128 = CARTESIAN_POINT ( 'NONE',  ( -50.12325739912953537, -25.31187256814138919, 4.701396598943802019 ) ) ;
#57130 = EDGE_CURVE ( 'NONE', #57364, #93093, #73862, .T. ) ;
#57129 = ORIENTED_EDGE ( 'NONE', *, *, #90952, .T. ) ;
#57131 = CARTESIAN_POINT ( 'NONE',  ( 4.075586527997184128, 21.15050231453075824, -1.500000000000002220 ) ) ;
#57132 = CARTESIAN_POINT ( 'NONE',  ( 15.99960863614631101, -3.577630190450212577, -27.91116951066581819 ) ) ;
#57133 = CARTESIAN_POINT ( 'NONE',  ( -119.5228709571500758, -23.47596703998600631, 11.44779298504227860 ) ) ;
#57134 = CARTESIAN_POINT ( 'NONE',  ( -107.6228709571500701, -23.48783264082479150, -1.443836473390060382 ) ) ;
#57135 = LINE ( 'NONE', #88070, #5078 ) ;
#57136 = CARTESIAN_POINT ( 'NONE',  ( -4.681240387505234857, -22.43558246840685300, -1.500000000000002220 ) ) ;
#57137 = AXIS2_PLACEMENT_3D ( 'NONE', #14029, #99272, #4579 ) ;
#57138 = COORDINATED_UNIVERSAL_TIME_OFFSET ( 0, 0, .AHEAD. ) ;
#57139 = CARTESIAN_POINT ( 'NONE',  ( -93.62287095715007013, -23.73907113216991860, -1.053371485793227924 ) ) ;
#57140 = DIRECTION ( 'NONE',  ( -0.7640209514960704107, 0.000000000000000000, 0.6451914333552789538 ) ) ;
#57141 = CARTESIAN_POINT ( 'NONE',  ( -16.95507112718987486, -10.73317591066004084, 11.49999999999999645 ) ) ;
#57142 = CARTESIAN_POINT ( 'NONE',  ( 5.085443162053245203, 3.316774720514426456, -27.56355752155217331 ) ) ;
#57143 = CARTESIAN_POINT ( 'NONE',  ( -32.64292555811511676, -24.15620529776627734, 10.23563542870661358 ) ) ;
#57144 = CARTESIAN_POINT ( 'NONE',  ( 0.5964549592197745387, 8.529703308962702124, -1.700000000000008837 ) ) ;
#57145 = PLANE ( 'NONE',  #3485 ) ;
#57146 = CARTESIAN_POINT ( 'NONE',  ( -96.52287095715006160, -23.47596703998600631, 11.44779298504228215 ) ) ;
#57147 = EDGE_CURVE ( 'NONE', #92122, #92240, #95201, .T. ) ;
#57149 = EDGE_CURVE ( 'NONE', #59834, #83063, #52912, .T. ) ;
#57148 = CARTESIAN_POINT ( 'NONE',  ( 19.84127317031322946, -0.4231496731191971561, -1.500000000000002220 ) ) ;
#57150 = DIRECTION ( 'NONE',  ( 0.000000000000000000, 0.000000000000000000, 1.000000000000000000 ) ) ;
#57151 = CARTESIAN_POINT ( 'NONE',  ( -16.88869819569221065, 10.18974688345344148, -1.500000000000002220 ) ) ;
#57152 = FACE_OUTER_BOUND ( 'NONE', #32956, .T. ) ;
#57153 = ADVANCED_FACE ( 'NONE', ( #6339 ), #67760, .T. ) ;
#57154 = DIRECTION ( 'NONE',  ( 0.000000000000000000, 1.000000000000000000, 0.000000000000000000 ) ) ;
#57155 = CALENDAR_DATE ( 2026, 9, 10 ) ;
#57156 = VECTOR ( 'NONE', #80961, 1000.000000000000114 ) ;
#57157 = LINE ( 'NONE', #58147, #84027 ) ;
#57158 = CARTESIAN_POINT ( 'NONE',  ( -111.5228709571500616, -23.73907113216990439, -1.053371485793247242 ) ) ;
#57159 = CARTESIAN_POINT ( 'NONE',  ( -19.88974639711211623, -5.441847772814488948, 11.49999999999999645 ) ) ;
#57160 = ADVANCED_FACE ( 'NONE', ( #51031 ), #75342, .F. ) ;
#57161 = CARTESIAN_POINT ( 'NONE',  ( 28.30015606816038698, 1.682774720514426114, -13.13501953239208575 ) ) ;
#57162 = CARTESIAN_POINT ( 'NONE',  ( 14.74224262856723833, 17.19160420931263999, 11.49999999999999645 ) ) ;
#57163 = ORIENTED_EDGE ( 'NONE', *, *, #52409, .T. ) ;
#57164 = CARTESIAN_POINT ( 'NONE',  ( -102.5895376238167103, -24.65952944569304606, 1.056160979905698571 ) ) ;
#57165 = CARTESIAN_POINT ( 'NONE',  ( -97.62752529066908380, -24.34968618360934300, 0.1864209137778856384 ) ) ;
#57166 = CARTESIAN_POINT ( 'NONE',  ( -27.61431623538372548, -24.77705460396850512, 2.278732773682637269 ) ) ;
#57167 = CARTESIAN_POINT ( 'NONE',  ( -127.5228709571500900, -23.72773821059536914, 11.05748984161097326 ) ) ;
#57168 = ADVANCED_FACE ( 'NONE', ( #98681 ), #17357, .F. ) ;
#57169 = LINE ( 'NONE', #17078, #77160 ) ;
#57170 = EDGE_CURVE ( 'NONE', #6520, #51171, #14274, .T. ) ;
#57171 = ORIENTED_EDGE ( 'NONE', *, *, #8595, .F. ) ;
#57172 = CIRCLE ( 'NONE', #39323, 4.300000000000000711 ) ;
#57173 = CARTESIAN_POINT ( 'NONE',  ( -79.34938298551102775, -25.31596414855141930, 5.853656268619368497 ) ) ;
#57174 = CARTESIAN_POINT ( 'NONE',  ( -18.62658236799572720, 13.20813282334384553, -1.500000000000002220 ) ) ;
#57176 = EDGE_CURVE ( 'NONE', #69024, #19418, #21056, .T. ) ;
#57175 = CARTESIAN_POINT ( 'NONE',  ( 16.00000000000000000, 2.939152317953647894E-15, -24.00000000000000000 ) ) ;
#57177 = CARTESIAN_POINT ( 'NONE',  ( -96.50665353833102245, -24.65952944569305316, 1.056160979905706121 ) ) ;
#57178 = CARTESIAN_POINT ( 'NONE',  ( -82.59187514100537442, -24.15620529776628089, 10.23563542870660825 ) ) ;
#57179 = CC_DESIGN_SECURITY_CLASSIFICATION ( #21497, ( #63621 ) ) ;
#57180 = CARTESIAN_POINT ( 'NONE',  ( -14.31525571501011207, 17.33968770572689166, 11.49999999999999645 ) ) ;
#57181 = ORIENTED_EDGE ( 'NONE', *, *, #68881, .T. ) ;
#57182 = DIRECTION ( 'NONE',  ( 0.000000000000000000, -0.000000000000000000, -1.000000000000000000 ) ) ;
#57183 = CARTESIAN_POINT ( 'NONE',  ( -20.58003014649542095, 7.718188279156099618, 11.49999999999998934 ) ) ;
#57184 = CARTESIAN_POINT ( 'NONE',  ( 31.74473449900405697, 4.976825198871215328, -4.259190951192157293 ) ) ;
#57185 = CARTESIAN_POINT ( 'NONE',  ( -111.5955121331480910, -23.48783264082477729, -1.443836473390087249 ) ) ;
#57186 = DIRECTION ( 'NONE',  ( 0.000000000000000000, -2.173523156925980399E-06, 0.9999999999976378895 ) ) ;
#57187 = AXIS2_PLACEMENT_3D ( 'NONE', #64898, #88210, #18678 ) ;
#57188 = ORIENTED_EDGE ( 'NONE', *, *, #15865, .T. ) ;
#57189 = CARTESIAN_POINT ( 'NONE',  ( -11.64875734969026233, 5.965225279485572685, 31.02402280011862246 ) ) ;
#57190 = CARTESIAN_POINT ( 'NONE',  ( -107.5228709571500900, -24.50321055353805377, 9.387540953477515160 ) ) ;
#57191 = ORIENTED_EDGE ( 'NONE', *, *, #48887, .F. ) ;
#57192 = CARTESIAN_POINT ( 'NONE',  ( -54.63280671366005947, -24.35071581493543391, 9.817618358456034144 ) ) ;
#57193 = CARTESIAN_POINT ( 'NONE',  ( 19.38413035786728145, -6.671778716439519030, 11.49999999999998934 ) ) ;
#57194 = EDGE_LOOP ( 'NONE', ( #69753, #90734, #6646, #2152 ) ) ;
#57195 = ORIENTED_EDGE ( 'NONE', *, *, #37785, .T. ) ;
#57196 = AXIS2_PLACEMENT_3D ( 'NONE', #11034, #34374, #1428 ) ;
#57197 = ORIENTED_EDGE ( 'NONE', *, *, #95007, .F. ) ;
#57198 = CARTESIAN_POINT ( 'NONE',  ( 2.911360383046243783, -6.376774720514417183, 20.24673073119071276 ) ) ;
#57199 = CARTESIAN_POINT ( 'NONE',  ( 22.28998074345494729, -6.091270044117925053, 11.49999999999998934 ) ) ;
#57200 = CARTESIAN_POINT ( 'NONE',  ( -41.52287095715008292, -24.35013146730203815, 9.818937971375104823 ) ) ;
#57201 = CARTESIAN_POINT ( 'NONE',  ( -9.871001836803966256, -17.81128643866572148, -1.500000000000002220 ) ) ;
#57202 = ORIENTED_EDGE ( 'NONE', *, *, #1444, .T. ) ;
#57203 = CARTESIAN_POINT ( 'NONE',  ( -71.18365115483554462, -25.08868281807281519, 7.289250223163644016 ) ) ;
#57204 = CARTESIAN_POINT ( 'NONE',  ( -29.53717958776107366, -24.26755322398480885, 9.817618405055078767 ) ) ;
#57205 = B_SPLINE_CURVE_WITH_KNOTS ( 'NONE', 3,
 ( #80404, #2796, #87012, #57089 ),
 .UNSPECIFIED., .F., .F.,
 ( 4, 4 ),
 ( 3.169701060731301374E-09, 0.001213954044779386957 ),
 .UNSPECIFIED. ) ;
#57206 = CARTESIAN_POINT ( 'NONE',  ( -40.52287095715006870, -23.47596703998600631, 11.44779298504229281 ) ) ;
#57207 = CARTESIAN_POINT ( 'NONE',  ( -71.03336120160147971, -25.03149811950544645, 7.389033691368496193 ) ) ;
#57208 = ORIENTED_EDGE ( 'NONE', *, *, #99918, .T. ) ;
#57209 = CARTESIAN_POINT ( 'NONE',  ( -28.81395509834238311, -25.21531791893868402, 2.889655623812062313 ) ) ;
#57210 = CARTESIAN_POINT ( 'NONE',  ( -49.10641598061040725, -25.26385650276297667, 4.048599411326989639 ) ) ;
#57211 = B_SPLINE_CURVE_WITH_KNOTS ( 'NONE', 3,
 ( #84174, #22762, #14664, #84676 ),
 .UNSPECIFIED., .F., .F.,
 ( 4, 4 ),
 ( 0.000000000000000000, 0.0001000000000000028644 ),
 .UNSPECIFIED. ) ;
#57212 = VERTEX_POINT ( 'NONE', #22049 ) ;
#57213 = CARTESIAN_POINT ( 'NONE',  ( -19.91680486407696904, 5.911688619927280008, 11.49999999999998934 ) ) ;
#57214 = VERTEX_POINT ( 'NONE', #82465 ) ;
#57216 = ORIENTED_EDGE ( 'NONE', *, *, #8811, .T. ) ;
#57215 = CARTESIAN_POINT ( 'NONE',  ( -125.6246441017137840, -24.40034930558991633, 0.3402023900116222244 ) ) ;
#57217 = AXIS2_PLACEMENT_3D ( 'NONE', #4329, #34773, #2332 ) ;
#57218 = B_SPLINE_SURFACE_WITH_KNOTS ( 'NONE', 3, 3, ( 
 ( #49064, #370, #31317, #876 ),
 ( #62798, #62287, #94717, #93712 ),
 ( #55179, #39934, #70896, #1387 ),
 ( #32322, #63294, #56180, #94213 ),
 ( #32825, #87105, #34330, #81997 ),
 ( #82486, #28208, #19587, #65798 ),
 ( #35824, #10987, #95723, #73394 ) ),
 .UNSPECIFIED., .F., .F., .F.,
 ( 4, 3, 4 ),
 ( 4, 4 ),
 ( 0.7945040050992238090, 0.8970133687736503436, 0.9995227324480768782 ),
 ( 0.8597124620935061579, 0.8611220869707849612 ),
 .UNSPECIFIED. ) ;
#57219 = CARTESIAN_POINT ( 'NONE',  ( -122.6228709571500417, -24.64965695001469115, 8.947790433994175174 ) ) ;
#57220 = CARTESIAN_POINT ( 'NONE',  ( -51.82604781446892162, -25.28888632563197802, 5.652223579025216438 ) ) ;
#57221 = ORIENTED_EDGE ( 'NONE', *, *, #99358, .T. ) ;
#57222 = ORIENTED_EDGE ( 'NONE', *, *, #27010, .T. ) ;
#57223 = DIRECTION ( 'NONE',  ( 1.000000000000000000, -0.000000000000000000, -0.000000000000000000 ) ) ;
#57224 = DIRECTION ( 'NONE',  ( 0.000000000000000000, -0.7071067811865513475, -0.7071067811865436870 ) ) ;
#57225 = FACE_OUTER_BOUND ( 'NONE', #7578, .T. ) ;
#57227 = ORIENTED_EDGE ( 'NONE', *, *, #8788, .F. ) ;
#57226 = CARTESIAN_POINT ( 'NONE',  ( -13.58966412916292299, 17.40808962483262690, 11.49999999999999645 ) ) ;
#57228 = CARTESIAN_POINT ( 'NONE',  ( -48.88077023010853850, -25.24573983383035269, 6.307065433768737961 ) ) ;
#57229 = VECTOR ( 'NONE', #13867, 1000.000000000000114 ) ;
#57230 = CARTESIAN_POINT ( 'NONE',  ( -14.16962031475959272, 17.58799634409329471, -1.500000000000002220 ) ) ;
#57232 = ORIENTED_EDGE ( 'NONE', *, *, #17255, .T. ) ;
#57231 = CARTESIAN_POINT ( 'NONE',  ( -129.5228709571500758, -23.47593901973090524, -1.443836447538996204 ) ) ;
#57233 = AXIS2_PLACEMENT_3D ( 'NONE', #97051, #17934, #64641 ) ;
#57234 = ORIENTED_EDGE ( 'NONE', *, *, #98537, .F. ) ;
#57235 = PLANE ( 'NONE',  #6135 ) ;
#57236 = CARTESIAN_POINT ( 'NONE',  ( -94.55620429048339304, -24.64898659630529210, 1.056161002820827699 ) ) ;
#57237 = EDGE_LOOP ( 'NONE', ( #16591, #88400, #74912, #88256 ) ) ;
#57238 = CARTESIAN_POINT ( 'NONE',  ( -18.51692787870624102, -10.26217664800131502, -1.500000000000002220 ) ) ;
#57239 = EDGE_CURVE ( 'NONE', #52986, #13454, #48077, .T. ) ;
#57240 = CARTESIAN_POINT ( 'NONE',  ( 30.58729439590573307, -4.540774720514427543, 26.14186284044631492 ) ) ;
#57241 = CARTESIAN_POINT ( 'NONE',  ( -69.62287095715005592, -29.50250786944525672, 11.44777988621623699 ) ) ;
#57242 = CARTESIAN_POINT ( 'NONE',  ( 5.796264663052079769, -21.44337444023769379, -1.500000000000002220 ) ) ;
#57243 = EDGE_CURVE ( 'NONE', #11758, #81218, #36798, .T. ) ;
#57244 = CARTESIAN_POINT ( 'NONE',  ( -19.80875734969026425, 0.3587747205144265483, 31.02402280011862246 ) ) ;
#57245 = B_SPLINE_CURVE_WITH_KNOTS ( 'NONE', 3,
 ( #31644, #85939, #84435, #62613 ),
 .UNSPECIFIED., .F., .F.,
 ( 4, 4 ),
 ( 0.4701216268238749829, 0.4791280580959905167 ),
 .UNSPECIFIED. ) ;
#57246 = EDGE_CURVE ( 'NONE', #396, #86154, #13445, .T. ) ;
#57247 = VERTEX_POINT ( 'NONE', #59145 ) ;
#57248 = CARTESIAN_POINT ( 'NONE',  ( 6.437068816671457583, -3.316774720514427344, -28.37834077173919667 ) ) ;
#57249 = LINE ( 'NONE', #3455, #80020 ) ;
#57250 = EDGE_CURVE ( 'NONE', #68269, #40045, #90085, .T. ) ;
#57251 = EDGE_CURVE ( 'NONE', #35157, #56064, #55455, .T. ) ;
#57252 = CARTESIAN_POINT ( 'NONE',  ( -36.47910878338743856, -24.66019654487199730, 8.947790411086113949 ) ) ;
#57253 = LINE ( 'NONE', #11544, #48618 ) ;
#57254 = VECTOR ( 'NONE', #87700, 1000.000000000000000 ) ;
#57255 = CARTESIAN_POINT ( 'NONE',  ( 19.46547125265945155, -1.073068822128883104, -1.500000000000002220 ) ) ;
#57256 = ORGANIZATION ( 'NAUO-ORG4', 'UNSPECIFIED', 'UNSPECIFIED' ) ;
#57257 = CARTESIAN_POINT ( 'NONE',  ( 20.36625868517733196, 6.724766957447481097, 11.49999999999998934 ) ) ;
#57258 = CARTESIAN_POINT ( 'NONE',  ( 9.150000000000000355, -6.376774720514426953, -15.70000000000000284 ) ) ;
#57259 = CARTESIAN_POINT ( 'NONE',  ( -0.4909855769230798139, -5.876774720514408301, 19.14743589743590135 ) ) ;
#57261 = B_SPLINE_CURVE_WITH_KNOTS ( 'NONE', 3,
 ( #46340, #99605, #30610, #52966 ),
 .UNSPECIFIED., .F., .F.,
 ( 4, 4 ),
 ( 0.000000000000000000, 9.999999999998897304E-05 ),
 .UNSPECIFIED. ) ;
#57260 = LINE ( 'NONE', #18661, #73539 ) ;
#57262 = CARTESIAN_POINT ( 'NONE',  ( 21.04450177026006230, 8.645109164175620364, -1.500000000000002220 ) ) ;
#57263 = VECTOR ( 'NONE', #52490, 1000.000000000000000 ) ;
#57264 = DIRECTION ( 'NONE',  ( 0.9780042670096485979, 7.494612801694890537E-17, 0.2085848837066585637 ) ) ;
#57265 = CARTESIAN_POINT ( 'NONE',  ( -102.6251342045818120, -24.51314013834316086, 0.6176544820404232805 ) ) ;
#57266 = CARTESIAN_POINT ( 'NONE',  ( -101.6228709571500559, -24.66019654487199730, 8.947790411086121054 ) ) ;
#57267 = CARTESIAN_POINT ( 'NONE',  ( -19.91179686852411734, 0.6080443046932394457, 11.49999999999999645 ) ) ;
#57268 = CARTESIAN_POINT ( 'NONE',  ( -100.4498239493576648, -29.50249942614374277, 7.563164501610023294 ) ) ;
#57269 = VECTOR ( 'NONE', #8009, 1000.000000000000000 ) ;
#57270 = CARTESIAN_POINT ( 'NONE',  ( -39.59379972882672405, -24.15620529776628089, 10.23563542870661180 ) ) ;
#57271 = CARTESIAN_POINT ( 'NONE',  ( -48.60673731413511689, -23.73766607897670866, -1.055555164236436250 ) ) ;
#57272 = ORIENTED_EDGE ( 'NONE', *, *, #39819, .T. ) ;
#57273 = CARTESIAN_POINT ( 'NONE',  ( -7.326923076923076650, -6.376774720514417183, 20.36318108974359831 ) ) ;
#57274 = ADVANCED_FACE ( 'NONE', ( #72198 ), #72698, .F. ) ;
#57275 = CARTESIAN_POINT ( 'NONE',  ( -62.62287095715004881, -23.47596703998600276, 11.44779298504227505 ) ) ;
#57276 = CARTESIAN_POINT ( 'NONE',  ( 19.61570337458852364, 9.273991169892711994, -1.500000000000002220 ) ) ;
#57277 = CARTESIAN_POINT ( 'NONE',  ( -84.52287095715006160, -23.48786465467241769, 11.44779295918254469 ) ) ;
#57278 = CARTESIAN_POINT ( 'NONE',  ( -1.081029368968937421, 19.50181592447522050, -1.500000000000002220 ) ) ;
#57279 = CYLINDRICAL_SURFACE ( 'NONE', #57187, 1.836000000000000743 ) ;
#57280 = EDGE_CURVE ( 'NONE', #59933, #48082, #41755, .T. ) ;
#57281 = VERTEX_POINT ( 'NONE', #64609 ) ;
#57282 = PERSON_AND_ORGANIZATION_ROLE ( 'creator' ) ;
#57283 = LINE ( 'NONE', #49656, #54853 ) ;
#57284 = CARTESIAN_POINT ( 'NONE',  ( -11.47117155886032158, -16.94740806926979815, 11.49999999999999645 ) ) ;
#57285 = FACE_OUTER_BOUND ( 'NONE', #39210, .T. ) ;
#57286 = CARTESIAN_POINT ( 'NONE',  ( -39.62287095715005592, -23.47596703998600276, 11.44779298504227505 ) ) ;
#57287 = VERTEX_POINT ( 'NONE', #49368 ) ;
#57288 = CARTESIAN_POINT ( 'NONE',  ( 24.50000000000000000, -0.9000000000000000222, -1.103411337323757957 ) ) ;
#57289 = CARTESIAN_POINT ( 'NONE',  ( -66.52287095715006160, -24.64898659630528854, 1.056161002820824368 ) ) ;
#57290 = CARTESIAN_POINT ( 'NONE',  ( 7.480769230769231726, -6.376774720514420736, 20.77403846153845635 ) ) ;
#57291 = DIRECTION ( 'NONE',  ( 0.000000000000000000, 0.9999999999976377785, 2.173523156925979128E-06 ) ) ;
#57292 = CARTESIAN_POINT ( 'NONE',  ( -67.55620429048342146, -23.47596703998600276, 11.44779298504227505 ) ) ;
#57293 = VECTOR ( 'NONE', #15636, 1000.000000000000114 ) ;
#57294 = EDGE_LOOP ( 'NONE', ( #92710, #74416, #17498, #15024 ) ) ;
#57295 = CARTESIAN_POINT ( 'NONE',  ( -5.265981236333618470E-16, -4.056774720514426669, -4.299999999999999822 ) ) ;
#57296 = EDGE_CURVE ( 'NONE', #90027, #37337, #31170, .T. ) ;
#57297 = CARTESIAN_POINT ( 'NONE',  ( -19.99251892732797486, -11.32171818645973538, 11.49999999999999645 ) ) ;
#57298 = CARTESIAN_POINT ( 'NONE',  ( 22.46337926046256328, 3.617889471270266277, 11.49999999999998934 ) ) ;
#57299 = CARTESIAN_POINT ( 'NONE',  ( -71.18885426527195648, -25.09962176569951708, 7.285300137760615691 ) ) ;
#57300 = VECTOR ( 'NONE', #78824, 1000.000000000000000 ) ;
#57301 = DIRECTION ( 'NONE',  ( -3.773278334453080206E-23, 0.9999999999976377785, 2.173523156925979975E-06 ) ) ;
#57302 = CARTESIAN_POINT ( 'NONE',  ( -90.50599089165145017, -24.52300882791529801, 0.6510814631126391472 ) ) ;
#57303 = CARTESIAN_POINT ( 'NONE',  ( 6.403846153846157740, -5.876774720514425177, 21.48076923076922995 ) ) ;
#57304 = CARTESIAN_POINT ( 'NONE',  ( -69.69184276925987831, -25.16776650702847817, 6.893752584519336146 ) ) ;
#57305 = EDGE_CURVE ( 'NONE', #52175, #22769, #7574, .T. ) ;
#57306 = CARTESIAN_POINT ( 'NONE',  ( -16.30586240431254197, 14.59307310709210626, 11.49999999999998934 ) ) ;
#57307 = CARTESIAN_POINT ( 'NONE',  ( -69.62363805984224996, -24.66019654487199375, 8.947790411086119278 ) ) ;
#57308 = CARTESIAN_POINT ( 'NONE',  ( -115.6228709571500701, -24.83602698348160942, 1.605859176311268621 ) ) ;
#57309 = DIRECTION ( 'NONE',  ( 0.09824042138329625029, 2.980407940728111021E-17, -0.9951627101165079203 ) ) ;
#57310 = CARTESIAN_POINT ( 'NONE',  ( -58.49789633566423674, -24.34968618360933945, 0.1864209137778795045 ) ) ;
#57311 = ORIENTED_EDGE ( 'NONE', *, *, #25063, .F. ) ;
#57312 = CARTESIAN_POINT ( 'NONE',  ( -10.01004151551622456, -17.79114453763541093, -1.500000000000002220 ) ) ;
#57313 = ORIENTED_EDGE ( 'NONE', *, *, #26561, .F. ) ;
#57314 = ORIENTED_EDGE ( 'NONE', *, *, #75667, .T. ) ;
#57315 = CARTESIAN_POINT ( 'NONE',  ( -19.18584950847915493, -12.73052202388904952, -1.500000000000002220 ) ) ;
#57316 = CARTESIAN_POINT ( 'NONE',  ( -95.62287095715005592, -29.50249982740957577, 7.747779886224967605 ) ) ;
#57317 = CIRCLE ( 'NONE', #39477, 6.594667762285751245 ) ;
#57318 = EDGE_LOOP ( 'NONE', ( #49077, #45538, #47812, #93081 ) ) ;
#57319 = CARTESIAN_POINT ( 'NONE',  ( -43.62287095715004881, -29.50248528299804818, 1.056150453629031594 ) ) ;
#57320 = CARTESIAN_POINT ( 'NONE',  ( -101.1944152955115044, -25.16311295231453826, 6.858246048749960799 ) ) ;
#57321 = VECTOR ( 'NONE', #86085, 1000.000000000000114 ) ;
#57322 = FACE_OUTER_BOUND ( 'NONE', #91688, .T. ) ;
#57323 = CARTESIAN_POINT ( 'NONE',  ( -53.58245071975559881, -24.51419770103157347, 9.386484678747180510 ) ) ;
#57325 = EDGE_LOOP ( 'NONE', ( #74093, #58670, #7776, #94865 ) ) ;
#57324 = CARTESIAN_POINT ( 'NONE',  ( 21.20698605602738951, -2.876969938318672870, 11.49999999999999645 ) ) ;
#57326 = ORIENTED_EDGE ( 'NONE', *, *, #78074, .F. ) ;
#57327 = CARTESIAN_POINT ( 'NONE',  ( -9.187330254778467875, -20.22999604658808082, -1.500000000000002220 ) ) ;
#57328 = CARTESIAN_POINT ( 'NONE',  ( 4.906390264955167169, 20.09725327650800608, -1.500000000000002220 ) ) ;
#57330 = ORIENTED_EDGE ( 'NONE', *, *, #52113, .F. ) ;
#57329 = VECTOR ( 'NONE', #30898, 1000.000000000000000 ) ;
#57331 = CARTESIAN_POINT ( 'NONE',  ( -6.728471858368818559, -6.376774720514408301, 19.14926908420045137 ) ) ;
#57332 = LINE ( 'NONE', #2531, #82651 ) ;
#57333 = ORIENTED_EDGE ( 'NONE', *, *, #7154, .F. ) ;
#57334 = CARTESIAN_POINT ( 'NONE',  ( 6.026637739148365548E-17, -29.50247984919009170, -1.443849575687677245 ) ) ;
#57335 = VERTEX_POINT ( 'NONE', #12271 ) ;
#57336 = AXIS2_PLACEMENT_3D ( 'NONE', #27024, #4190, #65611 ) ;
#57337 = CARTESIAN_POINT ( 'NONE',  ( 11.80640562518893866, -3.316774720514426011, -27.06722565682295567 ) ) ;
#57338 = CARTESIAN_POINT ( 'NONE',  ( 18.03207908435136986, 10.65457695745678457, -1.500000000000002220 ) ) ;
#57339 = CARTESIAN_POINT ( 'NONE',  ( -14.06357901826416068, -16.81340526219955933, 11.49999999999999645 ) ) ;
#57340 = CARTESIAN_POINT ( 'NONE',  ( 30.09341516180546350, -2.682774720514426559, -11.39311774897855933 ) ) ;
#57341 = CARTESIAN_POINT ( 'NONE',  ( -37.62287095715006302, -23.96127896941632685, -0.6493128931037903673 ) ) ;
#57342 = CARTESIAN_POINT ( 'NONE',  ( 21.68943130245101258, -6.005725296444199834, 11.49999999999998934 ) ) ;
#57343 = CARTESIAN_POINT ( 'NONE',  ( -2.368302597431856782, 20.80102113048726409, 11.49999999999998934 ) ) ;
#57344 = CARTESIAN_POINT ( 'NONE',  ( -26.09708441595108397, -24.97066806087577362, 5.016021429492140804 ) ) ;
#57345 = DIRECTION ( 'NONE',  ( 0.000000000000000000, 0.000000000000000000, 1.000000000000000000 ) ) ;
#57346 = CARTESIAN_POINT ( 'NONE',  ( -88.92287095715003886, -23.47593901973090169, -1.443836447538996870 ) ) ;
#57347 = ORIENTED_EDGE ( 'NONE', *, *, #28566, .F. ) ;
#57348 = ORIENTED_EDGE ( 'NONE', *, *, #74397, .F. ) ;
#57349 = EDGE_LOOP ( 'NONE', ( #55706, #26221, #58404, #13370 ) ) ;
#57350 = CARTESIAN_POINT ( 'NONE',  ( -52.48647243912292026, -24.65952944569304606, 1.056160979905696351 ) ) ;
#57351 = ORIENTED_EDGE ( 'NONE', *, *, #52799, .T. ) ;
#57352 = B_SPLINE_CURVE_WITH_KNOTS ( 'NONE', 3,
 ( #62321, #76512, #99843, #36967, #30351, #77013, #38469, #92743 ),
 .UNSPECIFIED., .F., .F.,
 ( 4, 2, 2, 4 ),
 ( -0.001240355328176662554, -0.0002398155169398004209, 0.0007607242942970617126, 0.002761803916770777523 ),
 .UNSPECIFIED. ) ;
#57353 = CARTESIAN_POINT ( 'NONE',  ( 6.977786103627443559, 20.27319509581574408, -1.500000000000002220 ) ) ;
#57354 = EDGE_LOOP ( 'NONE', ( #73300, #30223, #72907, #40946 ) ) ;
#57355 = CARTESIAN_POINT ( 'NONE',  ( -26.09636659181000695, -24.95932275238217102, 4.940287574183225061 ) ) ;
#57356 = CARTESIAN_POINT ( 'NONE',  ( -8.250207518706217158, 19.40231308534122689, -1.500000000000002220 ) ) ;
#57357 = CARTESIAN_POINT ( 'NONE',  ( 1.259127588940877285, 10.83856991095998801, 0.000000000000000000 ) ) ;
#57358 = EDGE_CURVE ( 'NONE', #84227, #91131, #9432, .T. ) ;
#57359 = CARTESIAN_POINT ( 'NONE',  ( 3.552327343495968570, -6.376774720514427841, 21.81288606793570395 ) ) ;
#57360 = CARTESIAN_POINT ( 'NONE',  ( -43.58953762381671027, -23.47596703998600276, 11.44779298504227505 ) ) ;
#57361 = LINE ( 'NONE', #56860, #53989 ) ;
#57362 = CARTESIAN_POINT ( 'NONE',  ( -109.3917100257398545, -25.30455905624913626, 4.480208735784438900 ) ) ;
#57363 = CARTESIAN_POINT ( 'NONE',  ( -20.57682416348112397, 7.868404785394932155, -1.500000000000002220 ) ) ;
#57364 = VERTEX_POINT ( 'NONE', #58971 ) ;
#57365 = CARTESIAN_POINT ( 'NONE',  ( -65.59219749188024196, -24.40133493613049964, 9.663955038902800609 ) ) ;
#57366 = AXIS2_PLACEMENT_3D ( 'NONE', #62521, #7214, #23424 ) ;
#57367 = EDGE_CURVE ( 'NONE', #33030, #68434, #73606, .T. ) ;
#57368 = DIRECTION ( 'NONE',  ( 0.000000000000000000, 1.000000000000000000, -0.000000000000000000 ) ) ;
#57369 = CARTESIAN_POINT ( 'NONE',  ( -41.36802863981588274, -25.27956007679128803, 5.250400797641334272 ) ) ;
#57370 = EDGE_CURVE ( 'NONE', #61510, #84489, #42753, .T. ) ;
#57371 = FACE_BOUND ( 'NONE', #63560, .T. ) ;
#57372 = AXIS2_PLACEMENT_3D ( 'NONE', #11052, #57739, #42516 ) ;
#57373 = ADVANCED_FACE ( 'NONE', ( #80803 ), #81955, .T. ) ;
#57374 = CARTESIAN_POINT ( 'NONE',  ( -1.044871794871790938, -5.876774720514426953, 21.75000000000000355 ) ) ;
#57375 = DIRECTION ( 'NONE',  ( 0.000000000000000000, 0.000000000000000000, -1.000000000000000000 ) ) ;
#57376 = CARTESIAN_POINT ( 'NONE',  ( -0.3244385709253747585, -21.36021439428519386, 11.49999999999998934 ) ) ;
#57377 = DIRECTION ( 'NONE',  ( -0.9975640502598241977, 0.06975647374412534407, -4.324999876874012340E-16 ) ) ;
#57378 = EDGE_CURVE ( 'NONE', #49156, #14292, #41243, .T. ) ;
#57379 = CARTESIAN_POINT ( 'NONE',  ( -91.62287095715004170, -23.47596703998600631, 11.44779298504227860 ) ) ;
#57380 = CARTESIAN_POINT ( 'NONE',  ( 0.000000000000000000, -6.943225279485572443, -1.149999999999999911 ) ) ;
#57381 = CARTESIAN_POINT ( 'NONE',  ( -81.41755102971610825, -25.21105436082871876, 6.516612835075878962 ) ) ;
#57382 = CARTESIAN_POINT ( 'NONE',  ( -19.71520456405594857, 11.01310763156902972, -1.500000000000002220 ) ) ;
#57383 = CARTESIAN_POINT ( 'NONE',  ( -112.5895376238167245, -23.47593901973091235, -1.443836447538999312 ) ) ;
#57384 = ORIENTED_EDGE ( 'NONE', *, *, #9467, .F. ) ;
#57385 = CARTESIAN_POINT ( 'NONE',  ( 4.639188450898540594, -5.876774720514418959, 20.39229233339611014 ) ) ;
#57386 = CARTESIAN_POINT ( 'NONE',  ( -79.54333787041024095, -24.51314013834316086, 0.6176544820404135105 ) ) ;
#57387 = CARTESIAN_POINT ( 'NONE',  ( 19.69962056004252560, 1.334664424591413434, 11.49999999999999645 ) ) ;
#57388 = CARTESIAN_POINT ( 'NONE',  ( -93.58953762381672448, -23.48786465467241769, 11.44779295918254114 ) ) ;
#57389 = CARTESIAN_POINT ( 'NONE',  ( -67.54913149170559450, -24.15543982623906416, -0.2315651400026651485 ) ) ;
#57390 = EDGE_LOOP ( 'NONE', ( #189, #8247, #8521 ) ) ;
#57391 = CARTESIAN_POINT ( 'NONE',  ( 6.303825520940272042, -5.965225279485572685, -28.39893233836329856 ) ) ;
#57392 = CARTESIAN_POINT ( 'NONE',  ( -39.52287095715006870, -24.65952944569304606, 1.056160979905691910 ) ) ;
#57393 = LINE ( 'NONE', #47763, #79012 ) ;
#57394 = CARTESIAN_POINT ( 'NONE',  ( -20.54952838774410750, 6.582847151591199264, -1.500000000000002220 ) ) ;
#57395 = CARTESIAN_POINT ( 'NONE',  ( -71.55620429048339304, -23.47596703998600276, 11.44779298504227505 ) ) ;
#57396 = DIRECTION ( 'NONE',  ( -0.000000000000000000, -1.000000000000000000, -0.000000000000000000 ) ) ;
#57397 = B_SPLINE_CURVE_WITH_KNOTS ( 'NONE', 3,
 ( #99231, #43965, #98233, #91621, #12509, #28237 ),
 .UNSPECIFIED., .F., .F.,
 ( 4, 2, 4 ),
 ( 0.000000000000000000, 0.001381645795574012190, 0.002763291591148024379 ),
 .UNSPECIFIED. ) ;
#57398 = CARTESIAN_POINT ( 'NONE',  ( -78.52287095715006160, -24.64898659630367916, 1.056161002820826145 ) ) ;
#57399 = DIRECTION ( 'NONE',  ( -3.773278334453079030E-23, 0.9999999999976377785, 2.173523156925979128E-06 ) ) ;
#57400 = CARTESIAN_POINT ( 'NONE',  ( -7.851535696030730982, 18.15458241006858131, -1.500000000000002220 ) ) ;
#57401 = ORIENTED_EDGE ( 'NONE', *, *, #36633, .T. ) ;
#57402 = CARTESIAN_POINT ( 'NONE',  ( -19.72078065558051208, -4.686549088087978099, 11.49999999999999645 ) ) ;
#57403 = CARTESIAN_POINT ( 'NONE',  ( -7.567681410454951241, -5.876774720514412742, 19.71630089903357330 ) ) ;
#57404 = ORIENTED_EDGE ( 'NONE', *, *, #29102, .T. ) ;
#57405 = CARTESIAN_POINT ( 'NONE',  ( -65.62287095715005592, -23.47596703998600631, 11.44779298504227683 ) ) ;
#57406 = CARTESIAN_POINT ( 'NONE',  ( -99.72678786515000127, -25.29364544523226854, 4.454263737081315178 ) ) ;
#57407 = FACE_BOUND ( 'NONE', #69395, .T. ) ;
#57408 = CARTESIAN_POINT ( 'NONE',  ( -59.62287095715004881, -24.66019654487199020, 8.947790411086131712 ) ) ;
#57409 = DIRECTION ( 'NONE',  ( -3.773278334444167608E-23, 1.000000000000000000, 0.000000000000000000 ) ) ;
#57410 = CARTESIAN_POINT ( 'NONE',  ( -32.99388727629348494, -25.11010231571544082, 2.831122766524410750 ) ) ;
#57411 = CARTESIAN_POINT ( 'NONE',  ( -4.446071851354966853, 19.53225066162704948, 11.49999999999998934 ) ) ;
#57412 = CARTESIAN_POINT ( 'NONE',  ( 27.86270917940689174, -5.965225279485572685, 29.49402280011862487 ) ) ;
#57413 = ORIENTED_EDGE ( 'NONE', *, *, #78971, .F. ) ;
#57414 = CARTESIAN_POINT ( 'NONE',  ( -32.62287095715005592, -24.51387760970722240, 9.387446482453418284 ) ) ;
#57415 = DIRECTION ( 'NONE',  ( 0.000000000000000000, -2.173523156925979552E-06, 0.9999999999976378895 ) ) ;
#57416 = CARTESIAN_POINT ( 'NONE',  ( -92.62287095715007013, -23.72773821059536559, 11.05748984161097681 ) ) ;
#57417 = CARTESIAN_POINT ( 'NONE',  ( -119.6228709571500559, -29.50248528299804818, 1.056150453629045360 ) ) ;
#57419 = EDGE_CURVE ( 'NONE', #53428, #79759, #28999, .T. ) ;
#57418 = DIRECTION ( 'NONE',  ( -0.2164396139380966033, 0.9762960071199348056, -0.000000000000000000 ) ) ;
#57420 = AXIS2_PLACEMENT_3D ( 'NONE', #53271, #16191, #76580 ) ;
#57421 = PLANE ( 'NONE',  #33269 ) ;
#57422 = ADVANCED_FACE ( 'NONE', ( #14762 ), #82786, .T. ) ;
#57423 = CARTESIAN_POINT ( 'NONE',  ( -100.9368031010810398, -25.32724633150699844, 4.398074151685130495 ) ) ;
#57424 = ORIENTED_EDGE ( 'NONE', *, *, #6284, .F. ) ;
#57425 = CARTESIAN_POINT ( 'NONE',  ( -16.58479117878708209, 11.75282063728064053, 11.49999999999998934 ) ) ;
#57426 = VERTEX_POINT ( 'NONE', #45730 ) ;
#57427 = CARTESIAN_POINT ( 'NONE',  ( -14.16064136294604303, -18.02537036913223290, 11.49999999999998934 ) ) ;
#57428 = CARTESIAN_POINT ( 'NONE',  ( -32.66837636242299681, -23.48783264082477729, -1.443836473390076147 ) ) ;
#57429 = VECTOR ( 'NONE', #64936, 1000.000000000000000 ) ;
#57430 = CARTESIAN_POINT ( 'NONE',  ( -122.5228709571500616, -24.65952944569305316, 1.056160979905705899 ) ) ;
#57431 = ORIENTED_EDGE ( 'NONE', *, *, #76576, .T. ) ;
#57432 = DIRECTION ( 'NONE',  ( 0.000000000000000000, 0.9999999999976377785, 2.173523156925979128E-06 ) ) ;
#57433 = CARTESIAN_POINT ( 'NONE',  ( 14.83533542161589480, 3.438288638725202517, -27.37882296607460120 ) ) ;
#57434 = CARTESIAN_POINT ( 'NONE',  ( -30.47287095715007155, -25.30769195857878984, 4.725583353285079724 ) ) ;
#57435 = CARTESIAN_POINT ( 'NONE',  ( -0.1268723920767304558, 21.18662008908366445, 11.49999999999999645 ) ) ;
#57436 = CARTESIAN_POINT ( 'NONE',  ( 18.07010470096111021, 12.80550835427630574, 11.49999999999998934 ) ) ;
#57437 = B_SPLINE_CURVE_WITH_KNOTS ( 'NONE', 3,
 ( #78251, #40212, #8764, #70662, #40712, #32089 ),
 .UNSPECIFIED., .F., .F.,
 ( 4, 2, 4 ),
 ( 0.000000000000000000, 0.001380901958385391580, 0.002761803916770783161 ),
 .UNSPECIFIED. ) ;
#57439 = CARTESIAN_POINT ( 'NONE',  ( -1.637206367458305500, 20.51943892441452633, -1.500000000000002220 ) ) ;
#57438 = CC_DESIGN_PERSON_AND_ORGANIZATION_ASSIGNMENT ( #94181, #24666, ( #66951 ) ) ;
#57440 = ORIENTED_EDGE ( 'NONE', *, *, #1627, .T. ) ;
#57441 = CARTESIAN_POINT ( 'NONE',  ( -41.51336541085899512, -23.73766607897670866, -1.055555164236442023 ) ) ;
#57442 = VERTEX_POINT ( 'NONE', #6162 ) ;
#57443 = CARTESIAN_POINT ( 'NONE',  ( -54.53713584333244313, -24.51314013834315020, 0.6176544820404069602 ) ) ;
#57444 = CARTESIAN_POINT ( 'NONE',  ( -49.62287095715006302, -23.94994826722515313, -0.6494450866351706431 ) ) ;
#57445 = ORIENTED_EDGE ( 'NONE', *, *, #24621, .T. ) ;
#57446 = VERTEX_POINT ( 'NONE', #20881 ) ;
#57447 = EDGE_LOOP ( 'NONE', ( #78987, #65215, #39460, #56967 ) ) ;
#57448 = DIRECTION ( 'NONE',  ( 0.9822594791677485837, 0.000000000000000000, -0.1875268396392987258 ) ) ;
#57449 = CARTESIAN_POINT ( 'NONE',  ( -28.52988911114128356, -24.35371376620799211, 9.386484685950517104 ) ) ;
#57450 = CARTESIAN_POINT ( 'NONE',  ( -102.5228709571500758, -29.50248528299804818, 1.056150453629042030 ) ) ;
#57451 = CARTESIAN_POINT ( 'NONE',  ( -7.464567774302189207, 19.34240081622845153, -1.500000000000002220 ) ) ;
#57452 = CARTESIAN_POINT ( 'NONE',  ( -15.31764660673900558, 15.41647822393392175, 11.49999999999999645 ) ) ;
#57453 = ORIENTED_EDGE ( 'NONE', *, *, #83019, .F. ) ;
#57454 = DIRECTION ( 'NONE',  ( 1.000000000000000000, -7.960204194457801640E-17, 0.000000000000000000 ) ) ;
#57455 = CARTESIAN_POINT ( 'NONE',  ( 2.650685085285006348, -5.876774720514410077, 19.28073557658628445 ) ) ;
#57456 = CARTESIAN_POINT ( 'NONE',  ( -14.11974515630795501, -17.41659395067913962, 11.49999999999998934 ) ) ;
#57457 = CARTESIAN_POINT ( 'NONE',  ( -92.92287095715002465, -23.47593901973090169, -1.443836447538996870 ) ) ;
#57458 = LINE ( 'NONE', #81271, #64308 ) ;
#57459 = EDGE_LOOP ( 'NONE', ( #74804, #99407, #2160, #31701 ) ) ;
#57460 = DIRECTION ( 'NONE',  ( 0.000000000000000000, 0.000000000000000000, -1.000000000000000000 ) ) ;
#57461 = CARTESIAN_POINT ( 'NONE',  ( -116.4728709548940628, -25.40673988423725405, 2.000950542041673774 ) ) ;
#57462 = AXIS2_PLACEMENT_3D ( 'NONE', #31140, #61619, #22513 ) ;
#57463 = ORIENTED_EDGE ( 'NONE', *, *, #40039, .T. ) ;
#57464 = B_SPLINE_CURVE_WITH_KNOTS ( 'NONE', 3,
 ( #90354, #68517, #29949, #46182, #45684, #14717 ),
 .UNSPECIFIED., .F., .F.,
 ( 4, 2, 4 ),
 ( 6.391158118972359742E-06, 0.001387004593080791133, 0.002767618028042609802 ),
 .UNSPECIFIED. ) ;
#57465 = ORIENTED_EDGE ( 'NONE', *, *, #83784, .F. ) ;
#57466 = CARTESIAN_POINT ( 'NONE',  ( -103.6228709571500417, -24.50216790748100237, 0.6166512839513710320 ) ) ;
#57467 = ORIENTED_EDGE ( 'NONE', *, *, #12419, .T. ) ;
#57468 = CARTESIAN_POINT ( 'NONE',  ( -6.410030533929251817, 20.24415959294862333, -1.500000000000002220 ) ) ;
#57469 = B_SPLINE_CURVE_WITH_KNOTS ( 'NONE', 3,
 ( #84397, #83897, #83394, #61078, #39216, #6768 ),
 .UNSPECIFIED., .F., .F.,
 ( 4, 2, 4 ),
 ( 0.000000000000000000, 0.001380764517854760629, 0.002761529035709521258 ),
 .UNSPECIFIED. ) ;
#57470 = ORIENTED_EDGE ( 'NONE', *, *, #30882, .T. ) ;
#57471 = CARTESIAN_POINT ( 'NONE',  ( -88.59843814960578356, -23.73766607897670511, -1.055555164236456678 ) ) ;
#57472 = CARTESIAN_POINT ( 'NONE',  ( 19.92038474643397805, 8.973206291307779026, 11.49999999999998934 ) ) ;
#57473 = CARTESIAN_POINT ( 'NONE',  ( -52.60591462248186190, -23.73791477778911840, 11.05961554403171299 ) ) ;
#57474 = LINE ( 'NONE', #50349, #79320 ) ;
#57475 = DIRECTION ( 'NONE',  ( -3.773278334444166432E-23, 1.000000000000000000, 0.000000000000000000 ) ) ;
#57476 = CARTESIAN_POINT ( 'NONE',  ( 12.58402814888991372, -17.87355554032721372, -1.500000000000002220 ) ) ;
#57477 = DIRECTION ( 'NONE',  ( -0.000000000000000000, 1.000000000000000000, -0.000000000000000000 ) ) ;
#57478 = ORIENTED_EDGE ( 'NONE', *, *, #26231, .F. ) ;
#57479 = CARTESIAN_POINT ( 'NONE',  ( 25.07255740347941853, 5.130262834649095716, -9.008209484467815997 ) ) ;
#57480 = CARTESIAN_POINT ( 'NONE',  ( -20.27875734969026311, 3.456774720514426136, 25.15402280011862146 ) ) ;
#57481 = ORIENTED_EDGE ( 'NONE', *, *, #79229, .T. ) ;
#57482 = CARTESIAN_POINT ( 'NONE',  ( -30.64752034897746924, -23.47593901973090169, -1.443836447538997758 ) ) ;
#57483 = VERTEX_POINT ( 'NONE', #43741 ) ;
#57484 = EDGE_CURVE ( 'NONE', #81901, #87248, #67497, .T. ) ;
#57485 = CARTESIAN_POINT ( 'NONE',  ( -40.02662638259540273, -25.26390949617024262, 6.217221587706935892 ) ) ;
#57486 = DIRECTION ( 'NONE',  ( 4.089440751051245812E-15, -1.000000000000000000, -1.042451643221144600E-15 ) ) ;
#57487 = CARTESIAN_POINT ( 'NONE',  ( -12.22836702412972087, 17.35733969022439993, -1.500000000000002220 ) ) ;
#57488 = CARTESIAN_POINT ( 'NONE',  ( -37.62287095715005592, -29.50250243563736774, 8.947779886222148704 ) ) ;
#57489 = ADVANCED_FACE ( 'NONE', ( #28504 ), #83932, .T. ) ;
#57490 = DIRECTION ( 'NONE',  ( 0.000000000000000000, 0.000000000000000000, -1.000000000000000000 ) ) ;
#57491 = AXIS2_PLACEMENT_3D ( 'NONE', #47285, #61516, #92438 ) ;
#57492 = DIRECTION ( 'NONE',  ( -0.000000000000000000, 1.000000000000000000, -0.000000000000000000 ) ) ;
#57493 = CARTESIAN_POINT ( 'NONE',  ( -68.60861524139340872, -23.48783264082476308, -1.443836473390094799 ) ) ;
#57494 = CARTESIAN_POINT ( 'NONE',  ( -17.77321681866180469, -7.816401696202086136, 11.49999999999998934 ) ) ;
#57495 = DIRECTION ( 'NONE',  ( -3.773278334453079030E-23, 0.9999999999976377785, 2.173523156925979128E-06 ) ) ;
#57496 = ORIENTED_EDGE ( 'NONE', *, *, #9386, .F. ) ;
#57497 = CARTESIAN_POINT ( 'NONE',  ( 13.97609912898263573, 13.72534901313461653, 11.49999999999999645 ) ) ;
#57498 = CARTESIAN_POINT ( 'NONE',  ( 31.61406883670153789, -4.508386143373845023, 26.44289287685778334 ) ) ;
#57499 = CARTESIAN_POINT ( 'NONE',  ( -97.52287095715006160, -23.48786465467241769, 11.44779295918254114 ) ) ;
#57500 = EDGE_CURVE ( 'NONE', #83990, #85754, #39623, .T. ) ;
#57501 = ORIENTED_EDGE ( 'NONE', *, *, #86875, .T. ) ;
#57502 = VECTOR ( 'NONE', #82635, 1000.000000000000000 ) ;
#57503 = CARTESIAN_POINT ( 'NONE',  ( -97.62287095715008434, -24.50216790748100237, 0.6166512839513762501 ) ) ;
#57504 = CARTESIAN_POINT ( 'NONE',  ( -75.62287095715004170, -24.83602698348158810, 1.605859176311266179 ) ) ;
#57505 = DIRECTION ( 'NONE',  ( 0.000000000000000000, 0.000000000000000000, 1.000000000000000000 ) ) ;
#57506 = DIRECTION ( 'NONE',  ( 0.000000000000000000, -0.000000000000000000, -1.000000000000000000 ) ) ;
#57507 = CARTESIAN_POINT ( 'NONE',  ( 8.085132396474181249, 17.94908993440701295, 11.49999999999998934 ) ) ;
#57508 = B_SPLINE_CURVE_WITH_KNOTS ( 'NONE', 3,
 ( #49622, #11536, #11047, #72954 ),
 .UNSPECIFIED., .F., .F.,
 ( 4, 4 ),
 ( 0.000000000000000000, 1.000000000000000000 ),
 .UNSPECIFIED. ) ;
#57509 = EDGE_LOOP ( 'NONE', ( #52172, #39964, #48671, #86118 ) ) ;
#57510 = FACE_OUTER_BOUND ( 'NONE', #63029, .T. ) ;
#57511 = PLANE ( 'NONE',  #43145 ) ;
#57512 = APPLICATION_PROTOCOL_DEFINITION ( 'international standard', 'config_control_design', 1994, #4487 ) ;
#57513 = VERTEX_POINT ( 'NONE', #76161 ) ;
#57514 = CARTESIAN_POINT ( 'NONE',  ( 3.362030615038681169, -5.876774720514423400, 21.34376340489846413 ) ) ;
#57515 = CARTESIAN_POINT ( 'NONE',  ( -1.501937386944296460, -6.376774720514415407, 19.86422795159478483 ) ) ;
#57516 = LINE ( 'NONE', #65635, #5358 ) ;
#57517 = CARTESIAN_POINT ( 'NONE',  ( -29.52287095715006160, -24.56627961951908645, 8.947790480023282811 ) ) ;
#57518 = LINE ( 'NONE', #18926, #33727 ) ;
#57519 = DIRECTION ( 'NONE',  ( 0.000000000000000000, 0.000000000000000000, -1.000000000000000000 ) ) ;
#57520 = FACE_OUTER_BOUND ( 'NONE', #45575, .T. ) ;
#57521 = CARTESIAN_POINT ( 'NONE',  ( 14.81759351585047391, 13.34335055255382052, 11.49999999999998934 ) ) ;
#57522 = CARTESIAN_POINT ( 'NONE',  ( -100.6434263600250745, -25.19749065189113679, 3.311375407965762463 ) ) ;
#57523 = CARTESIAN_POINT ( 'NONE',  ( -6.239078800006583769, 18.87631364486404806, -1.500000000000002220 ) ) ;
#57524 = VERTEX_POINT ( 'NONE', #6659 ) ;
#57525 = CARTESIAN_POINT ( 'NONE',  ( -29.52287095715006160, -24.56560739788454129, 1.056161319240904728 ) ) ;
#57526 = EDGE_CURVE ( 'NONE', #61907, #32410, #38107, .T. ) ;
#57527 = LINE ( 'NONE', #57027, #7902 ) ;
#57528 = DIRECTION ( 'NONE',  ( 0.000000000000000000, 1.408054769461693696E-16, -1.000000000000000000 ) ) ;
#57529 = CIRCLE ( 'NONE', #99636, 252.4458649670781085 ) ;
#57530 = CARTESIAN_POINT ( 'NONE',  ( 12.30588647389939538, -3.316774720514762187, -28.11066263608955751 ) ) ;
#57531 = CARTESIAN_POINT ( 'NONE',  ( 17.18838054715250152, -11.71887806637979779, 11.49999999999999645 ) ) ;
#57532 = CARTESIAN_POINT ( 'NONE',  ( -7.567681410454951241, -5.876774720514411854, 19.71630089903357330 ) ) ;
#57533 = ADVANCED_FACE ( 'NONE', ( #61467 ), #43613, .T. ) ;
#57534 = CARTESIAN_POINT ( 'NONE',  ( -50.91254006769597140, -25.20043120925951996, 3.405783117403155646 ) ) ;
#57535 = B_SPLINE_CURVE_WITH_KNOTS ( 'NONE', 3,
 ( #36730, #12876, #3799, #81907, #49981 ),
 .UNSPECIFIED., .F., .F.,
 ( 4, 1, 4 ),
 ( 0.000000000000000000, 0.5126593363417801807, 0.9999999999999998890 ),
 .UNSPECIFIED. ) ;
#57536 = CARTESIAN_POINT ( 'NONE',  ( 18.61037501828884189, -13.27421459584354579, 11.49999999999999645 ) ) ;
#57537 = EDGE_LOOP ( 'NONE', ( #90753, #27716, #72716, #62709 ) ) ;
#57538 = CARTESIAN_POINT ( 'NONE',  ( -0.02075734969026423599, -6.376774720514426953, -29.05397719988137339 ) ) ;
#57539 = DIRECTION ( 'NONE',  ( 0.000000000000000000, -0.9999999999976377785, -2.173523156925979975E-06 ) ) ;
#57540 = VERTEX_POINT ( 'NONE', #19752 ) ;
#57541 = CARTESIAN_POINT ( 'NONE',  ( 16.63042848490962555, -11.55671354112608817, -1.500000000000002220 ) ) ;
#57542 = CARTESIAN_POINT ( 'NONE',  ( 6.955725288069978696, -5.876774720514426065, 21.70430095680336890 ) ) ;
#57543 = DIRECTION ( 'NONE',  ( 0.000000000000000000, 0.9999999999976377785, 2.173523156925979128E-06 ) ) ;
#57544 = DIRECTION ( 'NONE',  ( -0.000000000000000000, 1.000000000000000000, -0.000000000000000000 ) ) ;
#57545 = ORIENTED_EDGE ( 'NONE', *, *, #98444, .F. ) ;
#57546 = CARTESIAN_POINT ( 'NONE',  ( -109.5228709571500616, -24.64965694238408034, 8.947790433994192938 ) ) ;
#57547 = CARTESIAN_POINT ( 'NONE',  ( -30.53953689462962018, -23.47596701192223989, 11.43488133310209420 ) ) ;
#57548 = CARTESIAN_POINT ( 'NONE',  ( -10.28607412905329532, -17.16720287211733975, -1.500000000000002220 ) ) ;
#57549 = CARTESIAN_POINT ( 'NONE',  ( -9.798014431990228701, 18.61115389415964572, 11.49999999999999645 ) ) ;
#57550 = CARTESIAN_POINT ( 'NONE',  ( -41.32836283488544638, 4.132774720514426292, 39.26872235229541985 ) ) ;
#57551 = FACE_OUTER_BOUND ( 'NONE', #94363, .T. ) ;
#57552 = CARTESIAN_POINT ( 'NONE',  ( 22.04941498731238525, 0.3350016526185666255, -1.500000000000002220 ) ) ;
#57553 = AXIS2_PLACEMENT_3D ( 'NONE', #19699, #44051, #20699 ) ;
#57554 = EDGE_CURVE ( 'NONE', #48655, #30953, #36535, .T. ) ;
#57555 = PRODUCT_DEFINITION ( 'UNKNOWN', '', #21418, #45906 ) ;
#57556 = CARTESIAN_POINT ( 'NONE',  ( 10.44337217408228291, 4.530443463488840194, -26.67771320976549987 ) ) ;
#57557 = DIRECTION ( 'NONE',  ( 0.000000000000000000, 0.000000000000000000, -1.000000000000000000 ) ) ;
#57558 = CARTESIAN_POINT ( 'NONE',  ( -28.98875734969026396, 0.3587747205144265483, 2.362022800118626531 ) ) ;
#57559 = CARTESIAN_POINT ( 'NONE',  ( -72.55911174566438149, -23.73766607897670156, -1.055555164236458454 ) ) ;
#57560 = CARTESIAN_POINT ( 'NONE',  ( -31.49625347033022749, -24.15543982623907127, -0.2315651400026576545 ) ) ;
#57561 = ORIENTED_EDGE ( 'NONE', *, *, #87635, .F. ) ;
#57562 = ORIENTED_EDGE ( 'NONE', *, *, #52888, .F. ) ;
#57563 = DIRECTION ( 'NONE',  ( -1.000000000000000000, 0.000000000000000000, 0.000000000000000000 ) ) ;
#57564 = CARTESIAN_POINT ( 'NONE',  ( -100.4381051993576506, -25.27404630390602236, 2.832404461470396928 ) ) ;
#57565 = CARTESIAN_POINT ( 'NONE',  ( -40.45829750704998418, -29.50249014687182836, 3.293933732389337621 ) ) ;
#57566 = CARTESIAN_POINT ( 'NONE',  ( 19.76637988705548210, 5.604140092158477415, -1.500000000000002220 ) ) ;
#57567 = VECTOR ( 'NONE', #90637, 1000.000000000000000 ) ;
#57568 = VERTEX_POINT ( 'NONE', #35506 ) ;
#57569 = CARTESIAN_POINT ( 'NONE',  ( -99.62287095715005592, -29.50247984919015209, -1.443849546365050029 ) ) ;
#57570 = EDGE_CURVE ( 'NONE', #54376, #69295, #23548, .T. ) ;
#57571 = DIRECTION ( 'NONE',  ( 1.000000000000000000, -0.000000000000000000, -0.000000000000000000 ) ) ;
#57572 = CARTESIAN_POINT ( 'NONE',  ( -2.768609665556983845, -5.965225279485594001, -29.41086200512614823 ) ) ;
#57573 = CARTESIAN_POINT ( 'NONE',  ( -22.12323335113916301, -3.008119206214963981, 11.49999999999998934 ) ) ;
#57574 = CIRCLE ( 'NONE', #83468, 2.000000000000001776 ) ;
#57575 = DIRECTION ( 'NONE',  ( 0.000000000000000000, -1.000000000000000000, 0.000000000000000000 ) ) ;
#57576 = CARTESIAN_POINT ( 'NONE',  ( 13.91401389203221406, -6.376774720514426953, 27.24920385068457662 ) ) ;
#57577 = VERTEX_POINT ( 'NONE', #10664 ) ;
#57578 = DIRECTION ( 'NONE',  ( -0.000000000000000000, -1.000000000000000000, 0.000000000000000000 ) ) ;
#57579 = CARTESIAN_POINT ( 'NONE',  ( 3.128267882468583228, -5.876774720514423400, 21.08409277973916218 ) ) ;
#57580 = CARTESIAN_POINT ( 'NONE',  ( 16.20321855003292555, -13.12800272717607619, 11.49999999999998934 ) ) ;
#57581 = VERTEX_POINT ( 'NONE', #28374 ) ;
#57583 = ORIENTED_EDGE ( 'NONE', *, *, #78006, .F. ) ;
#57582 = CARTESIAN_POINT ( 'NONE',  ( 0.4325450954222598288, 0.000000000000000000, 2.350000000000000089 ) ) ;
#57584 = VERTEX_POINT ( 'NONE', #66963 ) ;
#57585 = CARTESIAN_POINT ( 'NONE',  ( -69.97463645619113493, -25.25935341538093581, 7.520861282928617442 ) ) ;
#57586 = CARTESIAN_POINT ( 'NONE',  ( -17.90976863334866920, 11.11529090135583075, -1.500000000000002220 ) ) ;
#57587 = ORIENTED_EDGE ( 'NONE', *, *, #15520, .F. ) ;
#57588 = CARTESIAN_POINT ( 'NONE',  ( -114.6228709571500701, -23.95044443724992789, 10.65354141964649237 ) ) ;
#57589 = CARTESIAN_POINT ( 'NONE',  ( -102.6228709571500133, -24.33927499327854704, 9.819080762295815390 ) ) ;
#57590 = LINE ( 'NONE', #3800, #87019 ) ;
#57591 = CARTESIAN_POINT ( 'NONE',  ( -101.9507253916653440, -25.03152160760679479, 6.236251142457633456 ) ) ;
#57592 = CARTESIAN_POINT ( 'NONE',  ( -129.6228709571500701, -23.72773821059536559, 11.05748984161097503 ) ) ;
#57593 = CARTESIAN_POINT ( 'NONE',  ( -14.16021466491576675, 16.42052772630311352, -1.500000000000002220 ) ) ;
#57594 = CARTESIAN_POINT ( 'NONE',  ( -63.52287095715003318, -24.35013146730202749, 9.818937971375104823 ) ) ;
#57595 = EDGE_CURVE ( 'NONE', #73714, #80473, #71087, .T. ) ;
#57597 = EDGE_LOOP ( 'NONE', ( #77881, #30883, #22318, #55840 ) ) ;
#57596 = CARTESIAN_POINT ( 'NONE',  ( 22.02009960291501045, 3.200778107580485532, 11.49999999999999645 ) ) ;
#57598 = CARTESIAN_POINT ( 'NONE',  ( -72.62287095715005592, -24.66019654487199020, 8.947790411086131712 ) ) ;
#57599 = DIRECTION ( 'NONE',  ( 0.000000000000000000, 0.000000000000000000, -1.000000000000000000 ) ) ;
#57600 = CARTESIAN_POINT ( 'NONE',  ( -87.52287095715006160, -24.65952944569304606, 1.056160979905700570 ) ) ;
#57601 = ORIENTED_EDGE ( 'NONE', *, *, #43090, .T. ) ;
#57603 = VERTEX_POINT ( 'NONE', #72568 ) ;
#57602 = CARTESIAN_POINT ( 'NONE',  ( -41.52287095715005449, -24.66019654487198665, 8.947790411086121054 ) ) ;
#57604 = ORIENTED_EDGE ( 'NONE', *, *, #14668, .F. ) ;
#57605 = VECTOR ( 'NONE', #6088, 1000.000000000000000 ) ;
#57606 = CARTESIAN_POINT ( 'NONE',  ( -57.58953762381672448, -23.47596703998600276, 11.44779298504227505 ) ) ;
#57607 = EDGE_CURVE ( 'NONE', #53312, #10530, #81169, .T. ) ;
#57608 = CARTESIAN_POINT ( 'NONE',  ( -48.62287095715004881, -23.48783264082478439, -1.443836473390070596 ) ) ;
#57609 = LINE ( 'NONE', #87544, #23037 ) ;
#57610 = VERTEX_POINT ( 'NONE', #89785 ) ;
#57611 = B_SPLINE_CURVE_WITH_KNOTS ( 'NONE', 3,
 ( #91770, #92772, #8549, #39503 ),
 .UNSPECIFIED., .F., .F.,
 ( 4, 4 ),
 ( 0.5191410469121615634, 0.5201417939529271450 ),
 .UNSPECIFIED. ) ;
#57612 = DIRECTION ( 'NONE',  ( 0.000000000000000000, -1.000000000000000000, 0.000000000000000000 ) ) ;
#57613 = CARTESIAN_POINT ( 'NONE',  ( 18.78116726530667080, 12.29669497462397842, -1.500000000000002220 ) ) ;
#57614 = EDGE_CURVE ( 'NONE', #63282, #67539, #19141, .T. ) ;
#57615 = VERTEX_POINT ( 'NONE', #82166 ) ;
#57616 = DIRECTION ( 'NONE',  ( -3.773278334453080206E-23, 0.9999999999976377785, 2.173523156925979975E-06 ) ) ;
#57617 = PLANE ( 'NONE',  #49147 ) ;
#57618 = CARTESIAN_POINT ( 'NONE',  ( 7.227401621481964966, 5.356774720515138810, -27.22638491171618824 ) ) ;
#57619 = CARTESIAN_POINT ( 'NONE',  ( -41.52287095715004739, -24.34917612407030063, 0.1852690917476942645 ) ) ;
#57620 = CARTESIAN_POINT ( 'NONE',  ( -97.24791218068880028, -24.66513809378596989, 8.909134979017300893 ) ) ;
#57621 = CARTESIAN_POINT ( 'NONE',  ( 17.47348308817029405, 8.859467055162037141, 11.49999999999998934 ) ) ;
#57622 = DIRECTION ( 'NONE',  ( -0.000000000000000000, -1.000000000000000000, -0.000000000000000000 ) ) ;
#57623 = VERTEX_POINT ( 'NONE', #74555 ) ;
#57624 = CARTESIAN_POINT ( 'NONE',  ( -21.26083644630951142, -3.357327265692296780, -1.500000000000002220 ) ) ;
#57625 = CARTESIAN_POINT ( 'NONE',  ( 5.395440699609681090, -0.3587747205144061202, -28.51842087987364849 ) ) ;
#57626 = CARTESIAN_POINT ( 'NONE',  ( -70.94546041667526026, -25.12219101425611356, 6.902322780480511177 ) ) ;
#57627 = CARTESIAN_POINT ( 'NONE',  ( -53.55620429048339304, -23.47596703998600276, 11.44779298504227505 ) ) ;
#57628 = DIRECTION ( 'NONE',  ( -3.773278334453080206E-23, 0.9999999999976377785, 2.173523156925979975E-06 ) ) ;
#57629 = CARTESIAN_POINT ( 'NONE',  ( -22.40196285382242536, -4.882868457752029379, -1.500000000000002220 ) ) ;
#57630 = AXIS2_PLACEMENT_3D ( 'NONE', #40314, #71264, #1755 ) ;
#57631 = DATE_AND_TIME ( #78938, #3500 ) ;
#57632 = FACE_OUTER_BOUND ( 'NONE', #17146, .T. ) ;
#57633 = CARTESIAN_POINT ( 'NONE',  ( -53.54178288312186140, -24.34968618360933590, 0.1864209137778785885 ) ) ;
#57634 = CARTESIAN_POINT ( 'NONE',  ( -19.74138705131307248, -3.616033589355840849, 11.49999999999999645 ) ) ;
#57635 = DIRECTION ( 'NONE',  ( 0.000000000000000000, -0.9999999999976377785, -2.173523156925979975E-06 ) ) ;
#57636 = CARTESIAN_POINT ( 'NONE',  ( 13.91401389203221406, 0.3587747205144265483, 158.0376437107427137 ) ) ;
#57638 = CARTESIAN_POINT ( 'NONE',  ( -121.6228709571500559, -23.47596703998600631, 11.44779298504227683 ) ) ;
#57637 = AXIS2_PLACEMENT_3D ( 'NONE', #47864, #94524, #17405 ) ;
#57639 = DIRECTION ( 'NONE',  ( 1.000000000000000000, 3.773278334444166432E-23, 8.201307841325785021E-29 ) ) ;
#57640 = CARTESIAN_POINT ( 'NONE',  ( 7.150000000000004796, -2.000000000000001776, 18.24068255301867936 ) ) ;
#57641 = CARTESIAN_POINT ( 'NONE',  ( -19.55781625546462976, 3.520333346782119843, 11.49999999999998934 ) ) ;
#57642 = AXIS2_PLACEMENT_3D ( 'NONE', #98264, #89674, #20150 ) ;
#57643 = DIRECTION ( 'NONE',  ( -1.000000000000000000, -0.000000000000000000, -0.000000000000000000 ) ) ;
#57644 = CARTESIAN_POINT ( 'NONE',  ( 16.13486940644654766, 11.28601765141728741, -1.500000000000002220 ) ) ;
#57645 = VECTOR ( 'NONE', #46701, 1000.000000000000000 ) ;
#57646 = CARTESIAN_POINT ( 'NONE',  ( -28.52287095715005805, -23.31185441368106126, 11.44779303854528685 ) ) ;
#57647 = PERSON_AND_ORGANIZATION_ROLE ( 'classification_officer' ) ;
#57648 = CARTESIAN_POINT ( 'NONE',  ( -103.5228709571500758, -24.64898659630367916, 1.056161002820829697 ) ) ;
#57649 = CARTESIAN_POINT ( 'NONE',  ( 3.362850247043494001, -6.376774720514404748, 18.65880685207958223 ) ) ;
#57650 = CARTESIAN_POINT ( 'NONE',  ( 10.61356161029474521, 17.70173163822984819, 11.49999999999999645 ) ) ;
#57651 = B_SPLINE_CURVE_WITH_KNOTS ( 'NONE', 3,
 ( #85168, #47125, #940, #78038, #8551, #31890, #93781, #24272, #86671, #46625 ),
 .UNSPECIFIED., .F., .F.,
 ( 4, 3, 3, 4 ),
 ( 0.000000000000000000, 0.0001187730049107982994, 0.0002375745643523147167, 0.0004748892031761914605 ),
 .UNSPECIFIED. ) ;
#57652 = DIRECTION ( 'NONE',  ( 0.000000000000000000, 0.000000000000000000, -1.000000000000000000 ) ) ;
#57654 = EDGE_CURVE ( 'NONE', #71712, #46766, #57856, .T. ) ;
#57653 = CARTESIAN_POINT ( 'NONE',  ( -17.75566480456612695, 14.03706703302619374, 11.49999999999999645 ) ) ;
#57655 = ORIENTED_EDGE ( 'NONE', *, *, #60816, .T. ) ;
#57656 = DIRECTION ( 'NONE',  ( -3.773278334453079030E-23, 0.9999999999976377785, 2.173523156925979128E-06 ) ) ;
#57657 = CARTESIAN_POINT ( 'NONE',  ( -97.54592858886259421, -24.65952944569304606, 1.056160979905701680 ) ) ;
#57658 = CARTESIAN_POINT ( 'NONE',  ( -127.5228709571500616, -23.95044443724993144, 10.65354141964648882 ) ) ;
#57659 = DIRECTION ( 'NONE',  ( -0.000000000000000000, -1.000000000000000000, -0.000000000000000000 ) ) ;
#57660 = B_SPLINE_CURVE_WITH_KNOTS ( 'NONE', 3,
 ( #31849, #10003, #33334, #87637, #19110, #35842 ),
 .UNSPECIFIED., .F., .F.,
 ( 4, 2, 4 ),
 ( 0.000000000000000000, 0.001380901958385387894, 0.002761803916770775788 ),
 .UNSPECIFIED. ) ;
#57661 = ORIENTED_EDGE ( 'NONE', *, *, #68237, .T. ) ;
#57662 = CARTESIAN_POINT ( 'NONE',  ( -84.52287095715006160, -23.47596703998600631, 11.44779298504228571 ) ) ;
#57663 = CARTESIAN_POINT ( 'NONE',  ( -5.953223121155255981, 22.05028593715628560, -1.500000000000002220 ) ) ;
#57664 = CARTESIAN_POINT ( 'NONE',  ( -74.58127051957136189, -24.65952944569304606, 1.056160979905701680 ) ) ;
#57665 = LINE ( 'NONE', #88608, #60951 ) ;
#57666 = CARTESIAN_POINT ( 'NONE',  ( -82.51746163132445133, -23.73791477778912196, 11.05961554403170943 ) ) ;
#57667 = AXIS2_PLACEMENT_3D ( 'NONE', #53903, #54401, #78216 ) ;
#57668 = CARTESIAN_POINT ( 'NONE',  ( -8.346146134265904237, -20.86121191590761015, 11.49999999999999645 ) ) ;
#57669 = ORIENTED_EDGE ( 'NONE', *, *, #79553, .F. ) ;
#57670 = CARTESIAN_POINT ( 'NONE',  ( -43.49282179846755270, -24.34968618360933235, 0.1864209137778850833 ) ) ;
#57671 = CARTESIAN_POINT ( 'NONE',  ( 6.372119535971386917, -21.01724095701019479, 11.49999999999998934 ) ) ;
#57672 = EDGE_CURVE ( 'NONE', #16871, #62504, #97876, .T. ) ;
#57673 = FACE_OUTER_BOUND ( 'NONE', #95257, .T. ) ;
#57674 = CARTESIAN_POINT ( 'NONE',  ( -29.20082839157102583, -25.21724613326715314, 5.852069579333174509 ) ) ;
#57675 = ORIENTED_EDGE ( 'NONE', *, *, #30567, .F. ) ;
#57676 = CARTESIAN_POINT ( 'NONE',  ( -7.160000000000000142, 0.1579206558577707364, 6.788828319098143105 ) ) ;
#57677 = CARTESIAN_POINT ( 'NONE',  ( -107.5228709571501042, -23.72773821059536914, 11.05748984161097503 ) ) ;
#57678 = VERTEX_POINT ( 'NONE', #80173 ) ;
#57679 = ADVANCED_FACE ( 'NONE', ( #65476 ), #59614, .T. ) ;
#57680 = FACE_OUTER_BOUND ( 'NONE', #16137, .T. ) ;
#57681 = CARTESIAN_POINT ( 'NONE',  ( -7.444040098415714013, -19.11467064512029879, -1.500000000000002220 ) ) ;
#57682 = ORIENTED_EDGE ( 'NONE', *, *, #37906, .T. ) ;
#57683 = EDGE_LOOP ( 'NONE', ( #54535, #50340, #48822, #58707 ) ) ;
#57684 = EDGE_LOOP ( 'NONE', ( #88282, #2293, #38575, #33416, #11423, #47053, #78801, #42473, #22079, #5270, #36046, #22288 ) ) ;
#57685 = CARTESIAN_POINT ( 'NONE',  ( 2.905029696106983916, -6.376774720514415407, 20.12486936895525957 ) ) ;
#57686 = CARTESIAN_POINT ( 'NONE',  ( 17.26854690438276307, -15.35948741044508559, -1.500000000000002220 ) ) ;
#57687 = CARTESIAN_POINT ( 'NONE',  ( -104.5551257925524453, -23.96169478059714208, 10.65365249895717525 ) ) ;
#57688 = CARTESIAN_POINT ( 'NONE',  ( 20.12614038868121824, 2.982395457389826809, -1.500000000000002220 ) ) ;
#57689 = ORIENTED_EDGE ( 'NONE', *, *, #92513, .T. ) ;
#57690 = CARTESIAN_POINT ( 'NONE',  ( -70.43580950499047333, -25.03347651911512273, 7.560241782797326060 ) ) ;
#57691 = EDGE_CURVE ( 'NONE', #26881, #62407, #21747, .T. ) ;
#57692 = CARTESIAN_POINT ( 'NONE',  ( -29.50320195067551765, -23.87474868272149209, 10.65365256123546978 ) ) ;
#57693 = EDGE_CURVE ( 'NONE', #35458, #24252, #90484, .T. ) ;
#57694 = CARTESIAN_POINT ( 'NONE',  ( -105.5930656460468953, -24.15503026093913164, -0.2815557561904565298 ) ) ;
#57695 = CARTESIAN_POINT ( 'NONE',  ( -19.80875734969026425, -0.3587747205144265483, 30.51402280011862089 ) ) ;
#57696 = VERTEX_POINT ( 'NONE', #99865 ) ;
#57697 = CARTESIAN_POINT ( 'NONE',  ( -29.22054808153496808, -24.76881279543748704, 4.231944355383084222 ) ) ;
#57698 = PLANE ( 'NONE',  #92819 ) ;
#57699 = EDGE_CURVE ( 'NONE', #7760, #95350, #17129, .T. ) ;
#57700 = VERTEX_POINT ( 'NONE', #82662 ) ;
#57701 = CARTESIAN_POINT ( 'NONE',  ( -20.73834036848188234, 1.213307192923735345, -1.500000000000002220 ) ) ;
#57702 = ORIENTED_EDGE ( 'NONE', *, *, #19760, .F. ) ;
#57704 = EDGE_LOOP ( 'NONE', ( #15, #36203, #57797, #24190 ) ) ;
#57703 = DIRECTION ( 'NONE',  ( 0.000000000000000000, 1.000000000000000000, -0.000000000000000000 ) ) ;
#57705 = VECTOR ( 'NONE', #97822, 1000.000000000000000 ) ;
#57706 = CARTESIAN_POINT ( 'NONE',  ( -86.62287095715004170, -24.65952944569304606, 1.056160979905700348 ) ) ;
#57707 = CARTESIAN_POINT ( 'NONE',  ( -107.6228709571500843, -23.72747288104441665, -1.053458166803660889 ) ) ;
#57708 = ORIENTED_EDGE ( 'NONE', *, *, #23778, .T. ) ;
#57709 = EDGE_LOOP ( 'NONE', ( #37488, #96071, #70325, #48862 ) ) ;
#57710 = AXIS2_PLACEMENT_3D ( 'NONE', #23740, #47099, #68922 ) ;
#57711 = CARTESIAN_POINT ( 'NONE',  ( -33.52287095715006160, -23.47596703998600631, 11.44779298504229459 ) ) ;
#57712 = CARTESIAN_POINT ( 'NONE',  ( -116.6228709571500417, -23.48786465467241769, 11.44779295918253759 ) ) ;
#57713 = VECTOR ( 'NONE', #58615, 1000.000000000000114 ) ;
#57714 = CARTESIAN_POINT ( 'NONE',  ( -43.55308972817040569, -23.96169478059712787, 10.65365249895718769 ) ) ;
#57715 = ADVANCED_FACE ( 'NONE', ( #36990 ), #30876, .T. ) ;
#57717 = VERTEX_POINT ( 'NONE', #20753 ) ;
#57716 = CARTESIAN_POINT ( 'NONE',  ( -22.03165466229905789, 1.424673820674137614, 11.49999999999999645 ) ) ;
#57718 = VECTOR ( 'NONE', #19153, 1000.000000000000114 ) ;
#57719 = FACE_OUTER_BOUND ( 'NONE', #91403, .T. ) ;
#57720 = CARTESIAN_POINT ( 'NONE',  ( 11.26306171725914851, -19.60737681494043727, -1.500000000000002220 ) ) ;
#57721 = VECTOR ( 'NONE', #233, 1000.000000000000114 ) ;
#57723 = VERTEX_POINT ( 'NONE', #60845 ) ;
#57722 = DIRECTION ( 'NONE',  ( -1.000000000000000000, -3.773278334444167608E-23, -8.201307833595939069E-29 ) ) ;
#57724 = ORIENTED_EDGE ( 'NONE', *, *, #45987, .T. ) ;
#57725 = FACE_OUTER_BOUND ( 'NONE', #85890, .T. ) ;
#57726 = EDGE_CURVE ( 'NONE', #70639, #73004, #80789, .T. ) ;
#57727 = B_SPLINE_CURVE_WITH_KNOTS ( 'NONE', 3,
 ( #37853, #60708, #6900, #61703, #99726, #22112, #92131, #61211, #76888, #7389, #69300, #23105, #32732, #94127, #24611, #95139 ),
 .UNSPECIFIED., .F., .F.,
 ( 4, 2, 2, 2, 2, 2, 2, 4 ),
 ( 0.000000000000000000, 0.0002661357119279468509, 0.0005322714238558924008, 0.001064542847711783501, 0.001330678559639729159, 0.001596814271567674817, 0.001862949983495620476, 0.002129085695423566134 ),
 .UNSPECIFIED. ) ;
#57728 = ADVANCED_FACE ( 'NONE', ( #76036, #29373 ), #60350, .T. ) ;
#57729 = FACE_OUTER_BOUND ( 'NONE', #48314, .T. ) ;
#57730 = ORIENTED_EDGE ( 'NONE', *, *, #12309, .F. ) ;
#57731 = CARTESIAN_POINT ( 'NONE',  ( -13.58512445790048417, 16.25115196636789250, -1.500000000000002220 ) ) ;
#57732 = FACE_OUTER_BOUND ( 'NONE', #33536, .T. ) ;
#57733 = DIRECTION ( 'NONE',  ( 0.000000000000000000, 2.173523156925980399E-06, -0.9999999999976378895 ) ) ;
#57734 = CARTESIAN_POINT ( 'NONE',  ( -13.27262489239681997, 17.90159134968837051, -1.500000000000002220 ) ) ;
#57735 = FACE_OUTER_BOUND ( 'NONE', #48167, .T. ) ;
#57736 = EDGE_CURVE ( 'NONE', #63440, #27806, #84155, .T. ) ;
#57737 = ORIENTED_EDGE ( 'NONE', *, *, #21854, .T. ) ;
#57738 = CARTESIAN_POINT ( 'NONE',  ( -80.52287095715006160, -23.47596703998600631, 11.44779298504228571 ) ) ;
#57739 = DIRECTION ( 'NONE',  ( -0.000000000000000000, 0.000000000000000000, 1.000000000000000000 ) ) ;
#57740 = VECTOR ( 'NONE', #14504, 1000.000000000000000 ) ;
#57741 = ADVANCED_FACE ( 'NONE', ( #46110 ), #35279, .T. ) ;
#57742 = CARTESIAN_POINT ( 'NONE',  ( -41.51830428958714947, -25.18393819603653583, 3.285814443599428980 ) ) ;
#57743 = CARTESIAN_POINT ( 'NONE',  ( -116.5895376238167387, -24.64898659630368627, 1.056161002820393158 ) ) ;
#57744 = ADVANCED_FACE ( 'NONE', ( #86162 ), #88730, .T. ) ;
#57745 = CARTESIAN_POINT ( 'NONE',  ( -13.24781383850973349, 14.34467480260970795, -1.500000000000002220 ) ) ;
#57746 = CARTESIAN_POINT ( 'NONE',  ( 5.397486108853063236, 20.74927772461418485, 11.49999999999998934 ) ) ;
#57747 = CARTESIAN_POINT ( 'NONE',  ( -27.40838375831408058, -24.57999501220895411, 1.648157300620804344 ) ) ;
#57748 = DIRECTION ( 'NONE',  ( 0.000000000000000000, -1.000000000000000000, 0.000000000000000000 ) ) ;
#57749 = CARTESIAN_POINT ( 'NONE',  ( -77.54284170824401201, -24.51314013834315375, 0.6176544820404117342 ) ) ;
#57750 = CARTESIAN_POINT ( 'NONE',  ( 12.23086119556625206, 19.17791753167082192, -1.500000000000002220 ) ) ;
#57751 = DIRECTION ( 'NONE',  ( -8.847089727481724810E-17, 1.000000000000000000, 5.551115123125785167E-17 ) ) ;
#57752 = CARTESIAN_POINT ( 'NONE',  ( -102.5194659324134676, -23.73766607897671577, -1.055555164236430254 ) ) ;
#57753 = CARTESIAN_POINT ( 'NONE',  ( -128.5228709571500758, -24.64898659630368627, 1.056161002820834804 ) ) ;
#57754 = CARTESIAN_POINT ( 'NONE',  ( 2.927915493035635031, 19.71835975189664936, 11.49999999999999645 ) ) ;
#57755 = CARTESIAN_POINT ( 'NONE',  ( -31.52287095715004739, -24.33832256527048088, 0.1851278514138553211 ) ) ;
#57756 = CARTESIAN_POINT ( 'NONE',  ( -128.5228709571499905, -24.33927499327855770, 9.819080762295804732 ) ) ;
#57757 = CARTESIAN_POINT ( 'NONE',  ( -48.55326441215460420, -23.96119346886881019, -0.6495511937831938143 ) ) ;
#57758 = VERTEX_POINT ( 'NONE', #31881 ) ;
#57759 = DIRECTION ( 'NONE',  ( -0.000000000000000000, -1.000000000000000000, -0.000000000000000000 ) ) ;
#57760 = CARTESIAN_POINT ( 'NONE',  ( -31.82683686962402447, -24.87219037988794312, 1.747789950295619787 ) ) ;
#57761 = CARTESIAN_POINT ( 'NONE',  ( 20.80172415560569021, 6.174449132348904357, -1.500000000000002220 ) ) ;
#57762 = CARTESIAN_POINT ( 'NONE',  ( -56.50840713276495109, -23.96169478059713498, 10.65365249895718236 ) ) ;
#57763 = CARTESIAN_POINT ( 'NONE',  ( -18.91883139384513157, -4.797682538509264738, -1.500000000000002220 ) ) ;
#57764 = VECTOR ( 'NONE', #91560, 1000.000000000000000 ) ;
#57765 = CARTESIAN_POINT ( 'NONE',  ( -55.65727299751092261, -23.85049219812685806, 10.88485053497527133 ) ) ;
#57766 = ORIENTED_EDGE ( 'NONE', *, *, #63449, .T. ) ;
#57767 = DATE_AND_TIME ( #39642, #13393 ) ;
#57768 = LINE ( 'NONE', #65401, #66240 ) ;
#57769 = CARTESIAN_POINT ( 'NONE',  ( 1.945971545120378288, -20.36639758168144709, 11.49999999999999645 ) ) ;
#57770 = DIRECTION ( 'NONE',  ( -0.000000000000000000, -1.000000000000000000, -0.000000000000000000 ) ) ;
#57771 = AXIS2_PLACEMENT_3D ( 'NONE', #32022, #62998, #87310 ) ;
#57772 = PLANE ( 'NONE',  #77216 ) ;
#57773 = EDGE_LOOP ( 'NONE', ( #19478, #36262, #4259, #85905 ) ) ;
#57774 = CARTESIAN_POINT ( 'NONE',  ( -52.92287095715005307, -23.47596703998600276, 11.44779298504227683 ) ) ;
#57775 = LINE ( 'NONE', #74965, #52546 ) ;
#57776 = VECTOR ( 'NONE', #72647, 1000.000000000000000 ) ;
#57777 = DIRECTION ( 'NONE',  ( 0.000000000000000000, 0.000000000000000000, 1.000000000000000000 ) ) ;
#57778 = AXIS2_PLACEMENT_3D ( 'NONE', #29859, #37479, #47971 ) ;
#57779 = CARTESIAN_POINT ( 'NONE',  ( -55.62287095715005592, -23.47593901973091235, -1.443836447539007972 ) ) ;
#57780 = VERTEX_POINT ( 'NONE', #33371 ) ;
#57781 = CARTESIAN_POINT ( 'NONE',  ( -24.90875734969025501, 3.316774720514426456, 27.45402280011862572 ) ) ;
#57782 = AXIS2_PLACEMENT_3D ( 'NONE', #78574, #1484, #78075 ) ;
#57783 = CARTESIAN_POINT ( 'NONE',  ( -3.987988226355533072, 22.59150145119509290, 11.49999999999999645 ) ) ;
#57784 = CARTESIAN_POINT ( 'NONE',  ( 7.533951754900199305, 21.46025436219600024, 11.49999999999998934 ) ) ;
#57785 = CARTESIAN_POINT ( 'NONE',  ( -70.79215990384717827, -25.05760859634946414, 7.494946593071406760 ) ) ;
#57786 = FACE_OUTER_BOUND ( 'NONE', #95566, .T. ) ;
#57787 = CARTESIAN_POINT ( 'NONE',  ( -2.499999999999993339, 18.99999999999977618, 2.100000000000000089 ) ) ;
#57788 = CARTESIAN_POINT ( 'NONE',  ( 8.160000000000000142, -9.652339641703484574, 1.560255187525485976 ) ) ;
#57789 = CARTESIAN_POINT ( 'NONE',  ( -69.34467035722860828, -25.24945287413907380, 6.270865876356967128 ) ) ;
#57790 = CARTESIAN_POINT ( 'NONE',  ( -1.678574117887026373, -21.80011532881206548, -1.500000000000002220 ) ) ;
#57791 = PLANE ( 'NONE',  #52691 ) ;
#57792 = ADVANCED_FACE ( 'NONE', ( #80550 ), #44372, .F. ) ;
#57793 = B_SPLINE_CURVE_WITH_KNOTS ( 'NONE', 3,
 ( #72451, #67218, #12898, #83409 ),
 .UNSPECIFIED., .F., .F.,
 ( 4, 4 ),
 ( 0.000000000000000000, 9.999999999998900014E-05 ),
 .UNSPECIFIED. ) ;
#57794 = LINE ( 'NONE', #81618, #63889 ) ;
#57795 = LINE ( 'NONE', #43063, #53343 ) ;
#57796 = CARTESIAN_POINT ( 'NONE',  ( -58.57885350497856081, -24.65952944569304606, 1.056160979905697461 ) ) ;
#57797 = ORIENTED_EDGE ( 'NONE', *, *, #16428, .T. ) ;
#57798 = EDGE_CURVE ( 'NONE', #4648, #96462, #13396, .T. ) ;
#57799 = CARTESIAN_POINT ( 'NONE',  ( -18.43012528856881715, -8.789534013050598560, -1.500000000000002220 ) ) ;
#57800 = ORIENTED_EDGE ( 'NONE', *, *, #32131, .T. ) ;
#57801 = ORIENTED_EDGE ( 'NONE', *, *, #42828, .F. ) ;
#57802 = ORIENTED_EDGE ( 'NONE', *, *, #75095, .T. ) ;
#57803 = VERTEX_POINT ( 'NONE', #34383 ) ;
#57804 = CARTESIAN_POINT ( 'NONE',  ( 13.47786528765806580, -18.65256936556403744, -1.500000000000002220 ) ) ;
#57805 = PLANE ( 'NONE',  #27618 ) ;
#57806 = CARTESIAN_POINT ( 'NONE',  ( 18.20877288740043198, -8.745817889818592761, -1.500000000000002220 ) ) ;
#57807 = EDGE_CURVE ( 'NONE', #39894, #71598, #57793, .T. ) ;
#57808 = VERTEX_POINT ( 'NONE', #90040 ) ;
#57809 = CIRCLE ( 'NONE', #74021, 0.8160000000000007248 ) ;
#57810 = CARTESIAN_POINT ( 'NONE',  ( -59.52287095715006160, -29.50247984919015209, -1.443849546365056913 ) ) ;
#57811 = ADVANCED_FACE ( 'NONE', ( #25766 ), #61527, .F. ) ;
#57812 = DIRECTION ( 'NONE',  ( 0.000000000000000000, 0.000000000000000000, 1.000000000000000000 ) ) ;
#57813 = ADVANCED_FACE ( 'NONE', ( #10537 ), #21518, .T. ) ;
#57814 = CARTESIAN_POINT ( 'NONE',  ( 32.06540688909007741, -6.475225279485573360, -12.44045471929204716 ) ) ;
#57815 = CARTESIAN_POINT ( 'NONE',  ( -53.54759161719780991, -24.15620529776627734, 10.23563542870660825 ) ) ;
#57817 = ORIENTED_EDGE ( 'NONE', *, *, #24822, .F. ) ;
#57816 = CARTESIAN_POINT ( 'NONE',  ( -10.59417575825165159, 18.57464501519095279, 11.49999999999999645 ) ) ;
#57818 = PLANE ( 'NONE',  #45212 ) ;
#57819 = EDGE_CURVE ( 'NONE', #58649, #67935, #84358, .T. ) ;
#57820 = EDGE_LOOP ( 'NONE', ( #77404, #8535, #32538, #56910 ) ) ;
#57821 = CIRCLE ( 'NONE', #10861, 129.7684398600581517 ) ;
#57822 = CARTESIAN_POINT ( 'NONE',  ( -2.790049085472659396, -22.09070898310802633, 11.49999999999998934 ) ) ;
#57823 = CARTESIAN_POINT ( 'NONE',  ( -19.50335911044312098, -6.847048061534898977, -1.500000000000002220 ) ) ;
#57824 = ORIENTED_EDGE ( 'NONE', *, *, #28139, .T. ) ;
#57825 = CARTESIAN_POINT ( 'NONE',  ( -113.5895376238167245, -24.65952944569304961, 1.056160979905703678 ) ) ;
#57826 = ORIENTED_EDGE ( 'NONE', *, *, #2432, .T. ) ;
#57827 = FACE_OUTER_BOUND ( 'NONE', #88701, .T. ) ;
#57828 = ORIENTED_EDGE ( 'NONE', *, *, #87484, .T. ) ;
#57829 = CARTESIAN_POINT ( 'NONE',  ( 10.62437663934349530, 6.475225279485576024, -27.03002426119959978 ) ) ;
#57830 = CARTESIAN_POINT ( 'NONE',  ( -3.961239394588834895, 20.55660451852329018, -1.500000000000002220 ) ) ;
#57831 = EDGE_CURVE ( 'NONE', #42771, #94651, #34949, .T. ) ;
#57832 = CARTESIAN_POINT ( 'NONE',  ( 11.25260618158950621, 18.78031238747207610, 11.49999999999999645 ) ) ;
#57833 = DIRECTION ( 'NONE',  ( -1.000000000000000000, -3.773278334444166432E-23, -8.201307841325785021E-29 ) ) ;
#57834 = CARTESIAN_POINT ( 'NONE',  ( -22.50818191331092777, 0.9639279967183422837, 11.49999999999998934 ) ) ;
#57835 = VECTOR ( 'NONE', #78680, 1000.000000000000114 ) ;
#57836 = CARTESIAN_POINT ( 'NONE',  ( 18.03207908435136986, 10.65457695745678457, -1.500000000000002220 ) ) ;
#57837 = CARTESIAN_POINT ( 'NONE',  ( -89.40841769935767047, -25.26877885127129986, 5.947789088311301597 ) ) ;
#57838 = CARTESIAN_POINT ( 'NONE',  ( -106.5562042904834215, -23.47596703998600631, 11.44779298504227683 ) ) ;
#57839 = CARTESIAN_POINT ( 'NONE',  ( -119.6274284003628168, -23.73791477778912551, 11.05961554403169700 ) ) ;
#57840 = CARTESIAN_POINT ( 'NONE',  ( 33.13288845015618023, -5.965225279485572685, -0.1650522222209214185 ) ) ;
#57842 = VERTEX_POINT ( 'NONE', #34143 ) ;
#57841 = ADVANCED_FACE ( 'NONE', ( #70191, #31622, #93513 ), #58277, .F. ) ;
#57843 = B_SPLINE_CURVE_WITH_KNOTS ( 'NONE', 3,
 ( #50533, #50047, #88106, #80982 ),
 .UNSPECIFIED., .F., .F.,
 ( 4, 4 ),
 ( 2.531585061196475251E-09, 0.002563035601033511121 ),
 .UNSPECIFIED. ) ;
#57844 = ORIENTED_EDGE ( 'NONE', *, *, #85517, .T. ) ;
#57845 = ORIENTED_EDGE ( 'NONE', *, *, #77029, .F. ) ;
#57846 = DIRECTION ( 'NONE',  ( -0.000000000000000000, -1.000000000000000000, -0.000000000000000000 ) ) ;
#57847 = EDGE_LOOP ( 'NONE', ( #46978, #62517, #74237, #84800 ) ) ;
#57848 = EDGE_CURVE ( 'NONE', #10813, #18192, #80289, .T. ) ;
#57849 = AXIS2_PLACEMENT_3D ( 'NONE', #10477, #26208, #71895 ) ;
#57850 = CARTESIAN_POINT ( 'NONE',  ( 10.45947017991876926, -18.73710855793504848, -1.500000000000002220 ) ) ;
#57851 = ORIENTED_EDGE ( 'NONE', *, *, #34254, .F. ) ;
#57852 = CARTESIAN_POINT ( 'NONE',  ( 0.3910256410256394144, -5.876774720514411854, 19.63681891025641235 ) ) ;
#57853 = AXIS2_PLACEMENT_3D ( 'NONE', #2422, #18136, #26252 ) ;
#57854 = CARTESIAN_POINT ( 'NONE',  ( 21.06685942672242362, 1.161445541649065882, 11.49999999999998934 ) ) ;
#57855 = CARTESIAN_POINT ( 'NONE',  ( 30.93860345374796594, -6.475225279485573360, 19.84760796525321780 ) ) ;
#57856 = LINE ( 'NONE', #3557, #39784 ) ;
#57857 = CARTESIAN_POINT ( 'NONE',  ( -50.49351916561946751, -24.40133493613049609, 9.663955038902804162 ) ) ;
#57858 = AXIS2_PLACEMENT_3D ( 'NONE', #75281, #58577, #98616 ) ;
#57859 = DIRECTION ( 'NONE',  ( -3.773278334453079618E-23, 0.9999999999976377785, 2.173523156925979975E-06 ) ) ;
#57860 = CARTESIAN_POINT ( 'NONE',  ( -129.6236597985572985, -24.15620529776629510, 10.23563542870659759 ) ) ;
#57861 = CARTESIAN_POINT ( 'NONE',  ( 1.153593019990587942, -22.03401787307112869, -1.500000000000002220 ) ) ;
#57862 = ORIENTED_EDGE ( 'NONE', *, *, #4304, .T. ) ;
#57863 = CARTESIAN_POINT ( 'NONE',  ( -65.56867036171823315, -23.48786465467241058, 11.44779295918254824 ) ) ;
#57864 = DIRECTION ( 'NONE',  ( -3.773278334453079618E-23, 0.9999999999976377785, 2.173523156925979975E-06 ) ) ;
#57865 = FACE_OUTER_BOUND ( 'NONE', #90055, .T. ) ;
#57866 = AXIS2_PLACEMENT_3D ( 'NONE', #73686, #4182, #22864 ) ;
#57867 = EDGE_CURVE ( 'NONE', #20563, #63176, #2693, .T. ) ;
#57868 = CARTESIAN_POINT ( 'NONE',  ( -47.52287095715006160, -24.64898659630528854, 1.056161002820821038 ) ) ;
#57869 = DIRECTION ( 'NONE',  ( 0.000000000000000000, -1.000000000000000000, 0.000000000000000000 ) ) ;
#57870 = CARTESIAN_POINT ( 'NONE',  ( 21.01207135711032237, 3.775690236426352264, -1.500000000000002220 ) ) ;
#57871 = LINE ( 'NONE', #71082, #36896 ) ;
#57872 = CARTESIAN_POINT ( 'NONE',  ( -90.25587550125513303, -25.31768024997816724, 4.634761245912266681 ) ) ;
#57873 = EDGE_CURVE ( 'NONE', #40969, #34853, #33128, .T. ) ;
#57874 = CARTESIAN_POINT ( 'NONE',  ( -8.160000000000000142, -10.15233964170348457, 0.003711184059992174607 ) ) ;
#57875 = CARTESIAN_POINT ( 'NONE',  ( -80.94394040031853876, -25.13915873745154883, 7.007560659833019123 ) ) ;
#57876 = CARTESIAN_POINT ( 'NONE',  ( 19.01167203989450982, 12.12494712425435850, -1.500000000000002220 ) ) ;
#57877 = FACE_OUTER_BOUND ( 'NONE', #5640, .T. ) ;
#57878 = VERTEX_POINT ( 'NONE', #63096 ) ;
#57879 = CARTESIAN_POINT ( 'NONE',  ( 4.547994309883463870, -5.876774720514421624, 20.87593061325451416 ) ) ;
#57880 = CARTESIAN_POINT ( 'NONE',  ( -79.62973999110049306, -24.34968618360933945, 0.1864209137778814473 ) ) ;
#57881 = CARTESIAN_POINT ( 'NONE',  ( -19.47062899137607772, 3.135797168518691169, 11.49999999999999645 ) ) ;
#57882 = DIRECTION ( 'NONE',  ( 1.000000000000000000, 3.773278334444166432E-23, 8.201307841325785021E-29 ) ) ;
#57883 = DIRECTION ( 'NONE',  ( 0.000000000000000000, 0.000000000000000000, -1.000000000000000000 ) ) ;
#57884 = ADVANCED_FACE ( 'NONE', ( #94023 ), #32626, .T. ) ;
#57885 = ORIENTED_EDGE ( 'NONE', *, *, #60657, .T. ) ;
#57886 = PLANE ( 'NONE',  #97636 ) ;
#57887 = CARTESIAN_POINT ( 'NONE',  ( -29.81175120719462157, -24.60094610731835729, 4.942812391584706866 ) ) ;
#57888 = CARTESIAN_POINT ( 'NONE',  ( -113.5562042904833788, -24.64898659630528854, 1.056161002820831474 ) ) ;
#57889 = CARTESIAN_POINT ( 'NONE',  ( -19.98381242416700587, 8.274006965216138099, -1.500000000000002220 ) ) ;
#57890 = VECTOR ( 'NONE', #30489, 1000.000000000000114 ) ;
#57891 = CARTESIAN_POINT ( 'NONE',  ( -88.52287095715006160, -23.47593901973090524, -1.443836447538996426 ) ) ;
#57892 = DIRECTION ( 'NONE',  ( 0.000000000000000000, -1.000000000000000000, 0.000000000000000000 ) ) ;
#57893 = CARTESIAN_POINT ( 'NONE',  ( -50.58953762381672448, -23.47593901973091235, -1.443836447539009749 ) ) ;
#57894 = CARTESIAN_POINT ( 'NONE',  ( -81.09999867506596161, -25.06835676914625211, 7.442983283209521517 ) ) ;
#57895 = CARTESIAN_POINT ( 'NONE',  ( -14.06767371131996214, 13.90018863433869889, 11.49999999999998934 ) ) ;
#57896 = EDGE_LOOP ( 'NONE', ( #67478, #49432, #13231, #5742 ) ) ;
#57897 = VECTOR ( 'NONE', #87553, 1000.000000000000000 ) ;
#57898 = CARTESIAN_POINT ( 'NONE',  ( -20.02346298389695534, -3.155783441878276196, 11.49999999999999645 ) ) ;
#57899 = CYLINDRICAL_SURFACE ( 'NONE', #55357, 18.35000000000000142 ) ;
#57900 = ORIENTED_EDGE ( 'NONE', *, *, #94154, .F. ) ;
#57901 = PLANE ( 'NONE',  #89676 ) ;
#57902 = CARTESIAN_POINT ( 'NONE',  ( 31.61406883670153789, 4.508386143373845023, 26.44289287685778334 ) ) ;
#57903 = CARTESIAN_POINT ( 'NONE',  ( 0.000000000000000000, -1.530000000000000027, 0.3849999999999990652 ) ) ;
#57904 = DIRECTION ( 'NONE',  ( 0.000000000000000000, -0.000000000000000000, -1.000000000000000000 ) ) ;
#57905 = CARTESIAN_POINT ( 'NONE',  ( -120.5562042904834072, -23.48786465467241413, 11.44779295918253759 ) ) ;
#57906 = CARTESIAN_POINT ( 'NONE',  ( -13.81204400269958654, 14.50282280199826701, 11.49999999999998934 ) ) ;
#57907 = DIRECTION ( 'NONE',  ( -1.000000000000000000, 0.000000000000000000, 0.000000000000000000 ) ) ;
#57908 = EDGE_LOOP ( 'NONE', ( #42974, #78541, #9810, #68928 ) ) ;
#57909 = VECTOR ( 'NONE', #88299, 1000.000000000000114 ) ;
#57910 = FACE_OUTER_BOUND ( 'NONE', #23835, .T. ) ;
#57911 = FACE_OUTER_BOUND ( 'NONE', #10660, .T. ) ;
#57912 = PLANE ( 'NONE',  #77770 ) ;
#57913 = PLANE ( 'NONE',  #25373 ) ;
#57914 = CARTESIAN_POINT ( 'NONE',  ( -73.64957981708161583, -23.48783264082477018, -1.443836473390094355 ) ) ;
#57915 = VECTOR ( 'NONE', #72417, 1000.000000000000000 ) ;
#57916 = CARTESIAN_POINT ( 'NONE',  ( 14.58759567797699574, 3.520387117721317072, -28.38990266974735732 ) ) ;
#57917 = EDGE_CURVE ( 'NONE', #76505, #23443, #41987, .T. ) ;
#57918 = CARTESIAN_POINT ( 'NONE',  ( 8.286623624103266097E-13, -23.05000000000000426, 11.49999999999999645 ) ) ;
#57919 = EDGE_LOOP ( 'NONE', ( #97742, #20601, #41782, #58789 ) ) ;
#57920 = ADVANCED_FACE ( 'NONE', ( #25518 ), #17909, .F. ) ;
#57921 = VECTOR ( 'NONE', #61841, 1000.000000000000114 ) ;
#57922 = CARTESIAN_POINT ( 'NONE',  ( 15.76184642470745700, 12.85868457875834103, 11.49999999999998934 ) ) ;
#57924 = EDGE_CURVE ( 'NONE', #97996, #66785, #10513, .T. ) ;
#57923 = ORIENTED_EDGE ( 'NONE', *, *, #4848, .F. ) ;
#57925 = CARTESIAN_POINT ( 'NONE',  ( -17.89994474767736676, -14.32179853049041363, -1.500000000000002220 ) ) ;
#57926 = CARTESIAN_POINT ( 'NONE',  ( -32.60153195108193813, -23.96119346886880663, -0.6495511937831992544 ) ) ;
#57927 = EDGE_CURVE ( 'NONE', #35458, #8654, #25006, .T. ) ;
#57928 = ORIENTED_EDGE ( 'NONE', *, *, #95468, .F. ) ;
#57929 = DIRECTION ( 'NONE',  ( 0.000000000000000000, 0.000000000000000000, -1.000000000000000000 ) ) ;
#57930 = EDGE_CURVE ( 'NONE', #43884, #2131, #67336, .T. ) ;
#57931 = CARTESIAN_POINT ( 'NONE',  ( -49.44941220326682441, -25.26264084044488811, 6.666982223683588060 ) ) ;
#57932 = CARTESIAN_POINT ( 'NONE',  ( 29.73860345376319003, 1.477225279485574028, 19.84760796525321425 ) ) ;
#57933 = CARTESIAN_POINT ( 'NONE',  ( -21.05374637409849825, 2.266213160971460194, 11.49999999999999645 ) ) ;
#57934 = CARTESIAN_POINT ( 'NONE',  ( -2.513997614918375589, -22.02279109229760223, 11.49999999999998934 ) ) ;
#57935 = B_SPLINE_CURVE_WITH_KNOTS ( 'NONE', 3,
 ( #83720, #21807, #52784, #14198 ),
 .UNSPECIFIED., .F., .F.,
 ( 4, 4 ),
 ( 1.387778780781445521E-17, 9.999999999997510880E-05 ),
 .UNSPECIFIED. ) ;
#57936 = CARTESIAN_POINT ( 'NONE',  ( 3.086129920417311823, 20.35385046113321295, 11.49999999999998934 ) ) ;
#57937 = ORIENTED_EDGE ( 'NONE', *, *, #79560, .F. ) ;
#57938 = CARTESIAN_POINT ( 'NONE',  ( -41.60818966792778184, -23.73766607897670866, -1.055555164236441801 ) ) ;
#57939 = EDGE_LOOP ( 'NONE', ( #98754, #6459, #62474, #32217 ) ) ;
#57940 = DIRECTION ( 'NONE',  ( -0.06916465693916194757, -0.000000000000000000, 0.9976052577199501226 ) ) ;
#57941 = LINE ( 'NONE', #19352, #48636 ) ;
#57942 = ORIENTED_EDGE ( 'NONE', *, *, #16225, .F. ) ;
#57943 = ORIENTED_EDGE ( 'NONE', *, *, #34101, .F. ) ;
#57944 = VERTEX_POINT ( 'NONE', #59976 ) ;
#57945 = DIRECTION ( 'NONE',  ( 0.000000000000000000, 1.000000000000000000, 0.000000000000000000 ) ) ;
#57946 = DIRECTION ( 'NONE',  ( 0.4821794293845152457, 1.904163831934039853E-06, -0.8760724843726103162 ) ) ;
#57947 = CARTESIAN_POINT ( 'NONE',  ( -130.5728709571500588, -23.47596703998600631, 11.44779298504227860 ) ) ;
#57948 = CARTESIAN_POINT ( 'NONE',  ( -8.830788454959730416, 18.81286502489961876, -1.500000000000002220 ) ) ;
#57949 = CARTESIAN_POINT ( 'NONE',  ( -18.42844947050907578, 11.51566461966115540, 11.49999999999999645 ) ) ;
#57950 = VERTEX_POINT ( 'NONE', #27526 ) ;
#57951 = CARTESIAN_POINT ( 'NONE',  ( -127.6228709571500559, -24.65952944569305316, 1.056160979905707897 ) ) ;
#57952 = CIRCLE ( 'NONE', #9318, 3.500000000000000000 ) ;
#57953 = CARTESIAN_POINT ( 'NONE',  ( -115.5535853569740965, -24.40034930558990567, 0.3402023900116066257 ) ) ;
#57954 = CARTESIAN_POINT ( 'NONE',  ( 20.99545381566289137, 7.807860396396394620, -1.500000000000002220 ) ) ;
#57955 = LINE ( 'NONE', #72669, #56223 ) ;
#57956 = DIRECTION ( 'NONE',  ( -3.773278334453079618E-23, 0.9999999999976377785, 2.173523156925979975E-06 ) ) ;
#57957 = ORIENTED_EDGE ( 'NONE', *, *, #32240, .T. ) ;
#57958 = LINE ( 'NONE', #40714, #67966 ) ;
#57959 = CARTESIAN_POINT ( 'NONE',  ( 12.36220485508518685, -4.378682769551595300, -27.78718873729292582 ) ) ;
#57960 = B_SPLINE_SURFACE_WITH_KNOTS ( 'NONE', 3, 3, ( 
 ( #33387, #79060, #86179, #9553 ),
 ( #49142, #55251, #47633, #70966 ),
 ( #17166, #8561, #79567, #32397 ),
 ( #1457, #39511, #947, #1959 ),
 ( #94788, #17668, #93281, #31394 ),
 ( #63372, #25276, #69953, #56255 ),
 ( #48641, #94286, #41018, #31897 ),
 ( #24770, #10055, #62872, #64376 ),
 ( #441, #95296, #8054, #56756 ),
 ( #87685, #39003, #93788, #55752 ) ),
 .UNSPECIFIED., .F., .F., .F.,
 ( 4, 3, 3, 4 ),
 ( 4, 4 ),
 ( 0.7022005934521633463, 0.7765311282011415628, 0.8508616629501198902, 0.9995227324480764342 ),
 ( 0.6995784262351472105, 0.7010080898895992840 ),
 .UNSPECIFIED. ) ;
#57961 = ORIENTED_EDGE ( 'NONE', *, *, #66764, .T. ) ;
#57962 = CIRCLE ( 'NONE', #32005, 1.306876713926001354 ) ;
#57963 = ORIENTED_EDGE ( 'NONE', *, *, #66977, .F. ) ;
#57964 = CARTESIAN_POINT ( 'NONE',  ( -87.62287095715005592, -23.72747288104441665, -1.053458166803660889 ) ) ;
#57965 = ORIENTED_EDGE ( 'NONE', *, *, #56687, .F. ) ;
#57966 = CARTESIAN_POINT ( 'NONE',  ( 19.98919582620916913, -7.218065965386815996, -1.500000000000002220 ) ) ;
#57967 = ORIENTED_EDGE ( 'NONE', *, *, #3128, .T. ) ;
#57968 = CARTESIAN_POINT ( 'NONE',  ( 0.000000000000000000, 1.682774720514426114, -1.352392034746782823 ) ) ;
#57969 = CARTESIAN_POINT ( 'NONE',  ( -0.06377455873143267340, 21.83884041771831619, 11.49999999999998934 ) ) ;
#57970 = CARTESIAN_POINT ( 'NONE',  ( -52.55339013111201751, -23.96169478059712787, 10.65365249895718769 ) ) ;
#57971 = CARTESIAN_POINT ( 'NONE',  ( 8.023449251107201974, -21.19570997880782670, 11.49999999999998934 ) ) ;
#57972 = CARTESIAN_POINT ( 'NONE',  ( -41.39385049892748469, -25.18430990895221200, 3.844044810517027955 ) ) ;
#57973 = CARTESIAN_POINT ( 'NONE',  ( -49.52287095715008292, -23.96177878511307213, 10.65340807706330217 ) ) ;
#57974 = CARTESIAN_POINT ( 'NONE',  ( 21.07893183998518438, -5.767110019903106455, -1.500000000000002220 ) ) ;
#57975 = CARTESIAN_POINT ( 'NONE',  ( -66.62287095715004170, -24.51283580621365132, 0.6167428607019709297 ) ) ;
#57976 = ORIENTED_EDGE ( 'NONE', *, *, #74613, .F. ) ;
#57977 = LINE ( 'NONE', #17392, #43759 ) ;
#57978 = CARTESIAN_POINT ( 'NONE',  ( -49.18705952543585624, -25.12782698363243128, 7.035471548030500344 ) ) ;
#57979 = EDGE_CURVE ( 'NONE', #95847, #60537, #73845, .T. ) ;
#57980 = VECTOR ( 'NONE', #51244, 1000.000000000000114 ) ;
#57981 = ORIENTED_EDGE ( 'NONE', *, *, #97067, .T. ) ;
#57982 = CARTESIAN_POINT ( 'NONE',  ( -30.62558287684645109, -24.04478067413149844, -0.4748248766032758805 ) ) ;
#57983 = VERTEX_POINT ( 'NONE', #82793 ) ;
#57984 = CARTESIAN_POINT ( 'NONE',  ( -113.5228709571500616, -23.47593901973090524, -1.443836447538996204 ) ) ;
#57985 = CARTESIAN_POINT ( 'NONE',  ( -0.05083659990941549051, -22.39188026470795023, 1.363349870542264863 ) ) ;
#57986 = CARTESIAN_POINT ( 'NONE',  ( -12.29646723538143505, -17.35194501319736560, -1.500000000000002220 ) ) ;
#57987 = CARTESIAN_POINT ( 'NONE',  ( -28.49194798280534968, -6.376774720514426953, 28.38521343323375490 ) ) ;
#57988 = CARTESIAN_POINT ( 'NONE',  ( -26.30595710371889950, -24.97064650647640249, 3.418818890720438208 ) ) ;
#57989 = EDGE_CURVE ( 'NONE', #64635, #77501, #28022, .T. ) ;
#57990 = DIRECTION ( 'NONE',  ( -0.9796516281416185468, 4.362379964674604143E-07, -0.2007054744626703968 ) ) ;
#57991 = AXIS2_PLACEMENT_3D ( 'NONE', #100070, #30586, #47822 ) ;
#57992 = CARTESIAN_POINT ( 'NONE',  ( -84.62287095715007013, -23.48786465467241769, 11.44779295918254469 ) ) ;
#57993 = ADVANCED_FACE ( 'NONE', ( #11293 ), #74196, .F. ) ;
#57994 = CARTESIAN_POINT ( 'NONE',  ( 8.160000000000000142, -10.98394470431085601, -0.7905513910579705650 ) ) ;
#57995 = ORIENTED_EDGE ( 'NONE', *, *, #22735, .T. ) ;
#57996 = CARTESIAN_POINT ( 'NONE',  ( 12.07855387261060898, -15.37489856218140183, 11.49999999999999645 ) ) ;
#57997 = CARTESIAN_POINT ( 'NONE',  ( -5.544977400725785266, -6.376774720514411854, 19.92818918856636401 ) ) ;
#57998 = VECTOR ( 'NONE', #78659, 1000.000000000000114 ) ;
#57999 = B_SPLINE_CURVE_WITH_KNOTS ( 'NONE', 3,
 ( #48433, #26593, #97588, #41316, #42335, #87485, #73756, #80375, #57556, #19464 ),
 .UNSPECIFIED., .F., .F.,
 ( 4, 2, 2, 2, 4 ),
 ( 0.000000000000000000, 0.08666671201630674060, 0.1733334240326134812, 0.3466668480652273510, 0.6933336961304540358 ),
 .UNSPECIFIED. ) ;
#58000 = B_SPLINE_CURVE_WITH_KNOTS ( 'NONE', 3,
 ( #59952, #21353, #44220, #99970, #69553, #98479, #91374, #32, #52328, #20860, #28979, #51833, #30479, #75641 ),
 .UNSPECIFIED., .F., .F.,
 ( 4, 2, 2, 2, 2, 2, 4 ),
 ( 8.673617379884035472E-19, 0.0002414200208935323767, 0.0004828400417870638861, 0.0009656800835741269047, 0.001448520125361189978, 0.001689940146254730784, 0.001931360167148271807 ),
 .UNSPECIFIED. ) ;
#58001 = CARTESIAN_POINT ( 'NONE',  ( -79.34892427156343331, -25.26180990464883180, 6.036045387136124596 ) ) ;
#58002 = ORIENTED_EDGE ( 'NONE', *, *, #9781, .F. ) ;
#58003 = FACE_OUTER_BOUND ( 'NONE', #60581, .T. ) ;
#58004 = CARTESIAN_POINT ( 'NONE',  ( -99.63322708413970474, -25.31439593098938801, 5.473920184482165219 ) ) ;
#58005 = CARTESIAN_POINT ( 'NONE',  ( -90.52287095715003318, -23.85196035786899671, -0.8779234886475166810 ) ) ;
#58006 = CARTESIAN_POINT ( 'NONE',  ( -60.52287095715008292, -23.85196035786900737, -0.8779234886475210109 ) ) ;
#58007 = CARTESIAN_POINT ( 'NONE',  ( 9.442166470422634461, 17.27452087139410963, -1.500000000000002220 ) ) ;
#58008 = ORIENTED_EDGE ( 'NONE', *, *, #12535, .F. ) ;
#58009 = CARTESIAN_POINT ( 'NONE',  ( -94.62287095715005592, -24.64898659630528854, 1.056161002820827921 ) ) ;
#58010 = LINE ( 'NONE', #88942, #26912 ) ;
#58011 = PERSON_AND_ORGANIZATION ( #70597, #27821 ) ;
#58012 = ORIENTED_EDGE ( 'NONE', *, *, #31847, .F. ) ;
#58013 = CARTESIAN_POINT ( 'NONE',  ( 8.160000000000000142, -2.191226316053958875E-18, 2.701633758479787833E-17 ) ) ;
#58014 = FACE_OUTER_BOUND ( 'NONE', #7844, .T. ) ;
#58015 = PLANE ( 'NONE',  #31285 ) ;
#58016 = CARTESIAN_POINT ( 'NONE',  ( -76.52287095715007581, -23.47593901973090169, -1.443836447538996648 ) ) ;
#58017 = LINE ( 'NONE', #27557, #17496 ) ;
#58018 = CARTESIAN_POINT ( 'NONE',  ( 32.98733314340959311, 5.965225279485572685, 2.074222136288530027 ) ) ;
#58019 = CARTESIAN_POINT ( 'NONE',  ( -114.5206646555255503, -23.73791477778912196, 11.05961554403169700 ) ) ;
#58020 = CARTESIAN_POINT ( 'NONE',  ( 12.75013301566243129, -15.34773647900153115, 11.49999999999998934 ) ) ;
#58021 = CARTESIAN_POINT ( 'NONE',  ( -0.03132738354372287259, -22.64444240169225253, 8.124201566845400180 ) ) ;
#58022 = CARTESIAN_POINT ( 'NONE',  ( -0.2410636032128395945, 19.88167143085883737, -1.500000000000002220 ) ) ;
#58023 = ORIENTED_EDGE ( 'NONE', *, *, #52984, .T. ) ;
#58024 = VECTOR ( 'NONE', #93636, 1000.000000000000000 ) ;
#58025 = DIRECTION ( 'NONE',  ( -3.773278334453079618E-23, 0.9999999999976377785, 2.173523156925979975E-06 ) ) ;
#58026 = EDGE_CURVE ( 'NONE', #17009, #60699, #52997, .T. ) ;
#58027 = CARTESIAN_POINT ( 'NONE',  ( -70.52287095715007581, -23.48783264082477018, -1.443836473390089914 ) ) ;
#58028 = CARTESIAN_POINT ( 'NONE',  ( 5.548031177074126852, -6.376774720514426953, -25.42222224686167920 ) ) ;
#58029 = CARTESIAN_POINT ( 'NONE',  ( 5.171613189315443115, 20.13430294385436881, 11.49999999999999645 ) ) ;
#58030 = CARTESIAN_POINT ( 'NONE',  ( -7.491187506528125262, -6.376774720514410077, 19.53857357749109980 ) ) ;
#58031 = B_SPLINE_CURVE_WITH_KNOTS ( 'NONE', 3,
 ( #90667, #91162, #13529, #75426 ),
 .UNSPECIFIED., .F., .F.,
 ( 4, 4 ),
 ( 0.8611149010728148534, 0.8701213323449306092 ),
 .UNSPECIFIED. ) ;
#58032 = PLANE ( 'NONE',  #20980 ) ;
#58033 = CARTESIAN_POINT ( 'NONE',  ( -7.756741253720922380, -21.46081514045699024, 11.49999999999999645 ) ) ;
#58034 = EDGE_LOOP ( 'NONE', ( #35003, #93219, #61571, #16075 ) ) ;
#58035 = B_SPLINE_SURFACE_WITH_KNOTS ( 'NONE', 3, 1, ( 
 ( #68620, #20935 ),
 ( #60025, #82836 ),
 ( #45290, #38155 ),
 ( #14315, #14815 ),
 ( #53405, #6212 ),
 ( #7205, #21425 ),
 ( #37171, #44296 ),
 ( #69108, #20430 ),
 ( #67146, #68128 ),
 ( #29549, #67633 ),
 ( #44792, #28550 ),
 ( #99050, #74721 ),
 ( #100037, #61521 ),
 ( #36178, #30041 ),
 ( #60527, #91440 ),
 ( #13317, #84329 ),
 ( #51403, #99543 ),
 ( #75225, #52399 ),
 ( #21923, #76215 ) ),
 .UNSPECIFIED., .F., .F., .F.,
 ( 4, 1, 1, 1, 1, 1, 1, 1, 1, 1, 1, 1, 1, 1, 1, 1, 4 ),
 ( 2, 2 ),
 ( 0.000000000000000000, 0.07563486594245749650, 0.1456749912579856643, 0.2101933844674982454, 0.2691971886348943910, 0.3228467966362091879, 0.3711350468222357479, 0.4143602045761037855, 0.4526539356929054625, 0.5231868047418553047, 0.5919172609462786117, 0.6599757056395090249, 0.7292117337225374474, 0.7981350023964016716, 0.8652933977976429158, 0.9318417558440025283, 1.000000000000000000 ),
 ( 0.000000000000000000, 1.000000000000000000 ),
 .UNSPECIFIED. ) ;
#58036 = CARTESIAN_POINT ( 'NONE',  ( -29.49875734969025842, 5.965225279485572685, 15.62202280011862321 ) ) ;
#58037 = DIRECTION ( 'NONE',  ( 0.000000000000000000, -2.173523156925980399E-06, 0.9999999999976378895 ) ) ;
#58038 = ORIENTED_EDGE ( 'NONE', *, *, #75686, .F. ) ;
#58039 = ADVANCED_FACE ( 'NONE', ( #73205 ), #6141, .T. ) ;
#58040 = CARTESIAN_POINT ( 'NONE',  ( 3.706880958665978998, 19.89330832657401515, 11.49999999999998934 ) ) ;
#58041 = CARTESIAN_POINT ( 'NONE',  ( 6.698292889820671725, -6.376774720514424288, 21.80822233811499444 ) ) ;
#58042 = PLANE ( 'NONE',  #43684 ) ;
#58043 = ADVANCED_FACE ( 'NONE', ( #52355 ), #73339, .T. ) ;
#58044 = DIRECTION ( 'NONE',  ( 4.335561085774420994E-16, 0.000000000000000000, -1.000000000000000000 ) ) ;
#58045 = EDGE_CURVE ( 'NONE', #77563, #34509, #61970, .T. ) ;
#58046 = EDGE_LOOP ( 'NONE', ( #88041, #11957, #77338, #36245, #17691, #53967, #8637 ) ) ;
#58047 = CARTESIAN_POINT ( 'NONE',  ( -79.34850868052345163, -25.28330624484387101, 5.890934297546558618 ) ) ;
#58048 = CARTESIAN_POINT ( 'NONE',  ( 0.3910256410256441884, -6.376774720514427841, 21.75000000000000000 ) ) ;
#58049 = CARTESIAN_POINT ( 'NONE',  ( -16.07871291144651593, -12.00523380332558965, -1.500000000000002220 ) ) ;
#58050 = EDGE_CURVE ( 'NONE', #72919, #29476, #22870, .T. ) ;
#58051 = CARTESIAN_POINT ( 'NONE',  ( 19.40125262130244366, -8.172613994405130811, 11.49999999999999645 ) ) ;
#58052 = CARTESIAN_POINT ( 'NONE',  ( -50.40895856474225667, -29.50249942614373921, 7.563164501610022405 ) ) ;
#58053 = FACE_OUTER_BOUND ( 'NONE', #23958, .T. ) ;
#58054 = CARTESIAN_POINT ( 'NONE',  ( 18.22792733936863030, -12.41963300964812156, 11.49999999999998934 ) ) ;
#58055 = ADVANCED_FACE ( 'NONE', ( #92897 ), #84788, .T. ) ;
#58056 = VECTOR ( 'NONE', #89957, 1000.000000000000000 ) ;
#58057 = CARTESIAN_POINT ( 'NONE',  ( -39.59566294291796140, -25.31589243397437627, 4.684364548415942409 ) ) ;
#58058 = LINE ( 'NONE', #10359, #46790 ) ;
#58059 = DIRECTION ( 'NONE',  ( -0.000000000000000000, -1.000000000000000000, -0.000000000000000000 ) ) ;
#58060 = DIRECTION ( 'NONE',  ( 0.000000000000000000, 0.9999999999976377785, 2.173523156925979128E-06 ) ) ;
#58061 = CARTESIAN_POINT ( 'NONE',  ( -4.209565145052936330, 8.865772972990910716, 1.700000000000008837 ) ) ;
#58062 = ORIENTED_EDGE ( 'NONE', *, *, #72494, .T. ) ;
#58063 = VECTOR ( 'NONE', #66031, 1000.000000000000114 ) ;
#58064 = ORIENTED_EDGE ( 'NONE', *, *, #10891, .F. ) ;
#58065 = CARTESIAN_POINT ( 'NONE',  ( -41.62287095715006302, -23.48786465467240703, 11.44779295918255180 ) ) ;
#58066 = CARTESIAN_POINT ( 'NONE',  ( -30.47287095715007510, -29.50248298729120222, -6.412432995908637812E-05 ) ) ;
#58068 = EDGE_CURVE ( 'NONE', #71712, #39562, #31918, .T. ) ;
#58067 = CARTESIAN_POINT ( 'NONE',  ( -58.62287095715006302, -24.51283580621364067, 0.6167428607019806996 ) ) ;
#58069 = CARTESIAN_POINT ( 'NONE',  ( 15.34425395324244867, 13.73259486114767114, -1.500000000000002220 ) ) ;
#58070 = CARTESIAN_POINT ( 'NONE',  ( 0.7969447072908428797, -21.54811710690876225, 11.49999999999999645 ) ) ;
#58071 = ORIENTED_EDGE ( 'NONE', *, *, #7092, .F. ) ;
#58072 = DIRECTION ( 'NONE',  ( 0.000000000000000000, 0.000000000000000000, 1.000000000000000000 ) ) ;
#58073 = CARTESIAN_POINT ( 'NONE',  ( 7.164391295225654765, -5.876774720514420736, 20.71606273170883838 ) ) ;
#58074 = DIRECTION ( 'NONE',  ( 0.000000000000000000, -1.000000000000000000, 0.000000000000000000 ) ) ;
#58075 = CARTESIAN_POINT ( 'NONE',  ( 8.793911523065595759, -20.50603677605392150, 11.49999999999998934 ) ) ;
#58076 = LINE ( 'NONE', #74278, #49699 ) ;
#58077 = CARTESIAN_POINT ( 'NONE',  ( 25.05730599792488533, 1.684774720501991174, -18.59674224247030239 ) ) ;
#58078 = ORIENTED_EDGE ( 'NONE', *, *, #27449, .F. ) ;
#58079 = DIRECTION ( 'NONE',  ( 1.000000000000000000, 0.000000000000000000, 0.000000000000000000 ) ) ;
#58080 = CARTESIAN_POINT ( 'NONE',  ( -51.04357394935764347, -25.30543060587211812, 4.940877950953177056 ) ) ;
#58081 = VECTOR ( 'NONE', #85958, 1000.000000000000114 ) ;
#58082 = CARTESIAN_POINT ( 'NONE',  ( 18.76864855846692492, -9.085702381504452418, -1.500000000000002220 ) ) ;
#58083 = ORIENTED_EDGE ( 'NONE', *, *, #40823, .T. ) ;
#58085 = ORIENTED_EDGE ( 'NONE', *, *, #31445, .T. ) ;
#58084 = CARTESIAN_POINT ( 'NONE',  ( 14.85834502026402681, -3.582999323269832725, -27.37203305628894867 ) ) ;
#58086 = EDGE_LOOP ( 'NONE', ( #3625, #10651, #4736, #19302 ) ) ;
#58087 = CARTESIAN_POINT ( 'NONE',  ( -50.44234050327818153, -25.30264421209000858, 4.735024738193449600 ) ) ;
#58088 = CARTESIAN_POINT ( 'NONE',  ( 4.297136154115697160, 20.59472113332480703, -1.500000000000002220 ) ) ;
#58089 = ORIENTED_EDGE ( 'NONE', *, *, #12527, .T. ) ;
#58090 = CARTESIAN_POINT ( 'NONE',  ( -28.98875734969026041, -3.316774720514426456, -0.08597719988137648983 ) ) ;
#58091 = DIRECTION ( 'NONE',  ( 0.9685340172660600322, 0.000000000000000000, -0.2488812114211667037 ) ) ;
#58092 = CARTESIAN_POINT ( 'NONE',  ( -120.6253516754611610, -24.52399227489125266, 9.353111116836528183 ) ) ;
#58093 = CARTESIAN_POINT ( 'NONE',  ( -76.55010092559956547, -24.15620529776628089, 10.23563542870660470 ) ) ;
#58094 = DIRECTION ( 'NONE',  ( 0.000000000000000000, -1.000000000000000000, 0.000000000000000000 ) ) ;
#58095 = CARTESIAN_POINT ( 'NONE',  ( -10.76533847658563126, -18.86179312034942868, -1.500000000000002220 ) ) ;
#58096 = CARTESIAN_POINT ( 'NONE',  ( -97.62287095715005592, -24.64965695001468404, 8.947790433994178727 ) ) ;
#58098 = VERTEX_POINT ( 'NONE', #37119 ) ;
#58097 = CARTESIAN_POINT ( 'NONE',  ( 18.30470771955606679, 12.64531542519679697, 11.49999999999999645 ) ) ;
#58099 = CARTESIAN_POINT ( 'NONE',  ( 19.24418710706453339, 0.000000000000000000, 2.346898003627108320 ) ) ;
#58100 = CARTESIAN_POINT ( 'NONE',  ( 7.164391295225654765, -6.376774720514420736, 20.71606273170883838 ) ) ;
#58101 = EDGE_CURVE ( 'NONE', #81001, #32994, #51672, .T. ) ;
#58102 = CARTESIAN_POINT ( 'NONE',  ( -106.5228709571500758, -24.64965694238408034, 8.947790433994192938 ) ) ;
#58103 = ORIENTED_EDGE ( 'NONE', *, *, #18529, .T. ) ;
#58105 = ORIENTED_EDGE ( 'NONE', *, *, #66769, .F. ) ;
#58104 = CARTESIAN_POINT ( 'NONE',  ( -36.52287095715006870, -23.47596703998600631, 11.44779298504229281 ) ) ;
#58106 = EDGE_CURVE ( 'NONE', #42444, #42079, #13849, .T. ) ;
#58107 = VERTEX_POINT ( 'NONE', #14267 ) ;
#58108 = DIRECTION ( 'NONE',  ( 0.9890158633619159367, 0.1478094111296165969, 0.000000000000000000 ) ) ;
#58109 = EDGE_CURVE ( 'NONE', #10587, #3669, #73425, .T. ) ;
#58110 = DIRECTION ( 'NONE',  ( -3.773278334453079618E-23, 0.9999999999976377785, 2.173523156925979975E-06 ) ) ;
#58111 = CARTESIAN_POINT ( 'NONE',  ( 31.27206728860909024, 4.132774720514318822, -3.930752063305056332 ) ) ;
#58112 = EDGE_CURVE ( 'NONE', #67290, #16727, #45243, .T. ) ;
#58113 = CARTESIAN_POINT ( 'NONE',  ( -126.5228709571500048, -23.95044443724992789, 10.65354141964648882 ) ) ;
#58114 = VERTEX_POINT ( 'NONE', #49262 ) ;
#58115 = CARTESIAN_POINT ( 'NONE',  ( -130.5728709571500303, -24.76085724621141182, 8.931194175204877794 ) ) ;
#58116 = CARTESIAN_POINT ( 'NONE',  ( 6.846561153812083411, -21.39451737393737574, -1.500000000000002220 ) ) ;
#58117 = VERTEX_POINT ( 'NONE', #48755 ) ;
#58118 = CARTESIAN_POINT ( 'NONE',  ( -86.52287095715006160, -29.50250243563736774, 8.947779886222139822 ) ) ;
#58119 = DIRECTION ( 'NONE',  ( 0.000000000000000000, 0.6401843996644797086, -0.7682212795973759611 ) ) ;
#58120 = CARTESIAN_POINT ( 'NONE',  ( 9.214646252596866205, 5.356774720515496746, -27.04520690447069597 ) ) ;
#58121 = LINE ( 'NONE', #17537, #77329 ) ;
#58122 = CARTESIAN_POINT ( 'NONE',  ( -130.5728709571500588, -25.14081846633249384, 7.291654623549831626 ) ) ;
#58123 = CARTESIAN_POINT ( 'NONE',  ( 0.9049686737998731134, -19.58615294826029540, 11.49999999999998934 ) ) ;
#58124 = CARTESIAN_POINT ( 'NONE',  ( -50.17515359291254384, -25.31218963190688953, 4.714858780549761264 ) ) ;
#58125 = ORIENTED_EDGE ( 'NONE', *, *, #48241, .T. ) ;
#58126 = CARTESIAN_POINT ( 'NONE',  ( -18.46100929034391314, -11.06139713797464985, -1.500000000000002220 ) ) ;
#58127 = CARTESIAN_POINT ( 'NONE',  ( 15.97264540888995299, -3.316774720514426456, -27.93485543958162154 ) ) ;
#58128 = CARTESIAN_POINT ( 'NONE',  ( -71.30376622360817862, -25.25639414126157689, 6.239614501453647932 ) ) ;
#58129 = CARTESIAN_POINT ( 'NONE',  ( -101.6833297298926055, -25.24379662554390436, 3.680570895106967999 ) ) ;
#58130 = CARTESIAN_POINT ( 'NONE',  ( -4.926336369345162502, 0.3587747205143967943, -28.61095484066305161 ) ) ;
#58131 = CARTESIAN_POINT ( 'NONE',  ( -22.63010559926462051, 4.001702944626347680, -1.500000000000002220 ) ) ;
#58132 = CC_DESIGN_PERSON_AND_ORGANIZATION_ASSIGNMENT ( #15296, #31026, ( #63621 ) ) ;
#58133 = DATE_AND_TIME ( #99156, #6804 ) ;
#58134 = CARTESIAN_POINT ( 'NONE',  ( -0.02075734969026423599, -3.316774720514426456, -0.08597719988137648983 ) ) ;
#58135 = CARTESIAN_POINT ( 'NONE',  ( -49.54717124518386129, -24.15543982623906771, -0.2315651400026657036 ) ) ;
#58136 = CARTESIAN_POINT ( 'NONE',  ( 20.09017895974002599, 0.4902201509063087159, 11.49999999999999645 ) ) ;
#58137 = CARTESIAN_POINT ( 'NONE',  ( 22.81105451610979173, -4.772774720514425972, -18.46691820600746681 ) ) ;
#58138 = CARTESIAN_POINT ( 'NONE',  ( -32.57491724666229516, -24.66019654487198665, 8.947790411086131712 ) ) ;
#58139 = DIRECTION ( 'NONE',  ( -0.000000000000000000, -1.000000000000000000, -0.000000000000000000 ) ) ;
#58140 = CARTESIAN_POINT ( 'NONE',  ( -79.52287095715006160, -24.64898659630367916, 1.056161002820826145 ) ) ;
#58141 = FACE_OUTER_BOUND ( 'NONE', #88125, .T. ) ;
#58142 = CARTESIAN_POINT ( 'NONE',  ( -5.703961651189128901, -19.02375728206049743, 11.49999999999998934 ) ) ;
#58143 = CARTESIAN_POINT ( 'NONE',  ( -113.5585636484403267, -23.48783264082477373, -1.443836473390084807 ) ) ;
#58144 = CARTESIAN_POINT ( 'NONE',  ( 13.13437215454093199, 14.66711140016434278, -1.500000000000002220 ) ) ;
#58145 = FACE_OUTER_BOUND ( 'NONE', #15516, .T. ) ;
#58146 = VECTOR ( 'NONE', #42195, 1000.000000000000000 ) ;
#58147 = CARTESIAN_POINT ( 'NONE',  ( -15.87499999999997868, 2.877919977996279334E-16, -2.349999999999999645 ) ) ;
#58148 = DIRECTION ( 'NONE',  ( 0.000000000000000000, 1.000000000000000000, 0.000000000000000000 ) ) ;
#58149 = CARTESIAN_POINT ( 'NONE',  ( 1.647368763193059582, 20.57021071130147405, 11.49999999999999645 ) ) ;
#58150 = CARTESIAN_POINT ( 'NONE',  ( -42.62287095715003460, -24.51283580621364422, 0.6167428607019693754 ) ) ;
#58151 = CARTESIAN_POINT ( 'NONE',  ( -2.225104987405961854, -22.55768739424384606, 11.49999999999999645 ) ) ;
#58152 = ORIENTED_EDGE ( 'NONE', *, *, #8238, .F. ) ;
#58153 = FACE_OUTER_BOUND ( 'NONE', #8884, .T. ) ;
#58154 = CARTESIAN_POINT ( 'NONE',  ( -56.52287095715006870, -24.65952944569304606, 1.056160979905695463 ) ) ;
#58155 = EDGE_CURVE ( 'NONE', #99976, #68399, #94907, .T. ) ;
#58156 = CARTESIAN_POINT ( 'NONE',  ( -27.40807623642065494, -24.93063630324751045, 8.230615498763011573 ) ) ;
#58157 = LINE ( 'NONE', #66278, #4243 ) ;
#58158 = ORIENTED_EDGE ( 'NONE', *, *, #23821, .T. ) ;
#58159 = VERTEX_POINT ( 'NONE', #79682 ) ;
#58160 = CARTESIAN_POINT ( 'NONE',  ( 0.1645010273463769490, 0.3687607960183755251, -1.417169167140624575 ) ) ;
#58161 = CARTESIAN_POINT ( 'NONE',  ( -18.82434810282327220, -12.99595988342530362, -1.500000000000002220 ) ) ;
#58162 = DIRECTION ( 'NONE',  ( -1.000000000000000000, 0.000000000000000000, 0.000000000000000000 ) ) ;
#58163 = CARTESIAN_POINT ( 'NONE',  ( 20.07693369621832602, 7.961103810760662647, -1.500000000000002220 ) ) ;
#58164 = CARTESIAN_POINT ( 'NONE',  ( -37.52287095715006870, -24.64965694238406613, 8.947790433994205372 ) ) ;
#58165 = DIRECTION ( 'NONE',  ( 0.000000000000000000, 0.000000000000000000, -1.000000000000000000 ) ) ;
#58166 = EDGE_CURVE ( 'NONE', #19170, #97996, #64497, .T. ) ;
#58167 = CARTESIAN_POINT ( 'NONE',  ( -0.2110286175373513040, -22.56517410205234597, 11.49999999999999645 ) ) ;
#58168 = ORIENTED_EDGE ( 'NONE', *, *, #50345, .F. ) ;
#58169 = CARTESIAN_POINT ( 'NONE',  ( -89.81226385320384509, -25.06732983082694943, 7.447789526168956620 ) ) ;
#58170 = CARTESIAN_POINT ( 'NONE',  ( 19.17116566557315949, -10.70166234769870961, -1.500000000000002220 ) ) ;
#58171 = EDGE_CURVE ( 'NONE', #71061, #12190, #3080, .T. ) ;
#58172 = CARTESIAN_POINT ( 'NONE',  ( -17.97250661212648026, 0.3587747205144057872, -23.43622901028613725 ) ) ;
#58173 = CARTESIAN_POINT ( 'NONE',  ( -4.141025641025638748, -5.876774720514426953, 21.75000000000000355 ) ) ;
#58174 = EDGE_LOOP ( 'NONE', ( #60091, #38367, #17241, #81357 ) ) ;
#58175 = CARTESIAN_POINT ( 'NONE',  ( -89.62287095715007013, -24.35013146730204525, 9.818937971375106599 ) ) ;
#58176 = CARTESIAN_POINT ( 'NONE',  ( -47.52287095715006160, -23.47596703998600631, 11.44779298504229104 ) ) ;
#58177 = ORIENTED_EDGE ( 'NONE', *, *, #48419, .F. ) ;
#58178 = DIRECTION ( 'NONE',  ( -3.773278334453079030E-23, 0.9999999999976377785, 2.173523156925979128E-06 ) ) ;
#58179 = VERTEX_POINT ( 'NONE', #40128 ) ;
#58180 = AXIS2_PLACEMENT_3D ( 'NONE', #78855, #17977, #57557 ) ;
#58181 = ORIENTED_EDGE ( 'NONE', *, *, #22674, .F. ) ;
#58182 = ORIENTED_EDGE ( 'NONE', *, *, #65379, .F. ) ;
#58183 = CARTESIAN_POINT ( 'NONE',  ( -20.27875734969026311, -6.143225279485574397, 24.00402280011862288 ) ) ;
#58184 = CARTESIAN_POINT ( 'NONE',  ( -70.62287095715005592, -29.50247984919015209, -1.443849546365055359 ) ) ;
#58186 = EDGE_CURVE ( 'NONE', #80701, #25971, #7983, .T. ) ;
#58185 = CARTESIAN_POINT ( 'NONE',  ( 0.03625801282051022839, -5.876774720514410077, 19.27714342948718240 ) ) ;
#58187 = CARTESIAN_POINT ( 'NONE',  ( -10.90597124047809530, 17.21661415904998904, -1.500000000000002220 ) ) ;
#58188 = VERTEX_POINT ( 'NONE', #39619 ) ;
#58189 = CARTESIAN_POINT ( 'NONE',  ( 8.160000000000000142, -10.65233964170348635, -1.203735189656879756 ) ) ;
#58190 = AXIS2_PLACEMENT_3D ( 'NONE', #36455, #28342, #68412 ) ;
#58191 = CARTESIAN_POINT ( 'NONE',  ( -92.52287095715010423, -23.73934037231756733, 11.05740245334328620 ) ) ;
#58192 = CARTESIAN_POINT ( 'NONE',  ( -105.5074323697901377, -25.00158670708910691, 2.256160236439218369 ) ) ;
#58193 = CARTESIAN_POINT ( 'NONE',  ( -57.52287095715003318, -23.48783264082476663, -1.443836473390093911 ) ) ;
#58194 = EDGE_LOOP ( 'NONE', ( #75790, #55711, #39, #81250 ) ) ;
#58195 = FACE_OUTER_BOUND ( 'NONE', #52907, .T. ) ;
#58196 = CARTESIAN_POINT ( 'NONE',  ( -89.92287095715005307, -23.47593901973090524, -1.443836447538996870 ) ) ;
#58197 = VERTEX_POINT ( 'NONE', #40635 ) ;
#58198 = VECTOR ( 'NONE', #80475, 1000.000000000000114 ) ;
#58199 = CARTESIAN_POINT ( 'NONE',  ( -13.51810693421681719, -15.76408947421354156, 11.49999999999998934 ) ) ;
#58200 = EDGE_LOOP ( 'NONE', ( #76391, #27386 ) ) ;
#58202 = VERTEX_POINT ( 'NONE', #16782 ) ;
#58201 = CARTESIAN_POINT ( 'NONE',  ( -31.52287095715006160, -23.48786465467240347, 11.44779295918255357 ) ) ;
#58203 = DIRECTION ( 'NONE',  ( -3.773278334453080206E-23, 0.9999999999976377785, 2.173523156925979975E-06 ) ) ;
#58204 = CYLINDRICAL_SURFACE ( 'NONE', #71365, 27.94799999999999685 ) ;
#58205 = ORIENTED_EDGE ( 'NONE', *, *, #80201, .F. ) ;
#58206 = VERTEX_POINT ( 'NONE', #87805 ) ;
#58207 = CARTESIAN_POINT ( 'NONE',  ( -88.52287095715006160, -24.65952944569304606, 1.056160979905700570 ) ) ;
#58208 = AXIS2_PLACEMENT_3D ( 'NONE', #96838, #26335, #12093 ) ;
#58209 = CARTESIAN_POINT ( 'NONE',  ( 9.566520649354789185, 3.316774720514426011, -27.03026789950428110 ) ) ;
#58210 = CARTESIAN_POINT ( 'NONE',  ( -52.62287095715005592, -23.73934037231757088, 11.05740245334329153 ) ) ;
#58212 = EDGE_CURVE ( 'NONE', #46960, #15342, #44300, .T. ) ;
#58211 = CARTESIAN_POINT ( 'NONE',  ( -70.97512524164069703, -25.31201633795301831, 5.512439363672202219 ) ) ;
#58214 = ORIENTED_EDGE ( 'NONE', *, *, #10309, .T. ) ;
#58213 = CARTESIAN_POINT ( 'NONE',  ( 20.57361055066190758, -8.084994430987380909, 11.49999999999999645 ) ) ;
#58215 = CARTESIAN_POINT ( 'NONE',  ( -108.6313998591546550, -23.73766607897671932, -1.055555164236429366 ) ) ;
#58216 = CARTESIAN_POINT ( 'NONE',  ( 22.48748499206561746, 2.281147167042596013, 11.49999999999998934 ) ) ;
#58218 = ORIENTED_EDGE ( 'NONE', *, *, #987, .T. ) ;
#58217 = CARTESIAN_POINT ( 'NONE',  ( -46.52287095715006870, -24.51387760970725083, 9.387446482453420060 ) ) ;
#58219 = EDGE_CURVE ( 'NONE', #58835, #56230, #46811, .T. ) ;
#58220 = VERTEX_POINT ( 'NONE', #1576 ) ;
#58221 = CARTESIAN_POINT ( 'NONE',  ( 33.74607884027702909, -0.3587747205144265483, -4.999864028243830916 ) ) ;
#58222 = B_SPLINE_CURVE_WITH_KNOTS ( 'NONE', 3,
 ( #45639, #37522, #15680, #8069 ),
 .UNSPECIFIED., .F., .F.,
 ( 4, 4 ),
 ( 0.000000000000000000, 1.000000000000000000 ),
 .UNSPECIFIED. ) ;
#58223 = ADVANCED_FACE ( 'NONE', ( #94407 ), #41139, .F. ) ;
#58224 = CLOSED_SHELL ( 'NONE', ( #49519, #4471, #50140, #44852, #99296, #38551, #74423, #83, #13353, #77752, #74739, #72241, #65827, #26755, #72121, #58543, #40092, #30333, #53446, #41775, #43347, #82934, #4719, #86714, #64816, #19970, #76694, #27789, #16687, #2504, #51901, #40957, #27435, #90275, #83572, #48315, #9286, #33614, #57153 ) ) ;
#58225 = EDGE_CURVE ( 'NONE', #44828, #13092, #72092, .T. ) ;
#58226 = B_SPLINE_SURFACE_WITH_KNOTS ( 'NONE', 3, 1, ( 
 ( #3615, #11704 ),
 ( #26942, #50290 ),
 ( #66034, #42685 ),
 ( #21805, #92326 ),
 ( #36048, #67023 ),
 ( #7096, #45174 ),
 ( #68501, #13194 ),
 ( #14702, #37048 ),
 ( #28427, #61403 ),
 ( #59391, #6095 ),
 ( #52782, #68008 ),
 ( #84211, #44169 ),
 ( #59904, #91329 ),
 ( #12701, #30433 ),
 ( #13698, #90334 ) ),
 .UNSPECIFIED., .F., .F., .F.,
 ( 4, 1, 1, 1, 1, 1, 1, 1, 1, 1, 1, 1, 4 ),
 ( 2, 2 ),
 ( 0.000000000000000000, 0.08968993624739593495, 0.1784940104960813789, 0.2668377532994903878, 0.3565581760610176398, 0.4453342496549802521, 0.5308058350374902368, 0.6140762174402841778, 0.6977070858228016093, 0.7791419498114620090, 0.8553535905869761313, 0.9285568200856556542, 1.000000000000000000 ),
 ( 0.000000000000000000, 1.000000000000000000 ),
 .UNSPECIFIED. ) ;
#58227 = CARTESIAN_POINT ( 'NONE',  ( -86.52287095715006160, -23.48783264083431277, -1.443836473375255336 ) ) ;
#58228 = ORIENTED_EDGE ( 'NONE', *, *, #34081, .F. ) ;
#58229 = CARTESIAN_POINT ( 'NONE',  ( -19.86647519178106691, -7.318714840676754818, 11.49999999999998934 ) ) ;
#58230 = CARTESIAN_POINT ( 'NONE',  ( 32.69168087260868560, 4.943943141208723802, -11.74984035242545133 ) ) ;
#58231 = CARTESIAN_POINT ( 'NONE',  ( -41.80321513992567617, -25.30077457980579680, 4.650809782510233248 ) ) ;
#58232 = CARTESIAN_POINT ( 'NONE',  ( -16.22183044023116238, -15.26045173261249310, -1.500000000000002220 ) ) ;
#58233 = CARTESIAN_POINT ( 'NONE',  ( 0.4325450954222598288, 0.000000000000000000, 0.000000000000000000 ) ) ;
#58234 = ORIENTED_EDGE ( 'NONE', *, *, #25901, .F. ) ;
#58235 = LINE ( 'NONE', #20642, #46517 ) ;
#58236 = CARTESIAN_POINT ( 'NONE',  ( -44.62287095715004881, -24.64898659630528854, 1.056161002820819261 ) ) ;
#58237 = CARTESIAN_POINT ( 'NONE',  ( -36.52201391965095212, -23.48786465467240347, 11.44779295918255180 ) ) ;
#58238 = LINE ( 'NONE', #10548, #40492 ) ;
#58239 = CARTESIAN_POINT ( 'NONE',  ( -3.338044803349280443, -19.22079736023769669, 11.49999999999998934 ) ) ;
#58240 = CARTESIAN_POINT ( 'NONE',  ( -4.378498130703003532, 20.98420022172975763, -1.500000000000002220 ) ) ;
#58241 = CARTESIAN_POINT ( 'NONE',  ( -0.5218785734906133955, -5.876774720514408301, 19.14848118821636547 ) ) ;
#58242 = LINE ( 'NONE', #74451, #1694 ) ;
#58243 = CARTESIAN_POINT ( 'NONE',  ( -77.53983134128570498, -24.65952944569304606, 1.056160979905701458 ) ) ;
#58244 = CARTESIAN_POINT ( 'NONE',  ( 21.74077840044056842, -6.890983112422549794, -1.500000000000002220 ) ) ;
#58245 = EDGE_CURVE ( 'NONE', #35739, #17845, #96418, .T. ) ;
#58246 = CARTESIAN_POINT ( 'NONE',  ( -102.6235476894606791, -24.65952944569305316, 1.056160979905705677 ) ) ;
#58247 = DIRECTION ( 'NONE',  ( 0.000000000000000000, 0.000000000000000000, 1.000000000000000000 ) ) ;
#58248 = CARTESIAN_POINT ( 'NONE',  ( 19.20567810191101898, 5.375360269454119155, 11.49999999999999645 ) ) ;
#58249 = CARTESIAN_POINT ( 'NONE',  ( -111.6228709571500417, -24.66019654487199730, 8.947790411086124607 ) ) ;
#58250 = EDGE_CURVE ( 'NONE', #27723, #24726, #18947, .T. ) ;
#58251 = AXIS2_PLACEMENT_3D ( 'NONE', #85972, #63661, #94583 ) ;
#58252 = CARTESIAN_POINT ( 'NONE',  ( 16.26279755680690542, 6.475225279485573360, -27.67997040356620531 ) ) ;
#58253 = CARTESIAN_POINT ( 'NONE',  ( -48.58199726423757170, -24.51314013834315375, 0.6176544820404137326 ) ) ;
#58254 = ORIENTED_EDGE ( 'NONE', *, *, #28440, .T. ) ;
#58255 = CARTESIAN_POINT ( 'NONE',  ( 29.73839433968188573, 4.772784452553388235, -4.021546701937777080 ) ) ;
#58256 = LINE ( 'NONE', #10071, #57254 ) ;
#58257 = CARTESIAN_POINT ( 'NONE',  ( 17.51545567653809954, -12.82042131148251229, 11.49999999999998934 ) ) ;
#58258 = EDGE_CURVE ( 'NONE', #1776, #94542, #17696, .T. ) ;
#58259 = CARTESIAN_POINT ( 'NONE',  ( -67.62287095715005592, -24.65952944569304606, 1.056160979905697017 ) ) ;
#58260 = AXIS2_PLACEMENT_3D ( 'NONE', #35610, #58454, #12244 ) ;
#58261 = CARTESIAN_POINT ( 'NONE',  ( 7.694069055508638399, 17.95645395709951941, -1.500000000000002220 ) ) ;
#58262 = B_SPLINE_CURVE_WITH_KNOTS ( 'NONE', 3,
 ( #17883, #25492, #63577, #63069 ),
 .UNSPECIFIED., .F., .F.,
 ( 4, 4 ),
 ( 0.000000000000000000, 9.999999999999592548E-05 ),
 .UNSPECIFIED. ) ;
#58263 = EDGE_CURVE ( 'NONE', #66289, #54444, #75054, .T. ) ;
#58264 = CARTESIAN_POINT ( 'NONE',  ( -93.52287095715006160, -24.65952944569304606, 1.056160979905700570 ) ) ;
#58265 = AXIS2_PLACEMENT_3D ( 'NONE', #47796, #23423, #64048 ) ;
#58266 = DATE_AND_TIME ( #8705, #36072 ) ;
#58267 = AXIS2_PLACEMENT_3D ( 'NONE', #21925, #52905, #14318 ) ;
#58268 = CARTESIAN_POINT ( 'NONE',  ( -69.62287095715004170, -24.50321055353805733, 9.387540953477536476 ) ) ;
#58269 = CARTESIAN_POINT ( 'NONE',  ( 5.749347661499963458, 19.61174949527739386, 11.49999999999999645 ) ) ;
#58270 = CARTESIAN_POINT ( 'NONE',  ( -49.53202264565179291, -25.29391963383437769, 5.541708595187663455 ) ) ;
#58271 = DIRECTION ( 'NONE',  ( 1.955152872784845154E-15, -1.000000000000000000, -3.740001113483016365E-15 ) ) ;
#58272 = VECTOR ( 'NONE', #22601, 1000.000000000000000 ) ;
#58273 = VERTEX_POINT ( 'NONE', #57379 ) ;
#58274 = DIRECTION ( 'NONE',  ( -1.000000000000000000, -0.000000000000000000, 0.000000000000000000 ) ) ;
#58275 = LINE ( 'NONE', #59772, #42854 ) ;
#58276 = CARTESIAN_POINT ( 'NONE',  ( 31.44230187582509117, -4.132774720514425404, -3.488634554324458570 ) ) ;
#58277 =( BOUNDED_SURFACE ( )  B_SPLINE_SURFACE ( 3, 1, ( 
 ( #85916, #7282 ),
 ( #21998, #38233 ),
 ( #69188, #18406 ),
 ( #16901, #9791 ),
 ( #40246, #39735 ),
 ( #70691, #49374 ),
 ( #79294, #95029 ),
 ( #56985, #2197 ),
 ( #95530, #26015 ),
 ( #1185, #80305 ),
 ( #55988, #3201 ),
 ( #10797, #78785 ),
 ( #65110, #48869 ),
 ( #56492, #9281 ),
 ( #64616, #63602 ),
 ( #71198, #32123 ),
 ( #87923, #33636 ),
 ( #87413, #78288 ),
 ( #41761, #96030 ),
 ( #72706, #79797 ) ),
 .UNSPECIFIED., .F., .F., .T. ) 
 B_SPLINE_SURFACE_WITH_KNOTS ( ( 4, 3, 1, 1, 3, 3, 1, 1, 3, 4 ),
 ( 2, 2 ),
 ( 0.000000000000000000, 0.1255889732084985166, 0.1669421422606964800, 0.2082953113128944156, 0.2496484803650923789, 0.7477322152634136021, 0.7890853843156119263, 0.8304385533678104725, 0.8717917224200087967, 1.000000000000000000 ),
 ( 0.000000000000000000, 1.000000000000000000 ),
 .UNSPECIFIED. ) 
 GEOMETRIC_REPRESENTATION_ITEM ( )  RATIONAL_B_SPLINE_SURFACE ( (
 ( 0.9999602609241470264, 0.9999602609241470264),
 ( 0.9987387818499366965, 0.9987387818499366965),
 ( 0.9998573533027315108, 0.9998573533027315108),
 ( 1.003315975282531802, 1.003315975282531802),
 ( 1.003315975282531802, 1.003315975282531802),
 ( 1.003315975282531802, 1.003315975282531802),
 ( 1.003315975282531802, 1.003315975282531802),
 ( 1.003315975282531802, 1.003315975282531802),
 ( 1.003315975282531802, 1.003315975282531802),
 ( 0.9773170091682806815, 0.9773170091682806815),
 ( 0.9773170091682806815, 0.9773170091682806815),
 ( 1.003315975282531802, 1.003315975282531802),
 ( 1.003315975282531802, 1.003315975282531802),
 ( 1.003315975282531802, 1.003315975282531802),
 ( 1.003315975282531802, 1.003315975282531802),
 ( 1.003315975282531802, 1.003315975282531802),
 ( 1.003315975282531802, 1.003315975282531802),
 ( 0.9997852197113853423, 0.9997852197113853423),
 ( 0.9986931415022445302, 0.9986931415022445302),
 ( 1.000039740655109810, 1.000039740655109810) ) ) 
 REPRESENTATION_ITEM ( '' )  SURFACE ( )  );
#58278 = EDGE_CURVE ( 'NONE', #80473, #38812, #61387, .T. ) ;
#58279 = CARTESIAN_POINT ( 'NONE',  ( -109.5507803029036182, -24.51314013834315375, 0.6176544820404177294 ) ) ;
#58280 = ORIENTED_EDGE ( 'NONE', *, *, #98096, .F. ) ;
#58281 = LINE ( 'NONE', #97817, #17204 ) ;
#58282 = CARTESIAN_POINT ( 'NONE',  ( -7.281717392095591102, 21.80608952751712692, 11.49999999999999645 ) ) ;
#58283 = CARTESIAN_POINT ( 'NONE',  ( -6.081610112697643622, 21.96313418072945822, -1.500000000000002220 ) ) ;
#58284 = CARTESIAN_POINT ( 'NONE',  ( 4.931367317174526477, -6.376774720514420736, 20.61012727089847019 ) ) ;
#58285 = LINE ( 'NONE', #27324, #83596 ) ;
#58286 = CARTESIAN_POINT ( 'NONE',  ( 8.676776695296466002, 18.57322330470350735, 0.000000000000000000 ) ) ;
#58287 = CARTESIAN_POINT ( 'NONE',  ( 9.071512145086501278, 0.000000000000000000, 2.133776825740807753E-15 ) ) ;
#58288 = CARTESIAN_POINT ( 'NONE',  ( -69.84651095272120358, -25.15148347341441948, 6.994331270845397519 ) ) ;
#58289 = CARTESIAN_POINT ( 'NONE',  ( -21.08706934527708654, 5.832127334627817739, -1.500000000000002220 ) ) ;
#58290 = EDGE_CURVE ( 'NONE', #12603, #12714, #88307, .T. ) ;
#58291 = CARTESIAN_POINT ( 'NONE',  ( -61.24303308397303880, -29.50249942614373921, 7.563164501610022405 ) ) ;
#58292 = ADVANCED_FACE ( 'NONE', ( #82179, #20268, #35018 ), #68547, .T. ) ;
#58293 = CARTESIAN_POINT ( 'NONE',  ( -28.62287095715005947, -24.34879252677621153, 0.6165374033617160299 ) ) ;
#58294 = CARTESIAN_POINT ( 'NONE',  ( -64.52287095715006160, -23.48783264082476308, -1.443836473390094355 ) ) ;
#58295 = DIRECTION ( 'NONE',  ( -3.773278334453079618E-23, 0.9999999999976377785, 2.173523156925978705E-06 ) ) ;
#58296 = ORIENTED_EDGE ( 'NONE', *, *, #39723, .T. ) ;
#58297 = CARTESIAN_POINT ( 'NONE',  ( -3.558151220431595707, 20.12126150705307381, -1.500000000000002220 ) ) ;
#58298 = ORIENTED_EDGE ( 'NONE', *, *, #77713, .T. ) ;
#58299 = VERTEX_POINT ( 'NONE', #11178 ) ;
#58300 = ORIENTED_EDGE ( 'NONE', *, *, #63852, .T. ) ;
#58301 = ORIENTED_EDGE ( 'NONE', *, *, #58936, .F. ) ;
#58302 = CARTESIAN_POINT ( 'NONE',  ( -21.58539018223340022, -8.019882488244659768, 11.49999999999998934 ) ) ;
#58304 = EDGE_CURVE ( 'NONE', #32034, #74478, #66494, .T. ) ;
#58303 = CARTESIAN_POINT ( 'NONE',  ( 8.071512145086499501, -1.028487854913504362, 3.749999999999999556 ) ) ;
#58305 = CARTESIAN_POINT ( 'NONE',  ( 7.141438900065890216, -18.84860497471923679, -1.500000000000002220 ) ) ;
#58306 = VERTEX_POINT ( 'NONE', #26900 ) ;
#58307 = DIRECTION ( 'NONE',  ( -0.9994733861282923959, 0.000000000000000000, -0.03244919754393515293 ) ) ;
#58308 = FACE_OUTER_BOUND ( 'NONE', #66533, .T. ) ;
#58309 = EDGE_CURVE ( 'NONE', #4364, #95881, #43629, .T. ) ;
#58310 = DIRECTION ( 'NONE',  ( -3.773278334453079030E-23, 0.9999999999976377785, 2.173523156925979128E-06 ) ) ;
#58311 = PLANE ( 'NONE',  #2648 ) ;
#58313 = ORIENTED_EDGE ( 'NONE', *, *, #61834, .F. ) ;
#58312 = CARTESIAN_POINT ( 'NONE',  ( -17.73838780825237649, 11.93509662624355450, 11.49999999999999645 ) ) ;
#58314 = LINE ( 'NONE', #71146, #12811 ) ;
#58315 = EDGE_LOOP ( 'NONE', ( #7180, #94261, #16123, #8336, #89326, #52791, #1932, #42632 ) ) ;
#58316 = CARTESIAN_POINT ( 'NONE',  ( 20.70802603420765564, 8.137917507125113303, 11.49999999999998934 ) ) ;
#58317 = CARTESIAN_POINT ( 'NONE',  ( -16.33875328525262560, 12.67428768300982256, 11.49999999999998934 ) ) ;
#58318 = VECTOR ( 'NONE', #44451, 1000.000000000000000 ) ;
#58319 = ORIENTED_EDGE ( 'NONE', *, *, #99229, .T. ) ;
#58320 = CARTESIAN_POINT ( 'NONE',  ( 3.559170184186323915, -5.876774720514403860, 18.55412939673608719 ) ) ;
#58321 = ORIENTED_EDGE ( 'NONE', *, *, #23539, .T. ) ;
#58322 = DIRECTION ( 'NONE',  ( 0.1489078231574191002, 0.000000000000000000, -0.9888510809027407644 ) ) ;
#58323 = VECTOR ( 'NONE', #10367, 1000.000000000000000 ) ;
#58324 = ORIENTED_EDGE ( 'NONE', *, *, #63219, .F. ) ;
#58325 = CARTESIAN_POINT ( 'NONE',  ( 6.620851319379956301, -3.316774720514426011, -27.30756699305372592 ) ) ;
#58326 = CARTESIAN_POINT ( 'NONE',  ( -9.975069251262826953, -18.38325097723136992, -1.500000000000002220 ) ) ;
#58327 = CARTESIAN_POINT ( 'NONE',  ( 15.24057855588860377, 15.72025634131890470, 11.49999999999999645 ) ) ;
#58328 = CARTESIAN_POINT ( 'NONE',  ( -26.71877946146332050, -24.77993706282625297, 7.184564732929184849 ) ) ;
#58329 = CARTESIAN_POINT ( 'NONE',  ( 3.368619518803146029, -22.26131067175759881, 11.49999999999998934 ) ) ;
#58330 = CIRCLE ( 'NONE', #93941, 1.500000000000001332 ) ;
#58331 = CARTESIAN_POINT ( 'NONE',  ( -2.499008156623981236, -20.81284420272260860, -1.500000000000002220 ) ) ;
#58332 = CARTESIAN_POINT ( 'NONE',  ( -110.5228709571500900, -24.62226745350443480, 0.9660975649729556247 ) ) ;
#58333 = LINE ( 'NONE', #81660, #15595 ) ;
#58334 = CARTESIAN_POINT ( 'NONE',  ( -119.5920073095941945, -23.73791477778912551, 11.05961554403169700 ) ) ;
#58336 = ADVANCED_FACE ( 'NONE', ( #50744 ), #37759, .T. ) ;
#58335 = PLANE ( 'NONE',  #21538 ) ;
#58337 = ORIENTED_EDGE ( 'NONE', *, *, #70205, .T. ) ;
#58338 = AXIS2_PLACEMENT_3D ( 'NONE', #47436, #95603, #56562 ) ;
#58339 = ORIENTED_EDGE ( 'NONE', *, *, #55074, .T. ) ;
#58340 = CIRCLE ( 'NONE', #74545, 251.4258649670780699 ) ;
#58341 = EDGE_LOOP ( 'NONE', ( #4814, #6530 ) ) ;
#58342 = CARTESIAN_POINT ( 'NONE',  ( -44.52287095715007581, -24.35013146730204525, 9.818937971375103047 ) ) ;
#58343 = VERTEX_POINT ( 'NONE', #77054 ) ;
#58344 = AXIS2_PLACEMENT_3D ( 'NONE', #9792, #63097, #48870 ) ;
#58345 = CARTESIAN_POINT ( 'NONE',  ( 0.6623178260406717976, 21.47796536025111536, -1.500000000000002220 ) ) ;
#58346 = DIRECTION ( 'NONE',  ( 0.000000000000000000, 0.000000000000000000, -1.000000000000000000 ) ) ;
#58347 = ORIENTED_EDGE ( 'NONE', *, *, #72539, .T. ) ;
#58348 = CARTESIAN_POINT ( 'NONE',  ( -19.97109070424261645, 6.737033823242594366, 11.49999999999998934 ) ) ;
#58349 = DIRECTION ( 'NONE',  ( -0.000000000000000000, -1.000000000000000000, -0.000000000000000000 ) ) ;
#58350 = CARTESIAN_POINT ( 'NONE',  ( -52.62287095715006302, -24.65952944569304250, 1.056160979905695685 ) ) ;
#58351 = CARTESIAN_POINT ( 'NONE',  ( -8.160000000000000142, 0.000000000000000000, 0.000000000000000000 ) ) ;
#58352 = CARTESIAN_POINT ( 'NONE',  ( -101.5932192411211616, -23.96119346886880663, -0.6495511937832048055 ) ) ;
#58353 = PLANE ( 'NONE',  #98869 ) ;
#58354 = CARTESIAN_POINT ( 'NONE',  ( -19.11006845027251799, 11.06304553819242642, -1.500000000000002220 ) ) ;
#58355 = ORIENTED_EDGE ( 'NONE', *, *, #49693, .T. ) ;
#58356 = CARTESIAN_POINT ( 'NONE',  ( -81.63319337029726341, -24.15620529776628445, 10.23563542870661180 ) ) ;
#58357 = CARTESIAN_POINT ( 'NONE',  ( -65.52287095715006160, -29.50250786944525672, 11.44777988621623699 ) ) ;
#58358 = CARTESIAN_POINT ( 'NONE',  ( -78.62287095715011276, -24.35013146730204525, 9.818937971375108376 ) ) ;
#58360 = B_SPLINE_CURVE_WITH_KNOTS ( 'NONE', 3,
 ( #45011, #29770, #35528, #91659, #80693, #52610 ),
 .UNSPECIFIED., .F., .F.,
 ( 4, 2, 4 ),
 ( 6.384118696603436915E-06, 0.001386860460837369309, 0.002767336802978134953 ),
 .UNSPECIFIED. ) ;
#58359 = CARTESIAN_POINT ( 'NONE',  ( -62.60383890414039598, -23.73791477778912196, 11.05961554403171121 ) ) ;
#58361 = DIRECTION ( 'NONE',  ( 0.000000000000000000, -2.173523156925979552E-06, 0.9999999999976378895 ) ) ;
#58362 = CARTESIAN_POINT ( 'NONE',  ( 9.714863677370791706, 19.00186346016302608, -1.500000000000002220 ) ) ;
#58363 = DIRECTION ( 'NONE',  ( -3.773278334444166432E-23, 1.000000000000000000, 0.000000000000000000 ) ) ;
#58364 = CARTESIAN_POINT ( 'NONE',  ( -51.95144507529695233, -25.20650842489795451, 6.812665538484691474 ) ) ;
#58365 = CARTESIAN_POINT ( 'NONE',  ( -64.51565993021132783, -23.73791477778911840, 11.05961554403170766 ) ) ;
#58366 = CARTESIAN_POINT ( 'NONE',  ( -2.499999999999993339, 18.99999999999977618, 0.000000000000000000 ) ) ;
#58367 = CARTESIAN_POINT ( 'NONE',  ( 8.141615846073909424, -21.09679883994429161, -1.500000000000002220 ) ) ;
#58368 = ADVANCED_FACE ( 'NONE', ( #75550, #15161 ), #30892, .T. ) ;
#58369 = PLANE ( 'NONE',  #45802 ) ;
#58370 = ORIENTED_EDGE ( 'NONE', *, *, #57654, .T. ) ;
#58371 = CARTESIAN_POINT ( 'NONE',  ( -65.52287095715006160, -29.50248528299804818, 1.056150453629036701 ) ) ;
#58372 = CARTESIAN_POINT ( 'NONE',  ( -79.62361060721978845, -24.65952944569304606, 1.056160979905701902 ) ) ;
#58373 = CARTESIAN_POINT ( 'NONE',  ( -0.9724026449420489771, -19.73431249065222204, 11.49999999999999645 ) ) ;
#58374 = PLANE ( 'NONE',  #82848 ) ;
#58375 = CARTESIAN_POINT ( 'NONE',  ( -32.07722060962684196, -25.25098752628340293, 6.467533449461289941 ) ) ;
#58376 = ORIENTED_EDGE ( 'NONE', *, *, #78157, .F. ) ;
#58377 = LINE ( 'NONE', #51253, #79811 ) ;
#58378 = CARTESIAN_POINT ( 'NONE',  ( -29.66447556523817397, -24.60094274054533159, 3.393818988263333392 ) ) ;
#58380 = EDGE_CURVE ( 'NONE', #29853, #82528, #75636, .T. ) ;
#58379 = CARTESIAN_POINT ( 'NONE',  ( 9.450000000000002842, -2.000000000000001332, 18.24068255301868291 ) ) ;
#58381 = CARTESIAN_POINT ( 'NONE',  ( 18.49883484089910723, -11.16122333755292750, -1.500000000000002220 ) ) ;
#58382 = EDGE_CURVE ( 'NONE', #31584, #37593, #92782, .T. ) ;
#58383 = CARTESIAN_POINT ( 'NONE',  ( -10.75273025779354796, -5.876774720514426953, 23.03521261039436752 ) ) ;
#58384 = CARTESIAN_POINT ( 'NONE',  ( -70.55620429048339304, -25.00158670708909625, 2.256160236439166855 ) ) ;
#58385 = EDGE_CURVE ( 'NONE', #11431, #69290, #23799, .T. ) ;
#58386 = LINE ( 'NONE', #28914, #28631 ) ;
#58387 = CARTESIAN_POINT ( 'NONE',  ( 0.4987820251299121543, -0.03487823687206273449, -9.000000000000000000 ) ) ;
#58388 = CARTESIAN_POINT ( 'NONE',  ( -3.504374479207110316, 19.46862825742285708, 11.49999999999998934 ) ) ;
#58389 = VERTEX_POINT ( 'NONE', #46633 ) ;
#58390 = EDGE_CURVE ( 'NONE', #31511, #64945, #22261, .T. ) ;
#58391 = CARTESIAN_POINT ( 'NONE',  ( 13.48481281434462531, 15.16087405922196041, 11.49999999999999645 ) ) ;
#58392 = DIRECTION ( 'NONE',  ( 0.000000000000000000, 0.000000000000000000, -1.000000000000000000 ) ) ;
#58393 = VECTOR ( 'NONE', #25469, 1000.000000000000114 ) ;
#58394 = CARTESIAN_POINT ( 'NONE',  ( -29.81175120719462157, -29.50249373072461623, 4.942801737957442931 ) ) ;
#58395 = ORIENTED_EDGE ( 'NONE', *, *, #79560, .T. ) ;
#58396 = LINE ( 'NONE', #97922, #99295 ) ;
#58397 = CARTESIAN_POINT ( 'NONE',  ( 31.62974406627585466, 4.069828902950619387, 27.10097837741100335 ) ) ;
#58398 = CARTESIAN_POINT ( 'NONE',  ( -75.52287095715011844, -23.48783264082477373, -1.443836473390087694 ) ) ;
#58399 = CARTESIAN_POINT ( 'NONE',  ( -103.6228709571500985, -24.50321055353806443, 9.387540953477532923 ) ) ;
#58400 = CARTESIAN_POINT ( 'NONE',  ( -50.40445135320379677, -25.12298712672050982, 7.101635559041870494 ) ) ;
#58401 = CARTESIAN_POINT ( 'NONE',  ( 11.63622169266987783, 16.31392799894670631, 11.49999999999998934 ) ) ;
#58402 = ADVANCED_FACE ( 'NONE', ( #76057 ), #100379, .T. ) ;
#58403 = CARTESIAN_POINT ( 'NONE',  ( -54.52287095715006870, -29.50248528299804818, 1.056150453629033370 ) ) ;
#58404 = ORIENTED_EDGE ( 'NONE', *, *, #69641, .T. ) ;
#58405 = ADVANCED_FACE ( 'NONE', ( #29892 ), #44626, .F. ) ;
#58406 = VECTOR ( 'NONE', #46325, 1000.000000000000114 ) ;
#58407 = CARTESIAN_POINT ( 'NONE',  ( 33.96422015159436114, -5.965225279485572685, -7.233236000911337449 ) ) ;
#58408 = CARTESIAN_POINT ( 'NONE',  ( 22.81105451610979173, -1.475225279485572916, -18.46691820600746681 ) ) ;
#58409 = DIRECTION ( 'NONE',  ( 3.773278334444166432E-23, -1.000000000000000000, 0.000000000000000000 ) ) ;
#58410 = AXIS2_PLACEMENT_3D ( 'NONE', #51546, #91088, #35323 ) ;
#58411 = CARTESIAN_POINT ( 'NONE',  ( 30.53060340732035982, -1.477225279485574028, 19.84760796525321780 ) ) ;
#58412 = EDGE_CURVE ( 'NONE', #39929, #9188, #92288, .T. ) ;
#58413 = B_SPLINE_CURVE_WITH_KNOTS ( 'NONE', 3,
 ( #1293, #63200, #56591, #94628, #64209, #95133 ),
 .UNSPECIFIED., .F., .F.,
 ( 4, 2, 4 ),
 ( 1.570887131794176733E-05, 0.001396322306279758037, 0.002776935741241574537 ),
 .UNSPECIFIED. ) ;
#58414 = AXIS2_PLACEMENT_3D ( 'NONE', #59232, #90177, #51623 ) ;
#58415 = CARTESIAN_POINT ( 'NONE',  ( 15.50761710536933080, 3.593805972274664029, -28.23039328495952915 ) ) ;
#58416 = VECTOR ( 'NONE', #87617, 1000.000000000000000 ) ;
#58417 = CARTESIAN_POINT ( 'NONE',  ( -50.78266031332166364, -25.23256535379771037, 6.480020017899467355 ) ) ;
#58418 = ORIENTED_EDGE ( 'NONE', *, *, #13033, .F. ) ;
#58419 = CARTESIAN_POINT ( 'NONE',  ( -9.641467040090685003, 17.89903724589931855, -1.500000000000002220 ) ) ;
#58420 = ORIENTED_EDGE ( 'NONE', *, *, #81394, .F. ) ;
#58421 = CARTESIAN_POINT ( 'NONE',  ( -12.73177969873712279, -19.06072230859735939, -1.500000000000002220 ) ) ;
#58422 = EDGE_CURVE ( 'NONE', #71923, #30845, #76547, .T. ) ;
#58423 = CARTESIAN_POINT ( 'NONE',  ( -32.62929916188119250, -24.51314013834315375, 0.6176544820404111791 ) ) ;
#58424 = ORIENTED_EDGE ( 'NONE', *, *, #66541, .T. ) ;
#58425 = CARTESIAN_POINT ( 'NONE',  ( -108.5228709571501184, -23.96177878511310055, 10.65340807706329684 ) ) ;
#58426 = EDGE_CURVE ( 'NONE', #61060, #75155, #85176, .T. ) ;
#58427 = CARTESIAN_POINT ( 'NONE',  ( -49.51155500790866171, -25.12215341870864194, 6.743855441649687421 ) ) ;
#58428 = CARTESIAN_POINT ( 'NONE',  ( -74.52287095715007581, -23.47593901973090169, -1.443836447538996870 ) ) ;
#58429 = CARTESIAN_POINT ( 'NONE',  ( 12.09327641706010326, 17.40255341615222306, 11.49999999999999645 ) ) ;
#58430 = CARTESIAN_POINT ( 'NONE',  ( 15.99899278244174639, -15.33069297701436184, 11.49999999999998934 ) ) ;
#58431 = CARTESIAN_POINT ( 'NONE',  ( 19.85042311639309531, 5.490197614093233369, 11.49999999999998934 ) ) ;
#58432 = VERTEX_POINT ( 'NONE', #38007 ) ;
#58433 = CARTESIAN_POINT ( 'NONE',  ( -43.52287095715005449, -23.72747288104469732, -1.053458166803227680 ) ) ;
#58434 = ORIENTED_EDGE ( 'NONE', *, *, #75831, .F. ) ;
#58435 = CARTESIAN_POINT ( 'NONE',  ( 6.887358010905132666, -6.376774720514426065, 21.32574817943157086 ) ) ;
#58436 = DIRECTION ( 'NONE',  ( 0.000000000000000000, 0.000000000000000000, -1.000000000000000000 ) ) ;
#58437 = VERTEX_POINT ( 'NONE', #67466 ) ;
#58438 = VERTEX_POINT ( 'NONE', #98391 ) ;
#58439 = ORIENTED_EDGE ( 'NONE', *, *, #67383, .T. ) ;
#58440 = CARTESIAN_POINT ( 'NONE',  ( -83.62287095715007013, -24.34917612406838927, 0.1852690917426621231 ) ) ;
#58441 = CARTESIAN_POINT ( 'NONE',  ( -46.52287095715006160, -24.64898659630367561, 1.056161002820821038 ) ) ;
#58442 = CARTESIAN_POINT ( 'NONE',  ( 14.97568007496990816, -3.504021928054934509, -28.39450375387878722 ) ) ;
#58443 = CARTESIAN_POINT ( 'NONE',  ( 14.74948264216024008, 14.65492983226340407, -1.500000000000002220 ) ) ;
#58444 = B_SPLINE_CURVE_WITH_KNOTS ( 'NONE', 3,
 ( #4289, #26627, #57588, #26121, #88525, #11891 ),
 .UNSPECIFIED., .F., .F.,
 ( 4, 2, 4 ),
 ( 0.000000000000000000, 0.001380901958385390062, 0.002761803916770780125 ),
 .UNSPECIFIED. ) ;
#58445 = CARTESIAN_POINT ( 'NONE',  ( -1.268225406894735396, -21.67698866206750097, 11.49999999999999645 ) ) ;
#58446 = ORIENTED_EDGE ( 'NONE', *, *, #1575, .T. ) ;
#58447 = DIRECTION ( 'NONE',  ( -3.773278334453079618E-23, 0.9999999999976377785, 2.173523156925979975E-06 ) ) ;
#58448 = CARTESIAN_POINT ( 'NONE',  ( -115.5872436222452535, -24.92564183028979130, 1.928384488918252870 ) ) ;
#58449 = CARTESIAN_POINT ( 'NONE',  ( 17.77913403553526805, 13.70458096452923691, 11.49999999999998934 ) ) ;
#58450 = B_SPLINE_CURVE_WITH_KNOTS ( 'NONE', 3,
 ( #39834, #48464, #79394, #9883, #95125, #87519 ),
 .UNSPECIFIED., .F., .F.,
 ( 4, 2, 4 ),
 ( 6.391158118963033063E-06, 0.001387004593080781159, 0.002767618028042598960 ),
 .UNSPECIFIED. ) ;
#58451 = CYLINDRICAL_SURFACE ( 'NONE', #9185, 2.349999999999999645 ) ;
#58452 = CARTESIAN_POINT ( 'NONE',  ( -65.56866842408459206, -23.48783264082477018, -1.443836473390096353 ) ) ;
#58453 = ORIENTED_EDGE ( 'NONE', *, *, #16946, .T. ) ;
#58454 = DIRECTION ( 'NONE',  ( -2.464095846557964090E-17, 1.000000000000000000, 0.000000000000000000 ) ) ;
#58455 = CARTESIAN_POINT ( 'NONE',  ( -85.52287095715004739, -24.99132157543166954, 2.256160258750667502 ) ) ;
#58456 = ORIENTED_EDGE ( 'NONE', *, *, #84462, .T. ) ;
#58457 = ORIENTED_EDGE ( 'NONE', *, *, #33555, .T. ) ;
#58458 = VECTOR ( 'NONE', #3428, 1000.000000000000114 ) ;
#58459 = DIRECTION ( 'NONE',  ( 0.000000000000000000, -0.6401843996644797086, 0.7682212795973760722 ) ) ;
#58460 = ORIENTED_EDGE ( 'NONE', *, *, #75886, .T. ) ;
#58461 = CARTESIAN_POINT ( 'NONE',  ( -3.120219904758775975, 21.05623772282662998, -1.500000000000002220 ) ) ;
#58462 = VERTEX_POINT ( 'NONE', #28894 ) ;
#58463 = CARTESIAN_POINT ( 'NONE',  ( -89.81226385320383088, -29.50249691823240994, 6.409318347766594037 ) ) ;
#58464 = CARTESIAN_POINT ( 'NONE',  ( 21.05697796394607835, 5.830696701215154043, -1.500000000000002220 ) ) ;
#58465 = PLANE ( 'NONE',  #91862 ) ;
#58466 = CARTESIAN_POINT ( 'NONE',  ( 9.008567143757492346, 20.83016157428379955, -1.500000000000002220 ) ) ;
#58467 = LINE ( 'NONE', #96015, #27475 ) ;
#58468 = CARTESIAN_POINT ( 'NONE',  ( 5.495499487697820484, -5.876774720514418071, 20.18701882043406926 ) ) ;
#58469 = CARTESIAN_POINT ( 'NONE',  ( 1.885617179787854036, 21.85875792104173598, -1.500000000000002220 ) ) ;
#58470 = CARTESIAN_POINT ( 'NONE',  ( 7.041152093163508319, -6.376774720514424288, 21.17127001373575368 ) ) ;
#58471 = ORIENTED_EDGE ( 'NONE', *, *, #93792, .F. ) ;
#58472 = CARTESIAN_POINT ( 'NONE',  ( -13.89275734969026388, 5.965225279485572685, 31.02402280011862246 ) ) ;
#58473 = CARTESIAN_POINT ( 'NONE',  ( -121.5895376238167103, -23.47593901973091235, -1.443836447538997536 ) ) ;
#58474 = VERTEX_POINT ( 'NONE', #99880 ) ;
#58475 = CARTESIAN_POINT ( 'NONE',  ( -99.62287095715002749, -23.95044443724991012, 10.65354141964649592 ) ) ;
#58476 = CIRCLE ( 'NONE', #8263, 0.5999999999999998668 ) ;
#58477 = ORIENTED_EDGE ( 'NONE', *, *, #87332, .F. ) ;
#58478 = CARTESIAN_POINT ( 'NONE',  ( -7.326923076923074873, -6.376774720514427841, 21.75000000000001066 ) ) ;
#58479 = AXIS2_PLACEMENT_3D ( 'NONE', #9869, #1766, #95609 ) ;
#58480 = DIRECTION ( 'NONE',  ( 0.000000000000000000, -0.000000000000000000, 1.000000000000000000 ) ) ;
#58481 = CARTESIAN_POINT ( 'NONE',  ( 19.98919582620916913, -7.218065965386815996, 11.49999999999998934 ) ) ;
#58482 = CARTESIAN_POINT ( 'NONE',  ( -112.6317001763909929, -23.48783264082478794, -1.443836473390061492 ) ) ;
#58483 = CARTESIAN_POINT ( 'NONE',  ( -20.27875734969026311, -4.543225279485573864, 24.00402280011862288 ) ) ;
#58484 = CARTESIAN_POINT ( 'NONE',  ( -85.53959574234744423, -24.92564183028979485, 1.928384488918252204 ) ) ;
#58485 = DIRECTION ( 'NONE',  ( -3.773278334444166432E-23, 1.000000000000000000, 0.000000000000000000 ) ) ;
#58486 = DIRECTION ( 'NONE',  ( 1.000000000000000000, 0.000000000000000000, -0.000000000000000000 ) ) ;
#58487 = ORIENTED_EDGE ( 'NONE', *, *, #65951, .F. ) ;
#58488 = EDGE_CURVE ( 'NONE', #88020, #7140, #60370, .T. ) ;
#58489 = CARTESIAN_POINT ( 'NONE',  ( -18.05301863641116000, -7.546005365994440162, 11.49999999999999645 ) ) ;
#58490 = CARTESIAN_POINT ( 'NONE',  ( -58.62287095715004170, -24.35013146730203459, 9.818937971375111928 ) ) ;
#58491 = EDGE_CURVE ( 'NONE', #58657, #53793, #21266, .T. ) ;
#58492 = FACE_OUTER_BOUND ( 'NONE', #87366, .T. ) ;
#58493 = VERTEX_POINT ( 'NONE', #61361 ) ;
#58494 = EDGE_CURVE ( 'NONE', #89121, #7353, #63732, .T. ) ;
#58495 = CARTESIAN_POINT ( 'NONE',  ( 4.261846905714947731, -6.376774720514427841, 21.73176331363731251 ) ) ;
#58496 = CARTESIAN_POINT ( 'NONE',  ( -99.55523467558795403, -25.31557864785565926, 4.972803384765369650 ) ) ;
#58497 = ADVANCED_FACE ( 'NONE', ( #22760 ), #21762, .T. ) ;
#58498 = FACE_OUTER_BOUND ( 'NONE', #4209, .T. ) ;
#58499 = ADVANCED_FACE ( 'NONE', ( #70462 ), #40006, .T. ) ;
#58500 = CARTESIAN_POINT ( 'NONE',  ( -62.62287095715004881, -23.48783264082478794, -1.443836473390068820 ) ) ;
#58501 = CARTESIAN_POINT ( 'NONE',  ( 19.63295818312489871, -1.572306604260808260, -1.500000000000002220 ) ) ;
#58502 = ORIENTED_EDGE ( 'NONE', *, *, #49693, .F. ) ;
#58503 = LINE ( 'NONE', #19913, #92636 ) ;
#58504 = DIRECTION ( 'NONE',  ( -3.773278334453079030E-23, 0.9999999999976377785, 2.173523156925979128E-06 ) ) ;
#58505 = APPROVAL_STATUS ( 'not_yet_approved' ) ;
#58506 = ORIENTED_EDGE ( 'NONE', *, *, #49550, .T. ) ;
#58507 = CARTESIAN_POINT ( 'NONE',  ( -8.978253834636468866, -6.376774720514426953, 18.51871304725684553 ) ) ;
#58508 = PLANE ( 'NONE',  #29594 ) ;
#58509 = CARTESIAN_POINT ( 'NONE',  ( -104.6228709571500559, -23.47593901973091235, -1.443836447539001089 ) ) ;
#58510 = CARTESIAN_POINT ( 'NONE',  ( -118.5530130326516627, -24.51314013834317151, 0.6176544820404247238 ) ) ;
#58511 = CARTESIAN_POINT ( 'NONE',  ( 5.331146515430939203, -6.376774720514420736, 20.91308853528358469 ) ) ;
#58512 = DIRECTION ( 'NONE',  ( 0.000000000000000000, 0.000000000000000000, 1.000000000000000000 ) ) ;
#58513 = DIRECTION ( 'NONE',  ( 0.000000000000000000, 1.000000000000000000, 0.000000000000000000 ) ) ;
#58514 = CARTESIAN_POINT ( 'NONE',  ( -14.87316555497233495, -13.31901947624662519, -1.500000000000002220 ) ) ;
#58515 = CARTESIAN_POINT ( 'NONE',  ( -0.04339346789285819517, -22.48823745777612970, 1.345137965621359122 ) ) ;
#58516 = CARTESIAN_POINT ( 'NONE',  ( 15.68239283413728735, 12.23493734220040530, -1.500000000000002220 ) ) ;
#58517 = ORIENTED_EDGE ( 'NONE', *, *, #16773, .F. ) ;
#58518 = CARTESIAN_POINT ( 'NONE',  ( -116.6228709571500275, -23.47596703998600631, 11.44779298504227860 ) ) ;
#58519 = CARTESIAN_POINT ( 'NONE',  ( 4.215004826710222474, -6.376774720514427841, 21.34072927444733381 ) ) ;
#58520 = ADVANCED_FACE ( 'NONE', ( #2453 ), #9055, .F. ) ;
#58521 = CARTESIAN_POINT ( 'NONE',  ( 11.32485880260453293, -6.376774720514427841, -25.00877359051251148 ) ) ;
#58522 = CARTESIAN_POINT ( 'NONE',  ( -49.62287095715004881, -23.96177878511307568, 10.65340807706329684 ) ) ;
#58523 = DIRECTION ( 'NONE',  ( -0.7071067811865442421, 0.000000000000000000, 0.7071067811865507924 ) ) ;
#58524 = CARTESIAN_POINT ( 'NONE',  ( -4.568292318365942073, -5.965225279485572685, 30.06720597538392425 ) ) ;
#58525 = ORIENTED_EDGE ( 'NONE', *, *, #54265, .F. ) ;
#58526 = CARTESIAN_POINT ( 'NONE',  ( 30.53060340732036693, -4.132774720514426292, -5.153186819891554471 ) ) ;
#58527 = CARTESIAN_POINT ( 'NONE',  ( -127.5550744602278428, -24.65952944569305316, 1.056160979905707009 ) ) ;
#58528 = VERTEX_POINT ( 'NONE', #78047 ) ;
#58529 = CARTESIAN_POINT ( 'NONE',  ( -5.512817753899047268, 19.46650688538001361, -1.500000000000002220 ) ) ;
#58530 = LINE ( 'NONE', #21431, #19287 ) ;
#58531 = CARTESIAN_POINT ( 'NONE',  ( 30.93860345374796594, 0.6647747205144267646, 23.11160796525322070 ) ) ;
#58532 = DIRECTION ( 'NONE',  ( -1.000000000000000000, -0.000000000000000000, -7.994117400814786717E-16 ) ) ;
#58534 = ORIENTED_EDGE ( 'NONE', *, *, #49910, .T. ) ;
#58533 = ADVANCED_FACE ( 'NONE', ( #40521 ), #57960, .T. ) ;
#58535 = FACE_OUTER_BOUND ( 'NONE', #79541, .T. ) ;
#58536 = CARTESIAN_POINT ( 'NONE',  ( -1.967852706420949005, -5.876774720514407413, 19.18381548539530357 ) ) ;
#58537 = VECTOR ( 'NONE', #48011, 1000.000000000000000 ) ;
#58538 = CARTESIAN_POINT ( 'NONE',  ( -18.81522532469529452, 6.996975221643539911, -1.500000000000002220 ) ) ;
#58539 = CARTESIAN_POINT ( 'NONE',  ( 21.04674311342985860, -0.3259866984596996864, 11.49999999999999645 ) ) ;
#58540 = CARTESIAN_POINT ( 'NONE',  ( -29.17217916550134404, -25.16101538479635025, 6.097600585202582302 ) ) ;
#58541 = CARTESIAN_POINT ( 'NONE',  ( -70.54349239131259708, -24.52399227489127043, 9.353111116836524630 ) ) ;
#58542 = CARTESIAN_POINT ( 'NONE',  ( -17.20036718215007099, 13.84871166177648583, -1.500000000000002220 ) ) ;
#58543 = ADVANCED_FACE ( 'NONE', ( #16663 ), #62355, .T. ) ;
#58544 = CARTESIAN_POINT ( 'NONE',  ( -39.48225211724125927, -25.27805969471785019, 4.451013812573177297 ) ) ;
#58545 = CARTESIAN_POINT ( 'NONE',  ( -87.62287095715001328, -23.48786465467241769, 11.44779295918254114 ) ) ;
#58546 = CARTESIAN_POINT ( 'NONE',  ( -50.30027857337484676, -25.18440102389800828, 3.296100527055671581 ) ) ;
#58547 = EDGE_LOOP ( 'NONE', ( #18874, #44843, #75913, #95712 ) ) ;
#58548 = CARTESIAN_POINT ( 'NONE',  ( -74.52287095715007581, -23.47593901973090169, -1.443836447538996870 ) ) ;
#58549 = LINE ( 'NONE', #58061, #53481 ) ;
#58550 = ORIENTED_EDGE ( 'NONE', *, *, #59769, .F. ) ;
#58551 = ORIENTED_EDGE ( 'NONE', *, *, #35349, .T. ) ;
#58552 = FACE_OUTER_BOUND ( 'NONE', #71843, .T. ) ;
#58553 = CARTESIAN_POINT ( 'NONE',  ( -124.6228709571500701, -23.47596703998600631, 11.44779298504227860 ) ) ;
#58554 = FACE_OUTER_BOUND ( 'NONE', #93258, .T. ) ;
#58555 = CARTESIAN_POINT ( 'NONE',  ( -15.41819309731374510, 13.62919173607049927, -1.500000000000002220 ) ) ;
#58556 = CARTESIAN_POINT ( 'NONE',  ( 16.61904782137575154, -13.72857183568914685, 11.49999999999999645 ) ) ;
#58557 = ORIENTED_EDGE ( 'NONE', *, *, #83561, .T. ) ;
#58558 = LINE ( 'NONE', #96603, #23481 ) ;
#58559 = CARTESIAN_POINT ( 'NONE',  ( -53.52287095715006870, -29.50250243563736774, 8.947779886222146928 ) ) ;
#58560 = CARTESIAN_POINT ( 'NONE',  ( -4.169309590939843879, -6.376774720514411854, 19.59793130852656518 ) ) ;
#58561 = CARTESIAN_POINT ( 'NONE',  ( -7.140196579304709523, 21.16591527347414115, 11.49999999999998934 ) ) ;
#58562 = CARTESIAN_POINT ( 'NONE',  ( 15.14080536460164694, 3.622774720514426949, -26.62908960815038384 ) ) ;
#58563 = CARTESIAN_POINT ( 'NONE',  ( -76.62287095715007013, -29.50248528299804818, 1.056150453629038477 ) ) ;
#58564 = ORIENTED_EDGE ( 'NONE', *, *, #2477, .T. ) ;
#58565 = DIRECTION ( 'NONE',  ( -3.773278334453080206E-23, 0.9999999999976377785, 2.173523156925979975E-06 ) ) ;
#58566 = CARTESIAN_POINT ( 'NONE',  ( 31.48454476783385658, 4.132774720514426292, -1.134026763942596494 ) ) ;
#58567 = CARTESIAN_POINT ( 'NONE',  ( 17.12911088700535700, -11.98135219954639830, -1.500000000000002220 ) ) ;
#58568 = ORIENTED_EDGE ( 'NONE', *, *, #87437, .F. ) ;
#58570 = VERTEX_POINT ( 'NONE', #23773 ) ;
#58569 = CARTESIAN_POINT ( 'NONE',  ( -92.62287095715005592, -24.65952944569304606, 1.056160979905700348 ) ) ;
#58571 = VERTEX_POINT ( 'NONE', #54748 ) ;
#58572 = CARTESIAN_POINT ( 'NONE',  ( -100.5114778985442570, -24.40133493613050319, 9.663955038902802386 ) ) ;
#58573 = CARTESIAN_POINT ( 'NONE',  ( -15.95541298346445735, 13.85296639876547076, -1.500000000000002220 ) ) ;
#58574 = VERTEX_POINT ( 'NONE', #86678 ) ;
#58575 = CARTESIAN_POINT ( 'NONE',  ( -37.58953762381673869, -23.47596703998600276, 11.44779298504227505 ) ) ;
#58576 = CARTESIAN_POINT ( 'NONE',  ( -29.62287095715004881, -24.57400415421967566, 8.947790463233827651 ) ) ;
#58577 = DIRECTION ( 'NONE',  ( 0.000000000000000000, 2.173523156925980399E-06, -0.9999999999976378895 ) ) ;
#58578 = CARTESIAN_POINT ( 'NONE',  ( 4.621320343559625066, 12.75000000000004974, 2.100000000000000089 ) ) ;
#58579 = CARTESIAN_POINT ( 'NONE',  ( -49.37981359748505383, -25.18092312992202508, 3.262587406134465073 ) ) ;
#58580 = CARTESIAN_POINT ( 'NONE',  ( 8.489507321284875729, -19.98171680480944445, -1.500000000000002220 ) ) ;
#58581 = CARTESIAN_POINT ( 'NONE',  ( -107.5895376238167387, -23.48783264082479150, -1.443836473390060382 ) ) ;
#58583 = ORIENTED_EDGE ( 'NONE', *, *, #37996, .F. ) ;
#58582 = CARTESIAN_POINT ( 'NONE',  ( 0.6114060112162268412, -22.25658958135186793, 11.49999999999999645 ) ) ;
#58584 = CARTESIAN_POINT ( 'NONE',  ( -50.61185169649064619, -25.24728727379448046, 5.215441029265593720 ) ) ;
#58585 = DIRECTION ( 'NONE',  ( -0.000000000000000000, -1.000000000000000000, -0.000000000000000000 ) ) ;
#58586 = DIRECTION ( 'NONE',  ( 0.000000000000000000, 0.000000000000000000, -1.000000000000000000 ) ) ;
#58587 = ORIENTED_EDGE ( 'NONE', *, *, #88775, .F. ) ;
#58589 = ORIENTED_EDGE ( 'NONE', *, *, #18835, .T. ) ;
#58588 = CARTESIAN_POINT ( 'NONE',  ( -99.52287095715006160, -24.65952944569304961, 1.056160979905702346 ) ) ;
#58590 = ORIENTED_EDGE ( 'NONE', *, *, #28304, .T. ) ;
#58591 = CARTESIAN_POINT ( 'NONE',  ( 18.22465585706453339, -0.5000000000000000000, -2.153101996372891236 ) ) ;
#58592 = LINE ( 'NONE', #17148, #69271 ) ;
#58593 = CARTESIAN_POINT ( 'NONE',  ( -63.58953762381673869, -24.65952944569304250, 1.056160979905695907 ) ) ;
#58594 = CARTESIAN_POINT ( 'NONE',  ( -107.5228709571501184, -24.34917612407031129, 0.1852690917477051169 ) ) ;
#58595 = CARTESIAN_POINT ( 'NONE',  ( 8.160000000000000142, -10.65233964170348635, 1.628518864987183790 ) ) ;
#58596 = ORIENTED_EDGE ( 'NONE', *, *, #96217, .F. ) ;
#58597 = EDGE_CURVE ( 'NONE', #654, #42693, #48132, .T. ) ;
#58598 = CARTESIAN_POINT ( 'NONE',  ( 4.481524277812761525, 18.85844072219565604, 11.49999999999999645 ) ) ;
#58599 = CARTESIAN_POINT ( 'NONE',  ( -115.5228709571500758, -23.85229601348997264, 10.88205029486208630 ) ) ;
#58600 = CARTESIAN_POINT ( 'NONE',  ( 1.786768808452938950, -22.39398889530128756, -1.500000000000002220 ) ) ;
#58601 = ORIENTED_EDGE ( 'NONE', *, *, #62334, .T. ) ;
#58602 = CARTESIAN_POINT ( 'NONE',  ( -45.52287095715007581, -23.47593901973090169, -1.443836447538997092 ) ) ;
#58603 = ADVANCED_FACE ( 'NONE', ( #81070 ), #53166, .T. ) ;
#58604 = LINE ( 'NONE', #51991, #73321 ) ;
#58605 = CARTESIAN_POINT ( 'NONE',  ( -2.749999999999999112, 27.59999999999999432, 2.100000000000000089 ) ) ;
#58606 = ADVANCED_FACE ( 'NONE', ( #90176 ), #22346, .T. ) ;
#58607 = CARTESIAN_POINT ( 'NONE',  ( -97.24578741328294029, -24.82935162629097192, 1.633150109380539172 ) ) ;
#58608 = VECTOR ( 'NONE', #83194, 1000.000000000000114 ) ;
#58609 = CARTESIAN_POINT ( 'NONE',  ( 7.829539893445508270, 17.95258299782629408, 11.49999999999998934 ) ) ;
#58610 = ADVANCED_FACE ( 'NONE', ( #46007 ), #84550, .F. ) ;
#58611 = PLANE ( 'NONE',  #41287 ) ;
#58613 = VERTEX_POINT ( 'NONE', #76426 ) ;
#58612 = APPROVAL_PERSON_ORGANIZATION ( #98658, #5419, #68227 ) ;
#58614 = CARTESIAN_POINT ( 'NONE',  ( -18.46100929034391314, -11.06139713797464985, 11.49999999999998934 ) ) ;
#58615 = DIRECTION ( 'NONE',  ( -3.773278334453079618E-23, 0.9999999999976377785, 2.173523156925979975E-06 ) ) ;
#58616 = ADVANCED_FACE ( 'NONE', ( #15036 ), #19861, .T. ) ;
#58617 = CARTESIAN_POINT ( 'NONE',  ( -119.5562042904834072, -23.47596703998600631, 11.44779298504227683 ) ) ;
#58618 = CARTESIAN_POINT ( 'NONE',  ( -59.62287095715004170, -24.65952944569304606, 1.056160979905694131 ) ) ;
#58619 = CARTESIAN_POINT ( 'NONE',  ( -77.62287095715007013, -23.73934037231757443, 11.05740245334329153 ) ) ;
#58620 = CARTESIAN_POINT ( 'NONE',  ( 13.47786528765806580, -18.65256936556403744, -1.500000000000002220 ) ) ;
#58621 = MECHANICAL_CONTEXT ( 'NONE', #92623, 'mechanical' ) ;
#58622 = DIRECTION ( 'NONE',  ( 0.9890158633619158257, 0.1478094111296165136, 0.000000000000000000 ) ) ;
#58623 = CARTESIAN_POINT ( 'NONE',  ( -49.63343115848626752, -24.34968618360933590, 0.1864209137778799763 ) ) ;
#58624 = CARTESIAN_POINT ( 'NONE',  ( 2.654622155064554789, -19.98241913370796041, 11.49999999999999645 ) ) ;
#58625 = CARTESIAN_POINT ( 'NONE',  ( -109.1652331756773862, -25.10927527791083946, 3.437502883451723612 ) ) ;
#58626 = CARTESIAN_POINT ( 'NONE',  ( -74.52287095715007581, -29.50250786944525672, 11.44777988621623699 ) ) ;
#58627 = CARTESIAN_POINT ( 'NONE',  ( -46.52287095715005449, -23.96127896941631619, -0.6493128931038071316 ) ) ;
#58628 = LINE ( 'NONE', #80460, #61860 ) ;
#58629 = ADVANCED_FACE ( 'NONE', ( #33264 ), #17545, .F. ) ;
#58630 = LINE ( 'NONE', #89575, #15412 ) ;
#58631 = CARTESIAN_POINT ( 'NONE',  ( 13.99221305778824487, -14.08248706038611964, -1.500000000000002220 ) ) ;
#58632 = CARTESIAN_POINT ( 'NONE',  ( -125.5228709571500616, -23.47596703998600631, 11.44779298504227683 ) ) ;
#58633 = CARTESIAN_POINT ( 'NONE',  ( 3.669390655483735220, -19.36157329643844704, -1.500000000000002220 ) ) ;
#58634 = CARTESIAN_POINT ( 'NONE',  ( -42.48188582566654503, -24.65952944569304606, 1.056160979905694353 ) ) ;
#58635 = B_SPLINE_CURVE_WITH_KNOTS ( 'NONE', 3,
 ( #59006, #98035, #36650, #60995 ),
 .UNSPECIFIED., .F., .F.,
 ( 4, 4 ),
 ( 0.000000000000000000, 9.999999999998897304E-05 ),
 .UNSPECIFIED. ) ;
#58636 = CARTESIAN_POINT ( 'NONE',  ( -110.5228709571500616, -23.47596703998600631, 11.44779298504228038 ) ) ;
#58637 = CARTESIAN_POINT ( 'NONE',  ( -111.5228709571500190, -23.48783264082477018, -1.443836473390084585 ) ) ;
#58638 = CARTESIAN_POINT ( 'NONE',  ( 19.46067915675286386, 6.892634557253153105, 11.49999999999999645 ) ) ;
#58639 = CARTESIAN_POINT ( 'NONE',  ( -120.5520473220775983, -25.00158670708911046, 2.256160236439219702 ) ) ;
#58640 = CARTESIAN_POINT ( 'NONE',  ( -20.89466310375201985, -8.809181082428260368, 11.49999999999999645 ) ) ;
#58641 = VECTOR ( 'NONE', #29368, 1000.000000000000000 ) ;
#58642 = ORIENTED_EDGE ( 'NONE', *, *, #82475, .T. ) ;
#58643 = CARTESIAN_POINT ( 'NONE',  ( 8.160000000000000142, -10.15233964170348457, 0.003711184059992174607 ) ) ;
#58644 = CARTESIAN_POINT ( 'NONE',  ( -93.52287095715006160, -23.47596703998600631, 11.44779298504228393 ) ) ;
#58645 = EDGE_CURVE ( 'NONE', #95734, #12577, #23644, .T. ) ;
#58646 = CARTESIAN_POINT ( 'NONE',  ( -98.62287095715004170, -24.65952944569304606, 1.056160979905700792 ) ) ;
#58647 = CARTESIAN_POINT ( 'NONE',  ( -56.52287095715008292, -24.35013146730203815, 9.818937971375104823 ) ) ;
#58648 = ORIENTED_EDGE ( 'NONE', *, *, #39155, .T. ) ;
#58649 = VERTEX_POINT ( 'NONE', #77922 ) ;
#58650 = DIRECTION ( 'NONE',  ( -3.773278334453079030E-23, 0.9999999999976377785, 2.173523156925979128E-06 ) ) ;
#58651 = CARTESIAN_POINT ( 'NONE',  ( 9.198035947750891950, -20.93187084735588144, -1.500000000000002220 ) ) ;
#58652 = DIRECTION ( 'NONE',  ( 0.000000000000000000, 0.000000000000000000, 1.000000000000000000 ) ) ;
#58653 = CARTESIAN_POINT ( 'NONE',  ( 21.52761780497506905, -1.784033869580059939, -1.500000000000002220 ) ) ;
#58654 = CARTESIAN_POINT ( 'NONE',  ( -113.5205645610192562, -23.73791477778911840, 11.05961554403170233 ) ) ;
#58655 = DIRECTION ( 'NONE',  ( -3.773278334453079618E-23, 0.9999999999976377785, 2.173523156925979975E-06 ) ) ;
#58656 = CARTESIAN_POINT ( 'NONE',  ( 22.54279463279464579, 0.6884863543687869125, 11.49999999999999645 ) ) ;
#58657 = VERTEX_POINT ( 'NONE', #48007 ) ;
#58658 = CARTESIAN_POINT ( 'NONE',  ( -28.94430083015267030, -25.04003078313435537, 3.099314279037052700 ) ) ;
#58659 = AXIS2_PLACEMENT_3D ( 'NONE', #81337, #12305, #42304 ) ;
#58660 = CARTESIAN_POINT ( 'NONE',  ( 21.99661117994144988, 0.4758108284031232760, -1.500000000000002220 ) ) ;
#58661 = CARTESIAN_POINT ( 'NONE',  ( -5.366453405989237702, 1.999999999999993117, 19.19609335255483984 ) ) ;
#58662 = CARTESIAN_POINT ( 'NONE',  ( -29.24615158708846963, -25.21724433438351198, 5.024434671431828647 ) ) ;
#58663 = ORIENTED_EDGE ( 'NONE', *, *, #90335, .F. ) ;
#58664 = CARTESIAN_POINT ( 'NONE',  ( 10.86264265030973952, 5.965225279485574461, -27.62597719988137612 ) ) ;
#58665 = EDGE_CURVE ( 'NONE', #18147, #61918, #74659, .T. ) ;
#58666 = CARTESIAN_POINT ( 'NONE',  ( -47.55620429048338593, -23.47596703998600276, 11.44779298504227505 ) ) ;
#58667 = ORIENTED_EDGE ( 'NONE', *, *, #69005, .F. ) ;
#58668 = CARTESIAN_POINT ( 'NONE',  ( -45.52287095715007581, -23.47593901973090169, -1.443836447538997092 ) ) ;
#58669 = ORIENTED_EDGE ( 'NONE', *, *, #68333, .T. ) ;
#58670 = ORIENTED_EDGE ( 'NONE', *, *, #62735, .F. ) ;
#58671 = ORIENTED_EDGE ( 'NONE', *, *, #63686, .T. ) ;
#58672 = CARTESIAN_POINT ( 'NONE',  ( -100.6228709571500559, -29.50249982740957577, 7.747779886224967605 ) ) ;
#58673 = CARTESIAN_POINT ( 'NONE',  ( 32.98733314340959311, 5.965225279485572685, 2.074222136288530027 ) ) ;
#58674 = CARTESIAN_POINT ( 'NONE',  ( -57.53373409370878733, -24.65952944569304606, 1.056160979905698571 ) ) ;
#58675 = CARTESIAN_POINT ( 'NONE',  ( 20.35419724272142616, 1.316291261081859787, -1.500000000000002220 ) ) ;
#58676 = EDGE_CURVE ( 'NONE', #7077, #52807, #92809, .T. ) ;
#58677 = ORIENTED_EDGE ( 'NONE', *, *, #80574, .F. ) ;
#58678 = DIRECTION ( 'NONE',  ( 0.000000000000000000, -1.000000000000000000, 0.000000000000000000 ) ) ;
#58679 = LINE ( 'NONE', #3908, #57915 ) ;
#58681 = CARTESIAN_POINT ( 'NONE',  ( -97.52287095715007581, -24.33832256527048798, 0.1851278514138655906 ) ) ;
#58680 = CIRCLE ( 'NONE', #34417, 1.149999999999998135 ) ;
#58682 = PLANE ( 'NONE',  #38265 ) ;
#58683 = VERTEX_POINT ( 'NONE', #86054 ) ;
#58684 = CARTESIAN_POINT ( 'NONE',  ( -75.48966160648491552, -25.00158670708910691, 2.256160236439223699 ) ) ;
#58685 = CARTESIAN_POINT ( 'NONE',  ( -86.62287095715005592, -23.48786465467241413, 11.44779295918254469 ) ) ;
#58686 = LOCAL_TIME ( 0, 54, 15.00000000000000000, #2220 ) ;
#58687 = EDGE_LOOP ( 'NONE', ( #13726, #4522, #98499, #71149 ) ) ;
#58688 = CARTESIAN_POINT ( 'NONE',  ( -8.119355292522030254, -19.11072509857415369, -1.500000000000002220 ) ) ;
#58689 = ORIENTED_EDGE ( 'NONE', *, *, #13718, .F. ) ;
#58690 = CC_DESIGN_DATE_AND_TIME_ASSIGNMENT ( #57767, #34419, ( #10919 ) ) ;
#58692 = ORIENTED_EDGE ( 'NONE', *, *, #63532, .F. ) ;
#58691 = CARTESIAN_POINT ( 'NONE',  ( 11.62916340711181284, 5.965225279485572685, 28.75961759920349792 ) ) ;
#58693 = CARTESIAN_POINT ( 'NONE',  ( 22.81105451610979173, 6.475225279485573360, -18.46691820600746681 ) ) ;
#58694 = LINE ( 'NONE', #56715, #30865 ) ;
#58695 = ORIENTED_EDGE ( 'NONE', *, *, #34378, .T. ) ;
#58696 = EDGE_LOOP ( 'NONE', ( #33244, #100312, #44535, #4657 ) ) ;
#58697 = CARTESIAN_POINT ( 'NONE',  ( -33.52287095715007581, -23.72773821059535848, 11.05748984161097681 ) ) ;
#58698 = LINE ( 'NONE', #18135, #46462 ) ;
#58699 = DIRECTION ( 'NONE',  ( 0.000000000000000000, 0.000000000000000000, -1.000000000000000000 ) ) ;
#58700 = CARTESIAN_POINT ( 'NONE',  ( -43.50597321196386957, -23.96169478059712787, 10.65365249895718769 ) ) ;
#58702 = ORIENTED_EDGE ( 'NONE', *, *, #57595, .T. ) ;
#58701 = CARTESIAN_POINT ( 'NONE',  ( 7.643743511751816655, -20.74876368896106271, 11.49999999999999645 ) ) ;
#58703 = CARTESIAN_POINT ( 'NONE',  ( -108.5890517283027918, -24.34968618360934300, 0.1864209137778971292 ) ) ;
#58704 = CARTESIAN_POINT ( 'NONE',  ( -8.787219534579676861, -20.84281209399103929, -1.500000000000002220 ) ) ;
#58706 = ORIENTED_EDGE ( 'NONE', *, *, #46492, .F. ) ;
#58705 = CARTESIAN_POINT ( 'NONE',  ( -115.5133545927454719, -25.00182538069147142, 7.747789668545041586 ) ) ;
#58707 = ORIENTED_EDGE ( 'NONE', *, *, #21007, .T. ) ;
#58708 = B_SPLINE_CURVE_WITH_KNOTS ( 'NONE', 3,
 ( #26703, #89598, #96219, #4373 ),
 .UNSPECIFIED., .F., .F.,
 ( 4, 4 ),
 ( 6.938893903907228378E-18, 8.001919664664916716E-05 ),
 .UNSPECIFIED. ) ;
#58709 = CARTESIAN_POINT ( 'NONE',  ( -10.32858501761201353, -6.295917116278983983, 28.25808420984930791 ) ) ;
#58710 = CIRCLE ( 'NONE', #60318, 2.249999999999998668 ) ;
#58711 = B_SPLINE_CURVE_WITH_KNOTS ( 'NONE', 3,
 ( #98746, #96757, #20623, #51590, #58210, #89152 ),
 .UNSPECIFIED., .F., .F.,
 ( 4, 2, 4 ),
 ( 1.570887131794952276E-05, 0.001396322306279763675, 0.002776935741241577573 ),
 .UNSPECIFIED. ) ;
#58712 = CARTESIAN_POINT ( 'NONE',  ( 8.160000000000000142, -10.65233964170348635, 0.003711184059992174607 ) ) ;
#58713 = ORIENTED_EDGE ( 'NONE', *, *, #64730, .T. ) ;
#58714 = CARTESIAN_POINT ( 'NONE',  ( -21.01389645921736360, -2.595061309317715281, -1.500000000000002220 ) ) ;
#58715 = CARTESIAN_POINT ( 'NONE',  ( 32.85081302853803464, 3.622774720514426949, -13.10817780685209577 ) ) ;
#58716 = CARTESIAN_POINT ( 'NONE',  ( 30.53060340732035982, 6.475225279485573360, 20.86760796525322093 ) ) ;
#58717 = CARTESIAN_POINT ( 'NONE',  ( -19.27636426328722763, -11.15942449563467775, -1.500000000000002220 ) ) ;
#58718 = DIRECTION ( 'NONE',  ( -0.000000000000000000, 1.000000000000000000, -0.000000000000000000 ) ) ;
#58719 = ORIENTED_EDGE ( 'NONE', *, *, #22151, .F. ) ;
#58720 = CARTESIAN_POINT ( 'NONE',  ( 30.57287095715005520, -6.475225279485573360, 25.41160796525322141 ) ) ;
#58721 = CARTESIAN_POINT ( 'NONE',  ( -50.52287095715006160, -23.47596703998600631, 11.44779298504229104 ) ) ;
#58722 = B_SPLINE_CURVE_WITH_KNOTS ( 'NONE', 3,
 ( #30089, #98098, #82384, #30590 ),
 .UNSPECIFIED., .F., .F.,
 ( 4, 4 ),
 ( 0.000000000000000000, 1.000000000000000000 ),
 .UNSPECIFIED. ) ;
#58723 = CARTESIAN_POINT ( 'NONE',  ( -4.568292318365942073, 5.965225279485572685, 30.06720597538392425 ) ) ;
#58724 = DIRECTION ( 'NONE',  ( -2.417950247244706201E-16, 0.000000000000000000, 1.000000000000000000 ) ) ;
#58725 = CARTESIAN_POINT ( 'NONE',  ( 6.966380261627926451, -18.21767524041069564, 11.49999999999998934 ) ) ;
#58726 = AXIS2_PLACEMENT_3D ( 'NONE', #46509, #8445, #77438 ) ;
#58727 = EDGE_CURVE ( 'NONE', #55726, #69852, #38875, .T. ) ;
#58728 = CARTESIAN_POINT ( 'NONE',  ( -19.34459864454321831, 9.218434461607088792, -1.500000000000002220 ) ) ;
#58729 = CARTESIAN_POINT ( 'NONE',  ( -27.70544111104076990, -24.57999497002659695, 1.628749937114660540 ) ) ;
#58730 = AXIS2_PLACEMENT_3D ( 'NONE', #75343, #5844, #29177 ) ;
#58731 = EDGE_CURVE ( 'NONE', #31069, #86729, #27409, .T. ) ;
#58732 = CARTESIAN_POINT ( 'NONE',  ( 6.983857881298739301, -1.335431525194936242, 19.26533332368850182 ) ) ;
#58733 = CARTESIAN_POINT ( 'NONE',  ( -34.52287095715006160, -23.47593901973090169, -1.443836447538997314 ) ) ;
#58734 = CARTESIAN_POINT ( 'NONE',  ( 9.312063170398973355, -20.82641193498425025, -1.500000000000002220 ) ) ;
#58735 = APPROVAL_ROLE ( '' ) ;
#58736 = CARTESIAN_POINT ( 'NONE',  ( -107.6228709571500701, -29.50250243563736774, 8.947779886222136270 ) ) ;
#58737 = CARTESIAN_POINT ( 'NONE',  ( -128.5228709571501611, -24.50216790748206108, 0.6166512839542577229 ) ) ;
#58738 = CARTESIAN_POINT ( 'NONE',  ( 19.48829924427396421, 3.997931079995220127, 11.49999999999999645 ) ) ;
#58739 = CARTESIAN_POINT ( 'NONE',  ( -104.6328447509342539, -23.73766607897670866, -1.055555164236450016 ) ) ;
#58740 = CARTESIAN_POINT ( 'NONE',  ( -74.63881899433903300, -23.96169478059713498, 10.65365249895717881 ) ) ;
#58741 = CARTESIAN_POINT ( 'NONE',  ( -48.56837829547282581, -23.48783264082477729, -1.443836473390069264 ) ) ;
#58742 = EDGE_LOOP ( 'NONE', ( #12889, #16099, #47901, #10693 ) ) ;
#58743 = EDGE_CURVE ( 'NONE', #94221, #23708, #24644, .T. ) ;
#58744 = CARTESIAN_POINT ( 'NONE',  ( -25.53321154136338933, -24.92494999122525456, 4.756956508522131699 ) ) ;
#58745 = CARTESIAN_POINT ( 'NONE',  ( -62.62287095715007723, -24.50321055353805022, 9.387540953477532923 ) ) ;
#58746 = CARTESIAN_POINT ( 'NONE',  ( 10.00111611332133421, -19.26892646806700071, 11.49999999999998934 ) ) ;
#58747 = CARTESIAN_POINT ( 'NONE',  ( -77.62287095715007013, -24.66019654487199730, 8.947790411086128159 ) ) ;
#58748 = CARTESIAN_POINT ( 'NONE',  ( -1.979602623192304955, -19.45764201480039901, -1.500000000000002220 ) ) ;
#58749 = DIRECTION ( 'NONE',  ( 0.000000000000000000, 0.000000000000000000, -1.000000000000000000 ) ) ;
#58750 = VECTOR ( 'NONE', #87552, 1000.000000000000227 ) ;
#58751 = ORIENTED_EDGE ( 'NONE', *, *, #5153, .T. ) ;
#58752 = COORDINATED_UNIVERSAL_TIME_OFFSET ( 0, 0, .AHEAD. ) ;
#58753 = LOCAL_TIME ( 0, 54, 15.00000000000000000, #27798 ) ;
#58754 = DIRECTION ( 'NONE',  ( -3.773278334453079030E-23, 0.9999999999976377785, 2.173523156925979128E-06 ) ) ;
#58755 = CARTESIAN_POINT ( 'NONE',  ( -17.80769721941407369, -10.09151516499986734, 11.49999999999999645 ) ) ;
#58756 = LINE ( 'NONE', #65896, #71641 ) ;
#58757 = CARTESIAN_POINT ( 'NONE',  ( -61.25483432547240881, -25.20321001719939957, 6.713658772143283215 ) ) ;
#58758 = AXIS2_PLACEMENT_3D ( 'NONE', #49144, #3462, #26784 ) ;
#58759 = ORIENTED_EDGE ( 'NONE', *, *, #22888, .F. ) ;
#58760 = CARTESIAN_POINT ( 'NONE',  ( 8.160000000000000142, -9.728493947732140157, 1.239948043688426926 ) ) ;
#58761 = CARTESIAN_POINT ( 'NONE',  ( -39.44687923781921057, -25.18431065692472259, 4.188173887285336683 ) ) ;
#58762 = DIRECTION ( 'NONE',  ( -0.7512896232465786639, 0.000000000000000000, -0.6599726524652470561 ) ) ;
#58763 = AXIS2_PLACEMENT_3D ( 'NONE', #54951, #92988, #70165 ) ;
#58764 = B_SPLINE_CURVE_WITH_KNOTS ( 'NONE', 3,
 ( #3393, #94211, #71394, #17596, #65305, #26211, #40443, #95722, #2891, #57184 ),
 .UNSPECIFIED., .F., .F.,
 ( 4, 2, 2, 2, 4 ),
 ( -1.423960876792978737E-05, 0.0005136504108877040049, 0.001041540430543337831, 0.001569430450198971549, 0.002097320469854605483 ),
 .UNSPECIFIED. ) ;
#58765 = CARTESIAN_POINT ( 'NONE',  ( -98.62287095715007013, -23.47596703998600631, 11.44779298504227860 ) ) ;
#58766 = ORIENTED_EDGE ( 'NONE', *, *, #19017, .F. ) ;
#58767 = CARTESIAN_POINT ( 'NONE',  ( -80.96226385320385077, -25.14083923594767001, 2.947789366383926968 ) ) ;
#58768 = EDGE_CURVE ( 'NONE', #16463, #4897, #4413, .T. ) ;
#58769 = CARTESIAN_POINT ( 'NONE',  ( -18.14924840124409045, -14.16824886576183040, 11.49999999999999645 ) ) ;
#58770 = CARTESIAN_POINT ( 'NONE',  ( 0.8422786845129024424, 22.77647355728978340, 11.49999999999998934 ) ) ;
#58771 = CARTESIAN_POINT ( 'NONE',  ( -110.5193695319981657, -23.85049219812686161, 10.88485053497526778 ) ) ;
#58772 = B_SPLINE_SURFACE_WITH_KNOTS ( 'NONE', 3, 3, ( 
 ( #23334, #47701, #71039, #47201 ),
 ( #54817, #63442, #17744, #92856 ),
 ( #48716, #63952, #1527, #78120 ),
 ( #71540, #39579, #24848, #24353 ),
 ( #79634, #86750, #78618, #23844 ),
 ( #77623, #9126, #8633, #2035 ),
 ( #25352, #17238, #10127, #70531 ),
 ( #48205, #1019, #79135, #9630 ),
 ( #31465, #94362, #93353, #70026 ),
 ( #85753, #55823, #41092, #54319 ) ),
 .UNSPECIFIED., .F., .F., .F.,
 ( 4, 3, 3, 4 ),
 ( 4, 4 ),
 ( 0.7022005934544807149, 0.7765311282028795059, 0.8508616629512784080, 0.9995227324480759901 ),
 ( 0.3495361808025915229, 0.3507572245070639250 ),
 .UNSPECIFIED. ) ;
#58773 = CARTESIAN_POINT ( 'NONE',  ( -40.52287095715009002, -24.51163499207178376, 0.6490370598555547099 ) ) ;
#58774 = CARTESIAN_POINT ( 'NONE',  ( -49.65519464679333339, -25.23424849805013892, 3.597430756124838869 ) ) ;
#58775 = CARTESIAN_POINT ( 'NONE',  ( -50.62287095715005592, -25.00158670708909625, 2.256160236439165967 ) ) ;
#58776 = CARTESIAN_POINT ( 'NONE',  ( -110.5947698665794832, -23.85016227208580375, -0.8807180028928308646 ) ) ;
#58777 = CARTESIAN_POINT ( 'NONE',  ( 4.863445656156933694, -21.36585520573490626, 11.49999999999998934 ) ) ;
#58778 = ADVANCED_FACE ( 'NONE', ( #54614 ), #61282, .T. ) ;
#58779 = DIRECTION ( 'NONE',  ( -0.7071067811865507924, -0.000000000000000000, -0.7071067811865442421 ) ) ;
#58780 = AXIS2_PLACEMENT_3D ( 'NONE', #11182, #49763, #45509 ) ;
#58781 = B_SPLINE_CURVE_WITH_KNOTS ( 'NONE', 3,
 ( #54194, #46075, #13602, #29835 ),
 .UNSPECIFIED., .F., .F.,
 ( 4, 4 ),
 ( 0.0001059329845610884477, 0.03369911402185697680 ),
 .UNSPECIFIED. ) ;
#58782 = CARTESIAN_POINT ( 'NONE',  ( -3.737436867076076030, 13.63388347648318444, 2.100000000000000089 ) ) ;
#58783 = PLANE ( 'NONE',  #4737 ) ;
#58784 = FACE_OUTER_BOUND ( 'NONE', #93895, .T. ) ;
#58785 = ORIENTED_EDGE ( 'NONE', *, *, #84803, .F. ) ;
#58786 = CARTESIAN_POINT ( 'NONE',  ( -19.95082702767638239, -4.354873812894156870, -1.500000000000002220 ) ) ;
#58787 = ORIENTED_EDGE ( 'NONE', *, *, #45300, .F. ) ;
#58788 = ORIENTED_EDGE ( 'NONE', *, *, #60229, .F. ) ;
#58789 = ORIENTED_EDGE ( 'NONE', *, *, #17701, .F. ) ;
#58790 = EDGE_LOOP ( 'NONE', ( #73134, #41427, #39153, #37067, #24329 ) ) ;
#58791 = CARTESIAN_POINT ( 'NONE',  ( 22.66633601775066253, -4.223608244049824378, 11.49999999999998934 ) ) ;
#58792 = CARTESIAN_POINT ( 'NONE',  ( -105.5895376238167387, -23.48783264082479150, -1.443836473390060160 ) ) ;
#58793 = CARTESIAN_POINT ( 'NONE',  ( 3.706880958665978998, 19.89330832657401515, -1.500000000000002220 ) ) ;
#58794 = VECTOR ( 'NONE', #53699, 1000.000000000000000 ) ;
#58795 = ORIENTED_EDGE ( 'NONE', *, *, #31967, .T. ) ;
#58796 = DIRECTION ( 'NONE',  ( -3.773278334453079618E-23, 0.9999999999976377785, 2.173523156925979975E-06 ) ) ;
#58797 = LINE ( 'NONE', #34959, #10965 ) ;
#58798 = CARTESIAN_POINT ( 'NONE',  ( -76.52287095715007581, -24.66019654487199730, 8.947790411086124607 ) ) ;
#58799 = FACE_OUTER_BOUND ( 'NONE', #36744, .T. ) ;
#58801 = ORIENTED_EDGE ( 'NONE', *, *, #32063, .T. ) ;
#58800 = CARTESIAN_POINT ( 'NONE',  ( -2.881439591185620319, 21.19155266312798958, 11.49999999999999645 ) ) ;
#58802 = DIRECTION ( 'NONE',  ( 0.000000000000000000, 2.173523156925980399E-06, -0.9999999999976378895 ) ) ;
#58803 = AXIS2_PLACEMENT_3D ( 'NONE', #63511, #24421, #77190 ) ;
#58804 = VERTEX_POINT ( 'NONE', #88566 ) ;
#58805 = CARTESIAN_POINT ( 'NONE',  ( -21.31523168734759466, -6.469442287714795015, -1.500000000000002220 ) ) ;
#58806 = CARTESIAN_POINT ( 'NONE',  ( -20.66316395829706209, -0.6310838753663271516, 11.49999999999998934 ) ) ;
#58807 = EDGE_CURVE ( 'NONE', #14292, #39331, #50015, .T. ) ;
#58808 = B_SPLINE_CURVE_WITH_KNOTS ( 'NONE', 3,
 ( #98091, #51443, #13357, #44829, #82380, #67675, #29088, #28597, #59559, #90494 ),
 .UNSPECIFIED., .F., .F.,
 ( 4, 2, 2, 2, 4 ),
 ( 2.602085213965210642E-18, 0.0002772168619526806685, 0.0005544337239053587349, 0.0008316505858580367470, 0.001108867447810714868 ),
 .UNSPECIFIED. ) ;
#58809 = ORIENTED_EDGE ( 'NONE', *, *, #43371, .T. ) ;
#58810 = CARTESIAN_POINT ( 'NONE',  ( 3.787259615384621636, -5.876774720514405637, 18.51923076923076650 ) ) ;
#58811 = VERTEX_POINT ( 'NONE', #35777 ) ;
#58812 = CARTESIAN_POINT ( 'NONE',  ( -81.52287095715006160, -24.34917612407036458, 0.1852690917478629073 ) ) ;
#58813 = ORIENTED_EDGE ( 'NONE', *, *, #70993, .T. ) ;
#58814 = CARTESIAN_POINT ( 'NONE',  ( 19.44712688777480736, 7.780496645421295376, -1.500000000000002220 ) ) ;
#58815 = CARTESIAN_POINT ( 'NONE',  ( 20.57945552106664877, -7.502658216658728563, 11.49999999999999645 ) ) ;
#58816 = B_SPLINE_CURVE_WITH_KNOTS ( 'NONE', 3,
 ( #76982, #51674, #98827, #22192 ),
 .UNSPECIFIED., .F., .F.,
 ( 4, 4 ),
 ( 0.000000000000000000, 9.999999999996123101E-05 ),
 .UNSPECIFIED. ) ;
#58817 = CARTESIAN_POINT ( 'NONE',  ( -2.499999999999993339, 19.99999999999999645, 2.100000000000000089 ) ) ;
#58818 = CARTESIAN_POINT ( 'NONE',  ( -19.74168752133572724, 10.86179948771369297, 11.49999999999998934 ) ) ;
#58819 = EDGE_CURVE ( 'NONE', #89693, #55307, #26158, .T. ) ;
#58820 = CARTESIAN_POINT ( 'NONE',  ( 20.88312143257166653, -1.666129412636018214, -1.500000000000002220 ) ) ;
#58822 = LINE ( 'NONE', #15498, #70832 ) ;
#58821 = B_SPLINE_CURVE_WITH_KNOTS ( 'NONE', 3,
 ( #75713, #30548, #45783, #90954 ),
 .UNSPECIFIED., .F., .F.,
 ( 4, 4 ),
 ( 1.387778780781445676E-17, 9.999999999998900014E-05 ),
 .UNSPECIFIED. ) ;
#58823 = CARTESIAN_POINT ( 'NONE',  ( 5.654871928786437074, -5.876774720514419847, 20.64717925217163952 ) ) ;
#58824 = CARTESIAN_POINT ( 'NONE',  ( -119.5576586416463698, -23.48786465467241769, 11.44779295918253759 ) ) ;
#58825 = CIRCLE ( 'NONE', #86337, 0.8160000000000007248 ) ;
#58826 = PLANE ( 'NONE',  #63740 ) ;
#58827 = ORIENTED_EDGE ( 'NONE', *, *, #23308, .F. ) ;
#58828 = AXIS2_PLACEMENT_3D ( 'NONE', #39162, #70118, #599 ) ;
#58829 = VERTEX_POINT ( 'NONE', #81941 ) ;
#58830 = ORIENTED_EDGE ( 'NONE', *, *, #100082, .F. ) ;
#58831 = DIRECTION ( 'NONE',  ( 1.955152872784845154E-15, -1.000000000000000000, -3.740001113483016365E-15 ) ) ;
#58832 = CARTESIAN_POINT ( 'NONE',  ( 15.63241172484657682, -14.69700884395465934, -1.500000000000002220 ) ) ;
#58833 = VECTOR ( 'NONE', #65016, 1000.000000000000114 ) ;
#58834 = DIRECTION ( 'NONE',  ( -2.135527794058834642E-14, 0.000000000000000000, -1.000000000000000000 ) ) ;
#58835 = VERTEX_POINT ( 'NONE', #64758 ) ;
#58836 = CARTESIAN_POINT ( 'NONE',  ( -20.42954818520503935, 5.180689535515515587, -1.500000000000002220 ) ) ;
#58837 = DIRECTION ( 'NONE',  ( -1.000000000000000000, 0.000000000000000000, -7.994117400814786717E-16 ) ) ;
#58838 = CARTESIAN_POINT ( 'NONE',  ( 3.181132013147180970, -6.376774720514426065, 21.64201922499777808 ) ) ;
#58839 = DIRECTION ( 'NONE',  ( 0.000000000000000000, 0.000000000000000000, -1.000000000000000000 ) ) ;
#58840 = CARTESIAN_POINT ( 'NONE',  ( -1.382686142301752019, 8.868309232919825646, -9.000000000000000000 ) ) ;
#58841 = CARTESIAN_POINT ( 'NONE',  ( 16.26279755680690542, -1.684774720514426560, -27.67997040356620531 ) ) ;
#58842 = CARTESIAN_POINT ( 'NONE',  ( 14.53198226072946220, 16.64418356588832992, -1.500000000000002220 ) ) ;
#58843 = VECTOR ( 'NONE', #73075, 1000.000000000000114 ) ;
#58844 = EDGE_CURVE ( 'NONE', #50489, #53334, #54425, .T. ) ;
#58845 = CARTESIAN_POINT ( 'NONE',  ( -81.62360521410421654, -24.66019654487198665, 8.947790411086131712 ) ) ;
#58846 = ADVANCED_FACE ( 'NONE', ( #19041 ), #50500, .F. ) ;
#58847 = CARTESIAN_POINT ( 'NONE',  ( -51.93149462243456327, -25.31633352654386471, 6.174051004181417390 ) ) ;
#58848 = DIRECTION ( 'NONE',  ( 0.000000000000000000, -1.000000000000000000, 0.000000000000000000 ) ) ;
#58849 = DIRECTION ( 'NONE',  ( 1.000000000000000000, 1.655121434032223174E-15, 0.000000000000000000 ) ) ;
#58850 = CARTESIAN_POINT ( 'NONE',  ( 21.32124590881793225, -1.116183810207903804, 11.49999999999998934 ) ) ;
#58851 = CARTESIAN_POINT ( 'NONE',  ( 2.246611357655420083, 0.1632191352058117717, -0.1632191352058112166 ) ) ;
#58852 = CARTESIAN_POINT ( 'NONE',  ( -90.25673798828883321, -25.26266127311082954, 3.981777872396911278 ) ) ;
#58853 = EDGE_CURVE ( 'NONE', #36363, #2649, #86511, .T. ) ;
#58854 = CARTESIAN_POINT ( 'NONE',  ( -64.49570014113403715, -24.51419770103158058, 9.386484678747169852 ) ) ;
#58855 = DIRECTION ( 'NONE',  ( 0.000000000000000000, 0.000000000000000000, -1.000000000000000000 ) ) ;
#58856 = CARTESIAN_POINT ( 'NONE',  ( -19.18631400275845422, -11.98935526391121087, -1.500000000000002220 ) ) ;
#58857 = B_SPLINE_SURFACE_WITH_KNOTS ( 'NONE', 3, 3, ( 
 ( #93729, #69901, #46570, #30838 ),
 ( #54195, #47077, #61803, #48076 ),
 ( #85621, #1404, #16107, #77991 ),
 ( #54688, #23211, #24223, #56198 ),
 ( #38946, #79512, #8505, #25221 ),
 ( #39456, #92723, #63313, #70405 ),
 ( #55697, #62303, #892, #70913 ) ),
 .UNSPECIFIED., .F., .F., .F.,
 ( 4, 3, 4 ),
 ( 4, 4 ),
 ( 0.0004766839783843426618, 0.1029713700210909133, 0.2054660560637974753 ),
 ( 0.3795905586011096289, 0.3807784255434110698 ),
 .UNSPECIFIED. ) ;
#58858 = EDGE_CURVE ( 'NONE', #7917, #51194, #89049, .T. ) ;
#58859 = VERTEX_POINT ( 'NONE', #81455 ) ;
#58860 = CARTESIAN_POINT ( 'NONE',  ( 3.825768195983636044, -5.876774720514424288, 21.47884071039599618 ) ) ;
#58861 = CARTESIAN_POINT ( 'NONE',  ( -79.51716573576175051, -23.73766607897669800, -1.055555164236459564 ) ) ;
#58862 = CARTESIAN_POINT ( 'NONE',  ( -5.448126336921106372, -18.99418723138115084, 11.49999999999999645 ) ) ;
#58863 = CARTESIAN_POINT ( 'NONE',  ( -74.58953762381673869, -23.48783264082478794, -1.443836473390067265 ) ) ;
#58864 = B_SPLINE_CURVE_WITH_KNOTS ( 'NONE', 3,
 ( #61962, #61464, #77159, #53848 ),
 .UNSPECIFIED., .F., .F.,
 ( 4, 4 ),
 ( 0.000000000000000000, 1.000000000000000000 ),
 .UNSPECIFIED. ) ;
#58865 =( BOUNDED_CURVE ( )  B_SPLINE_CURVE ( 3, ( #68970, #54764, #17181, #77067 ),
 .UNSPECIFIED., .F., .T. ) 
 B_SPLINE_CURVE_WITH_KNOTS ( ( 4, 4 ),
 ( 4.603180203402792436, 4.712388980384689674 ),
 .UNSPECIFIED. ) 
 CURVE ( )  GEOMETRIC_REPRESENTATION_ITEM ( )  RATIONAL_B_SPLINE_CURVE ( ( 1.000000000000000000, 0.9990063671772055898, 0.9990063671772055898, 1.000000000000000000 ) ) 
 REPRESENTATION_ITEM ( '' )  );
#58866 = CARTESIAN_POINT ( 'NONE',  ( -67.65233053103399641, -23.48783264082477018, -1.443836473390094799 ) ) ;
#58867 = VERTEX_POINT ( 'NONE', #43395 ) ;
#58868 = EDGE_CURVE ( 'NONE', #42081, #86899, #41785, .T. ) ;
#58869 = CARTESIAN_POINT ( 'NONE',  ( -11.64875734969026233, -5.965225279485572685, 31.02402280011862246 ) ) ;
#58870 = CARTESIAN_POINT ( 'NONE',  ( -29.54861811807234417, -25.26026587690250480, 3.015634576047991011 ) ) ;
#58871 = AXIS2_PLACEMENT_3D ( 'NONE', #95122, #10888, #25611 ) ;
#58872 = CARTESIAN_POINT ( 'NONE',  ( -100.4426124108961176, -25.17353343843558378, 7.101635449178290926 ) ) ;
#58873 = CARTESIAN_POINT ( 'NONE',  ( 18.49883484089910723, -11.16122333755292750, 11.49999999999998934 ) ) ;
#58874 = CARTESIAN_POINT ( 'NONE',  ( -49.36186039879741116, -25.27517977621036849, 3.293514770891703858 ) ) ;
#58875 = DIRECTION ( 'NONE',  ( 0.000000000000000000, 0.000000000000000000, 1.000000000000000000 ) ) ;
#58876 = EDGE_CURVE ( 'NONE', #11406, #84649, #11574, .T. ) ;
#58877 = PLANE ( 'NONE',  #85323 ) ;
#58878 = CARTESIAN_POINT ( 'NONE',  ( -81.78239782233198696, -25.19580958332243981, 6.707330381882551151 ) ) ;
#58879 = CARTESIAN_POINT ( 'NONE',  ( 14.45944668481935658, 13.51102189132778442, 11.49999999999998934 ) ) ;
#58880 = ORIENTED_EDGE ( 'NONE', *, *, #12883, .T. ) ;
#58881 = VECTOR ( 'NONE', #60021, 1000.000000000000000 ) ;
#58882 = CARTESIAN_POINT ( 'NONE',  ( 19.68333694646799614, 4.735253856516091098, 11.49999999999999645 ) ) ;
#58883 = CARTESIAN_POINT ( 'NONE',  ( 21.57151214508649772, -0.8999999999999998002, 0.000000000000000000 ) ) ;
#58884 = CARTESIAN_POINT ( 'NONE',  ( 5.696197030082937651, -6.376774720514422512, 21.05387829558662816 ) ) ;
#58885 = EDGE_LOOP ( 'NONE', ( #16003, #75098, #73830, #63596 ) ) ;
#58886 = CARTESIAN_POINT ( 'NONE',  ( -37.52287095715006160, -23.73934037231756022, 11.05740245334329686 ) ) ;
#58887 = CARTESIAN_POINT ( 'NONE',  ( 12.88745205057041510, -5.152774720521900775, -28.14312002385437239 ) ) ;
#58888 = CARTESIAN_POINT ( 'NONE',  ( -71.52287095715010423, -24.35013146730203815, 9.818937971375099494 ) ) ;
#58889 = LINE ( 'NONE', #44160, #6782 ) ;
#58890 = CARTESIAN_POINT ( 'NONE',  ( -50.54027953994811639, -25.12358199471872311, 7.098256093999977701 ) ) ;
#58891 = CARTESIAN_POINT ( 'NONE',  ( 16.02535498940104830, 12.03463022438520191, 11.49999999999998934 ) ) ;
#58892 = CARTESIAN_POINT ( 'NONE',  ( 11.16000000000000014, -10.15233964170348457, 0.003711184059992174607 ) ) ;
#58893 = EDGE_LOOP ( 'NONE', ( #47654, #26575, #5607, #78736 ) ) ;
#58894 = VECTOR ( 'NONE', #91197, 1000.000000000000000 ) ;
#58895 = CARTESIAN_POINT ( 'NONE',  ( -32.62287095715004170, -23.96177878511308634, 10.65340807706331105 ) ) ;
#58896 = CARTESIAN_POINT ( 'NONE',  ( -127.5228709571500616, -23.47593901973090524, -1.443836447538996204 ) ) ;
#58897 = CARTESIAN_POINT ( 'NONE',  ( 20.13489193910601216, 1.682774720514426114, -22.92085183005151450 ) ) ;
#58898 = DIRECTION ( 'NONE',  ( -3.773278334453079030E-23, 0.9999999999976377785, 2.173523156925979128E-06 ) ) ;
#58899 = FACE_OUTER_BOUND ( 'NONE', #97103, .T. ) ;
#58900 = AXIS2_PLACEMENT_3D ( 'NONE', #1822, #77914, #310 ) ;
#58901 = EDGE_CURVE ( 'NONE', #100062, #67442, #27666, .T. ) ;
#58902 = EDGE_CURVE ( 'NONE', #61298, #69448, #50227, .T. ) ;
#58903 = CARTESIAN_POINT ( 'NONE',  ( 0.4325450954222598288, 0.000000000000000000, 0.000000000000000000 ) ) ;
#58904 = ORIENTED_EDGE ( 'NONE', *, *, #70784, .T. ) ;
#58905 = CARTESIAN_POINT ( 'NONE',  ( -14.66855384320708033, -14.05595220846724835, 11.49999999999998934 ) ) ;
#58906 = VECTOR ( 'NONE', #24010, 1000.000000000000000 ) ;
#58907 = VERTEX_POINT ( 'NONE', #88067 ) ;
#58908 = CARTESIAN_POINT ( 'NONE',  ( 11.31314246093949727, 19.96360691973900359, 11.49999999999998934 ) ) ;
#58909 = DIRECTION ( 'NONE',  ( -0.000000000000000000, -1.000000000000000000, 0.000000000000000000 ) ) ;
#58910 = VERTEX_POINT ( 'NONE', #3346 ) ;
#58911 = CARTESIAN_POINT ( 'NONE',  ( -108.5228709571501327, -24.51387760970724727, 9.387446482453400520 ) ) ;
#58912 = B_SPLINE_CURVE_WITH_KNOTS ( 'NONE', 3,
 ( #47061, #93713, #24206, #93212 ),
 .UNSPECIFIED., .F., .F.,
 ( 4, 4 ),
 ( 0.000000000000000000, 9.999999999998897304E-05 ),
 .UNSPECIFIED. ) ;
#58913 = LINE ( 'NONE', #98954, #22645 ) ;
#58914 = CARTESIAN_POINT ( 'NONE',  ( -87.55620429048337883, -24.64898659630528854, 1.056161002820825923 ) ) ;
#58916 = VERTEX_POINT ( 'NONE', #89559 ) ;
#58915 = CARTESIAN_POINT ( 'NONE',  ( 4.903939382885006637, -20.63555827282145572, 11.49999999999999645 ) ) ;
#58917 = ORIENTED_EDGE ( 'NONE', *, *, #45327, .T. ) ;
#58918 = CARTESIAN_POINT ( 'NONE',  ( -12.03526013704878039, -18.61824004984164560, 11.49999999999998934 ) ) ;
#58919 = CARTESIAN_POINT ( 'NONE',  ( -11.90445915685808131, 16.78794160864392992, 11.49999999999998934 ) ) ;
#58920 = ADVANCED_FACE ( 'NONE', ( #18544 ), #12427, .T. ) ;
#58921 = EDGE_LOOP ( 'NONE', ( #91855, #98845, #29134, #25614, #85463, #51795 ) ) ;
#58922 = ORIENTED_EDGE ( 'NONE', *, *, #8757, .T. ) ;
#58923 = CARTESIAN_POINT ( 'NONE',  ( -57.52287095715005449, -29.50250243563736774, 8.947779886222145151 ) ) ;
#58924 = LINE ( 'NONE', #49325, #92344 ) ;
#58925 = ORIENTED_EDGE ( 'NONE', *, *, #41518, .F. ) ;
#58926 = ORIENTED_EDGE ( 'NONE', *, *, #39031, .F. ) ;
#58927 = VERTEX_POINT ( 'NONE', #65255 ) ;
#58928 = CARTESIAN_POINT ( 'NONE',  ( -27.25988310792305214, -5.965225279485572685, 30.32664379231667695 ) ) ;
#58929 = CARTESIAN_POINT ( 'NONE',  ( -28.60235697241663999, -23.80516273491463508, 10.65365253163527015 ) ) ;
#58930 = LINE ( 'NONE', #89872, #64944 ) ;
#58931 = CARTESIAN_POINT ( 'NONE',  ( -18.78340662496949776, 8.880393494302802893, -1.500000000000002220 ) ) ;
#58932 = CARTESIAN_POINT ( 'NONE',  ( 8.489507321284875729, -19.98171680480944445, 11.49999999999999645 ) ) ;
#58933 = ORIENTED_EDGE ( 'NONE', *, *, #81386, .T. ) ;
#58934 = CIRCLE ( 'NONE', #33010, 4.299999999999999822 ) ;
#58935 = CARTESIAN_POINT ( 'NONE',  ( -40.33243357995862510, -25.18556298990670683, 3.298389014606699643 ) ) ;
#58936 = EDGE_CURVE ( 'NONE', #41375, #48360, #96180, .T. ) ;
#58937 = DIRECTION ( 'NONE',  ( 0.000000000000000000, -1.000000000000000000, 0.000000000000000000 ) ) ;
#58938 = DIRECTION ( 'NONE',  ( 0.000000000000000000, 1.000000000000000000, -0.000000000000000000 ) ) ;
#58939 = CARTESIAN_POINT ( 'NONE',  ( -22.05133119090760019, 4.102169094691678453, 11.49999999999998934 ) ) ;
#58940 = ADVANCED_FACE ( 'NONE', ( #21522 ), #76307, .T. ) ;
#58941 = EDGE_CURVE ( 'NONE', #18541, #32116, #29150, .T. ) ;
#58942 = CARTESIAN_POINT ( 'NONE',  ( -41.52287095715006870, -24.64898659630528144, 1.056161002820819261 ) ) ;
#58943 = CARTESIAN_POINT ( 'NONE',  ( -34.62287095715007013, -23.47596703998600276, 11.44779298504227505 ) ) ;
#58944 = VERTEX_POINT ( 'NONE', #83936 ) ;
#58945 = DIRECTION ( 'NONE',  ( -0.000000000000000000, 0.000000000000000000, 1.000000000000000000 ) ) ;
#58946 = CARTESIAN_POINT ( 'NONE',  ( 12.09245314707524876, -4.658029312750951334, -27.52981586573924488 ) ) ;
#58947 = B_SPLINE_CURVE_WITH_KNOTS ( 'NONE', 3,
 ( #65681, #50433, #4756, #35709, #27093, #3274 ),
 .UNSPECIFIED., .F., .F.,
 ( 4, 2, 4 ),
 ( 1.570755371634131319E-05, 0.001396183895866090138, 0.002776660238015839048 ),
 .UNSPECIFIED. ) ;
#58948 = CIRCLE ( 'NONE', #57372, 1.000000000000000444 ) ;
#58949 = EDGE_CURVE ( 'NONE', #40969, #7626, #13916, .T. ) ;
#58950 = ORIENTED_EDGE ( 'NONE', *, *, #96456, .T. ) ;
#58951 = ORIENTED_EDGE ( 'NONE', *, *, #5597, .F. ) ;
#58952 = DIRECTION ( 'NONE',  ( 0.000000000000000000, -0.9999999999976377785, -2.173523156925979128E-06 ) ) ;
#58953 = ORIENTED_EDGE ( 'NONE', *, *, #71330, .T. ) ;
#58954 = CARTESIAN_POINT ( 'NONE',  ( 20.49606604269246546, -5.804284187783010474, -1.500000000000002220 ) ) ;
#58955 = ORIENTED_EDGE ( 'NONE', *, *, #35892, .T. ) ;
#58956 = LINE ( 'NONE', #13752, #77017 ) ;
#58957 = CARTESIAN_POINT ( 'NONE',  ( 13.92123049006271707, -16.85212209846622855, -1.500000000000002220 ) ) ;
#58958 = CARTESIAN_POINT ( 'NONE',  ( -38.52287095715006160, -24.33927499327854349, 9.819080762295811837 ) ) ;
#58959 = CARTESIAN_POINT ( 'NONE',  ( 19.36006514395606004, 11.85157241509795512, -1.500000000000002220 ) ) ;
#58960 = CARTESIAN_POINT ( 'NONE',  ( -41.09701627025020088, -25.28892465612891627, 3.494173594328332300 ) ) ;
#58961 = CARTESIAN_POINT ( 'NONE',  ( 22.81105451610979173, -1.475225279485572916, -18.46691820600746681 ) ) ;
#58962 = CARTESIAN_POINT ( 'NONE',  ( -19.33260374144687077, -10.33727041909969380, -1.500000000000002220 ) ) ;
#58963 = CARTESIAN_POINT ( 'NONE',  ( -66.62287095715002749, -23.73907113216991860, -1.053371485793230811 ) ) ;
#58964 = VERTEX_POINT ( 'NONE', #22017 ) ;
#58965 = B_SPLINE_CURVE_WITH_KNOTS ( 'NONE', 3,
 ( #43301, #66158, #96085, #97073, #79846, #11834 ),
 .UNSPECIFIED., .F., .F.,
 ( 4, 2, 4 ),
 ( 0.000000000000000000, 0.001380764517853248817, 0.002761529035706497635 ),
 .UNSPECIFIED. ) ;
#58966 = CARTESIAN_POINT ( 'NONE',  ( -122.5906892354238806, -23.96169478059714564, 10.65365249895717170 ) ) ;
#58968 = EDGE_CURVE ( 'NONE', #60035, #38301, #38099, .T. ) ;
#58967 = DIRECTION ( 'NONE',  ( -3.773278334453080206E-23, 0.9999999999976377785, 2.173523156925979975E-06 ) ) ;
#58969 = ADVANCED_FACE ( 'NONE', ( #6315 ), #10933, .T. ) ;
#58970 = ORIENTED_EDGE ( 'NONE', *, *, #65563, .F. ) ;
#58971 = CARTESIAN_POINT ( 'NONE',  ( -49.52287095715006160, -23.48786465467241769, 11.44779295918255002 ) ) ;
#58972 = DIRECTION ( 'NONE',  ( -3.773278334453079618E-23, 0.9999999999976377785, 2.173523156925979975E-06 ) ) ;
#58973 = CARTESIAN_POINT ( 'NONE',  ( -10.23455669472452101, -23.17852390460462786, 1.363349870542264863 ) ) ;
#58974 = CARTESIAN_POINT ( 'NONE',  ( -20.53569570583907122, -5.550916044964551155, 11.49999999999998934 ) ) ;
#58975 = CARTESIAN_POINT ( 'NONE',  ( -112.5891746945082446, -24.34968618360934656, 0.1864209137779000991 ) ) ;
#58976 = CARTESIAN_POINT ( 'NONE',  ( -26.09636659181000695, -24.75186549494400623, 4.940288025096378099 ) ) ;
#58977 = EDGE_CURVE ( 'NONE', #75868, #7254, #9059, .T. ) ;
#58978 = FACE_OUTER_BOUND ( 'NONE', #96611, .T. ) ;
#58979 = CARTESIAN_POINT ( 'NONE',  ( -68.54060897849606704, -24.51314013834315375, 0.6176544820404119562 ) ) ;
#58980 = B_SPLINE_CURVE_WITH_KNOTS ( 'NONE', 3,
 ( #30608, #83395, #21484, #99603 ),
 .UNSPECIFIED., .F., .F.,
 ( 4, 4 ),
 ( 0.000000000000000000, 9.999999999998900014E-05 ),
 .UNSPECIFIED. ) ;
#58981 = AXIS2_PLACEMENT_3D ( 'NONE', #85689, #48649, #55757 ) ;
#58982 = ADVANCED_FACE ( 'NONE', ( #36771 ), #5314, .T. ) ;
#58983 = CARTESIAN_POINT ( 'NONE',  ( -117.6294113641524604, -23.48786465467241769, 11.44779295918253581 ) ) ;
#58984 = EDGE_LOOP ( 'NONE', ( #35710, #76382, #53181, #83496 ) ) ;
#58985 = CARTESIAN_POINT ( 'NONE',  ( -12.82114019720147802, -14.77593736753402709, 11.49999999999999645 ) ) ;
#58986 = FACE_OUTER_BOUND ( 'NONE', #71802, .T. ) ;
#58987 = AXIS2_PLACEMENT_3D ( 'NONE', #35408, #83045, #52121 ) ;
#58988 = CARTESIAN_POINT ( 'NONE',  ( -28.89879952236138294, -24.84188620179533302, 7.830688885502556928 ) ) ;
#58989 = EDGE_LOOP ( 'NONE', ( #44019, #48286, #38601, #15756 ) ) ;
#58990 = EDGE_CURVE ( 'NONE', #82250, #76858, #36913, .T. ) ;
#58991 = CARTESIAN_POINT ( 'NONE',  ( 3.797776442307698286, -6.376774720514427841, 21.83974358974358410 ) ) ;
#58992 = CARTESIAN_POINT ( 'NONE',  ( -99.30277203926080176, -25.31439712689208577, 6.024134105486370849 ) ) ;
#58994 = ADVANCED_FACE ( 'NONE', ( #12918 ), #7302, .T. ) ;
#58993 = CARTESIAN_POINT ( 'NONE',  ( -31.62287095715005236, -23.94994826722514958, -0.6494450866351750840 ) ) ;
#58995 = CARTESIAN_POINT ( 'NONE',  ( -106.5228709571500616, -23.73907113216990794, -1.053371485793244577 ) ) ;
#58996 = CARTESIAN_POINT ( 'NONE',  ( 19.47230031930329730, 2.946587627359682493, -1.500000000000002220 ) ) ;
#58997 = EDGE_CURVE ( 'NONE', #6989, #77894, #2101, .T. ) ;
#58998 = ORIENTED_EDGE ( 'NONE', *, *, #15633, .T. ) ;
#58999 = B_SPLINE_CURVE_WITH_KNOTS ( 'NONE', 3,
 ( #34077, #65050, #95967, #86189 ),
 .UNSPECIFIED., .F., .F.,
 ( 4, 4 ),
 ( 0.8794099815877536308, 0.8804107286285189904 ),
 .UNSPECIFIED. ) ;
#59000 = CARTESIAN_POINT ( 'NONE',  ( -109.5228709571500474, -23.48783264082477018, -1.443836473390083253 ) ) ;
#59001 = CARTESIAN_POINT ( 'NONE',  ( 8.971512145086524725, -7.528487854913504584, -6.499999999999999112 ) ) ;
#59003 = ADVANCED_FACE ( 'NONE', ( #71604 ), #41661, .T. ) ;
#59002 = PERSON_AND_ORGANIZATION_ROLE ( 'creator' ) ;
#59004 = EDGE_LOOP ( 'NONE', ( #27504, #91887, #97942, #13371 ) ) ;
#59005 = CARTESIAN_POINT ( 'NONE',  ( -74.52287095715007581, -24.34917612406836795, 0.1852690917426520756 ) ) ;
#59006 = CARTESIAN_POINT ( 'NONE',  ( -69.52287095715003318, -24.66019654487199375, 8.947790411086119278 ) ) ;
#59007 = CARTESIAN_POINT ( 'NONE',  ( -47.58190297339098151, -24.51314013834316086, 0.6176544820404172853 ) ) ;
#59008 = CARTESIAN_POINT ( 'NONE',  ( -50.58953762381673158, -24.99156044556120193, 7.747789690856343725 ) ) ;
#59009 = CARTESIAN_POINT ( 'NONE',  ( -7.312991930324885814, -6.376774720514413630, 20.02088365235844947 ) ) ;
#59010 = CARTESIAN_POINT ( 'NONE',  ( -99.62287095715005592, -23.48786465467241769, 11.44779295918254114 ) ) ;
#59011 = DIRECTION ( 'NONE',  ( -0.000000000000000000, -1.000000000000000000, -0.000000000000000000 ) ) ;
#59012 = CARTESIAN_POINT ( 'NONE',  ( -11.44242300287478820, -16.35863574123370512, 11.49999999999998934 ) ) ;
#59013 = VECTOR ( 'NONE', #4000, 1000.000000000000000 ) ;
#59014 = LINE ( 'NONE', #28538, #4608 ) ;
#59015 = CARTESIAN_POINT ( 'NONE',  ( -0.08050249797735845037, -22.00783190155722480, 0.02034857451668616729 ) ) ;
#59016 = VERTEX_POINT ( 'NONE', #80710 ) ;
#59017 = CARTESIAN_POINT ( 'NONE',  ( -29.52287095715005805, -23.64127125214882597, -1.053577532865616950 ) ) ;
#59018 = CARTESIAN_POINT ( 'NONE',  ( -63.52287095715006160, -24.64965694238575011, 8.947790433994201820 ) ) ;
#59019 = VECTOR ( 'NONE', #91972, 1000.000000000000000 ) ;
#59020 =( LENGTH_UNIT ( ) NAMED_UNIT ( * ) SI_UNIT ( .MILLI., .METRE. ) );
#59021 = CARTESIAN_POINT ( 'NONE',  ( 9.002841642506252740, -6.376774720514426065, -25.01329513651794656 ) ) ;
#59022 = CYLINDRICAL_SURFACE ( 'NONE', #78528, 1.000000000000000888 ) ;
#59023 = CARTESIAN_POINT ( 'NONE',  ( -81.58510886217409563, -24.51314013834316796, 0.6176544820404249458 ) ) ;
#59024 = CARTESIAN_POINT ( 'NONE',  ( -75.22287095715006444, -23.47593901973090169, -1.443836447538997536 ) ) ;
#59025 = FACE_OUTER_BOUND ( 'NONE', #82087, .T. ) ;
#59026 = ORIENTED_EDGE ( 'NONE', *, *, #40204, .F. ) ;
#59027 = CARTESIAN_POINT ( 'NONE',  ( -108.5228709571500616, -24.64965694238408034, 8.947790433994192938 ) ) ;
#59028 = DIRECTION ( 'NONE',  ( 0.06975647374412549673, 0.9975640502598241977, 0.000000000000000000 ) ) ;
#59029 = VERTEX_POINT ( 'NONE', #88324 ) ;
#59030 = CARTESIAN_POINT ( 'NONE',  ( 8.375906630400100639, -18.44307005126401933, 11.49999999999998934 ) ) ;
#59031 = CARTESIAN_POINT ( 'NONE',  ( -68.94158059132026040, -25.26655430154058735, 6.097253937284948577 ) ) ;
#59032 = CARTESIAN_POINT ( 'NONE',  ( 15.14080536460164517, 5.152774720514427642, -26.62908960815038384 ) ) ;
#59033 = CARTESIAN_POINT ( 'NONE',  ( -109.6228709571500275, -24.50216790748098816, 0.6166512839513658140 ) ) ;
#59034 = ORIENTED_EDGE ( 'NONE', *, *, #19892, .F. ) ;
#59035 = CARTESIAN_POINT ( 'NONE',  ( -77.52287095715006160, -24.64965694238575011, 8.947790433994198267 ) ) ;
#59036 = CARTESIAN_POINT ( 'NONE',  ( -24.90875734969025501, -5.356774720514425603, 26.43402280011862615 ) ) ;
#59037 = CARTESIAN_POINT ( 'NONE',  ( -14.83682921977595548, 13.52632505182701017, -1.500000000000002220 ) ) ;
#59038 = CARTESIAN_POINT ( 'NONE',  ( -20.11743356864677423, -6.099313207006018089, 11.49999999999999645 ) ) ;
#59039 = PLANE ( 'NONE',  #32394 ) ;
#59040 = CARTESIAN_POINT ( 'NONE',  ( -70.53412792675530341, -24.92592662359561118, 8.075495903017998245 ) ) ;
#59041 = CARTESIAN_POINT ( 'NONE',  ( -2.767897998228395551, 21.91458177938747909, 11.49999999999998934 ) ) ;
#59042 = CARTESIAN_POINT ( 'NONE',  ( -60.45647255754339966, -25.29664575297535833, 6.028421396434780810 ) ) ;
#59043 = EDGE_CURVE ( 'NONE', #56992, #83990, #73225, .T. ) ;
#59044 = DIRECTION ( 'NONE',  ( -0.000000000000000000, 1.000000000000000000, -0.000000000000000000 ) ) ;
#59045 = FACE_OUTER_BOUND ( 'NONE', #91266, .T. ) ;
#59046 = ORIENTED_EDGE ( 'NONE', *, *, #22669, .F. ) ;
#59047 = CARTESIAN_POINT ( 'NONE',  ( -35.52287095715007581, -24.83620972994591014, 8.398175272781369216 ) ) ;
#59048 = B_SPLINE_SURFACE_WITH_KNOTS ( 'NONE', 3, 1, ( 
 ( #72520, #10607 ),
 ( #3012, #63927 ),
 ( #25330, #86232 ),
 ( #32445, #9608 ),
 ( #80117, #41572 ),
 ( #47682, #24328 ),
 ( #79615, #78597 ),
 ( #54795, #71018 ),
 ( #55300, #86728 ),
 ( #70509, #47180 ),
 ( #85730, #78099 ) ),
 .UNSPECIFIED., .F., .F., .F.,
 ( 4, 1, 1, 1, 1, 1, 1, 1, 4 ),
 ( 2, 2 ),
 ( 0.000000000000000000, 0.1281355097972514123, 0.2541727119019812631, 0.3781116451390049149, 0.5017122630072827771, 0.6239863093684839823, 0.7470956136177411278, 0.8728746366500607090, 1.000000000000000000 ),
 ( 0.000000000000000000, 1.000000000000000000 ),
 .UNSPECIFIED. ) ;
#59049 = CARTESIAN_POINT ( 'NONE',  ( -40.62287095715004170, -29.50249982740957577, 7.747779886224967605 ) ) ;
#59050 = EDGE_CURVE ( 'NONE', #61038, #36448, #47887, .T. ) ;
#59051 = ORIENTED_EDGE ( 'NONE', *, *, #54601, .T. ) ;
#59052 = B_SPLINE_CURVE_WITH_KNOTS ( 'NONE', 3,
 ( #61194, #22091, #53074, #84002 ),
 .UNSPECIFIED., .F., .F.,
 ( 4, 4 ),
 ( 0.000000000000000000, 9.999999999996123101E-05 ),
 .UNSPECIFIED. ) ;
#59053 = ORIENTED_EDGE ( 'NONE', *, *, #56612, .T. ) ;
#59054 = CARTESIAN_POINT ( 'NONE',  ( -83.55620429048339304, -24.65952944569304606, 1.056160979905699904 ) ) ;
#59055 = CARTESIAN_POINT ( 'NONE',  ( 13.91401389203221406, 6.475225279485573360, 158.0376437107427137 ) ) ;
#59056 = CARTESIAN_POINT ( 'NONE',  ( -6.660000000000001030, 1.527978830621527617, 4.717155776778118259 ) ) ;
#59057 = CARTESIAN_POINT ( 'NONE',  ( -11.90445915685808131, 16.78794160864392992, -1.500000000000002220 ) ) ;
#59058 = EDGE_CURVE ( 'NONE', #50681, #60699, #64014, .T. ) ;
#59059 = CARTESIAN_POINT ( 'NONE',  ( 20.98156868870745484, 4.911575462371418510, 11.49999999999999645 ) ) ;
#59060 = ORIENTED_EDGE ( 'NONE', *, *, #54274, .T. ) ;
#59061 = CARTESIAN_POINT ( 'NONE',  ( -91.62357778056286861, -24.65952944569304606, 1.056160979905701680 ) ) ;
#59062 = CARTESIAN_POINT ( 'NONE',  ( -28.98875734969026041, -5.965225279485572685, 25.61802280011862720 ) ) ;
#59063 = DIRECTION ( 'NONE',  ( -1.000000000000000000, 0.000000000000000000, -7.994117400814786717E-16 ) ) ;
#59064 = CARTESIAN_POINT ( 'NONE',  ( 7.974090105135403839, 20.87195307945309963, 11.49999999999998934 ) ) ;
#59065 = ADVANCED_FACE ( 'NONE', ( #24908 ), #54001, .T. ) ;
#59066 = EDGE_CURVE ( 'NONE', #79629, #82392, #48266, .T. ) ;
#59067 = CARTESIAN_POINT ( 'NONE',  ( 8.971512145086499856, -1.028487854913501032, 5.500000000000000000 ) ) ;
#59068 = CARTESIAN_POINT ( 'NONE',  ( -124.6228709571500559, -23.73907113216991860, -1.053371485793223705 ) ) ;
#59069 = ORIENTED_EDGE ( 'NONE', *, *, #34616, .F. ) ;
#59070 = CARTESIAN_POINT ( 'NONE',  ( 27.53860345374784657, 4.772774720514425972, -8.321925749325748356 ) ) ;
#59071 = CARTESIAN_POINT ( 'NONE',  ( -48.52287095715006160, -23.47596703998600631, 11.44779298504229104 ) ) ;
#59072 = ADVANCED_FACE ( 'NONE', ( #94929 ), #87823, .F. ) ;
#59073 = CARTESIAN_POINT ( 'NONE',  ( 17.92008016455634589, 10.74458801173053324, -1.500000000000002220 ) ) ;
#59074 = ORIENTED_EDGE ( 'NONE', *, *, #12078, .F. ) ;
#59075 = CIRCLE ( 'NONE', #13631, 2.249999999999998668 ) ;
#59077 = VERTEX_POINT ( 'NONE', #80207 ) ;
#59076 = CARTESIAN_POINT ( 'NONE',  ( 32.53346577320679245, -2.682774720514426559, -11.93731717363830747 ) ) ;
#59078 = ORIENTED_EDGE ( 'NONE', *, *, #31919, .F. ) ;
#59079 = CARTESIAN_POINT ( 'NONE',  ( -51.29485095150216978, -25.26813275791670321, 4.047404401365850113 ) ) ;
#59080 = CARTESIAN_POINT ( 'NONE',  ( 19.19679251752027227, 8.867671107084703408, -1.500000000000002220 ) ) ;
#59081 = ORIENTED_EDGE ( 'NONE', *, *, #23641, .T. ) ;
#59082 = CARTESIAN_POINT ( 'NONE',  ( -28.52287095715005805, -29.50248528299880846, 1.056150804693231082 ) ) ;
#59083 = CARTESIAN_POINT ( 'NONE',  ( -98.58953762381672448, -23.48783264082478439, -1.443836473390061936 ) ) ;
#59084 = CARTESIAN_POINT ( 'NONE',  ( -48.62287095715007013, -24.51387760970723662, 9.387446482453421837 ) ) ;
#59085 = CYLINDRICAL_SURFACE ( 'NONE', #53406, 0.2500000000000011102 ) ;
#59086 = CARTESIAN_POINT ( 'NONE',  ( -80.62287095715005592, -29.50249982740957577, 7.747779886224967605 ) ) ;
#59087 = CARTESIAN_POINT ( 'NONE',  ( -19.96617879207914825, 8.700599545123990808, -1.500000000000002220 ) ) ;
#59088 = CARTESIAN_POINT ( 'NONE',  ( -80.40733119250255356, -25.04327900430719112, 7.562221853552162365 ) ) ;
#59090 = ORIENTED_EDGE ( 'NONE', *, *, #47190, .F. ) ;
#59089 = CARTESIAN_POINT ( 'NONE',  ( -18.01732314745861530, 13.19606014829601826, 11.49999999999999645 ) ) ;
#59091 = DIRECTION ( 'NONE',  ( -1.000000000000000000, 0.000000000000000000, -0.000000000000000000 ) ) ;
#59092 = DIRECTION ( 'NONE',  ( 0.000000000000000000, -1.000000000000000000, 0.000000000000000000 ) ) ;
#59093 = EDGE_CURVE ( 'NONE', #41820, #92347, #82912, .T. ) ;
#59094 = CARTESIAN_POINT ( 'NONE',  ( -43.62287095715004881, -29.50247984919015209, -1.443849546365060466 ) ) ;
#59095 = ORIENTED_EDGE ( 'NONE', *, *, #66917, .F. ) ;
#59096 = VECTOR ( 'NONE', #61416, 1000.000000000000114 ) ;
#59097 = ORIENTED_EDGE ( 'NONE', *, *, #51988, .T. ) ;
#59098 = EDGE_CURVE ( 'NONE', #63837, #91326, #56392, .T. ) ;
#59099 = ORIENTED_EDGE ( 'NONE', *, *, #48669, .T. ) ;
#59100 = CARTESIAN_POINT ( 'NONE',  ( -100.7773612853930416, -25.13940139968743281, 7.065664229807540053 ) ) ;
#59101 = B_SPLINE_CURVE_WITH_KNOTS ( 'NONE', 3,
 ( #89929, #35651, #99020, #44262 ),
 .UNSPECIFIED., .F., .F.,
 ( 4, 4 ),
 ( 0.000000000000000000, 9.999999999998206125E-05 ),
 .UNSPECIFIED. ) ;
#59102 = CARTESIAN_POINT ( 'NONE',  ( -128.2228709571500644, -23.47593901973090524, -1.443836447538996204 ) ) ;
#59103 = DIRECTION ( 'NONE',  ( -1.000000000000000000, -3.773278334444166432E-23, -8.201307841325785021E-29 ) ) ;
#59104 = LINE ( 'NONE', #42879, #19423 ) ;
#59105 = CARTESIAN_POINT ( 'NONE',  ( -87.52287095715006160, -24.64965694238575011, 8.947790433994196491 ) ) ;
#59106 = DIRECTION ( 'NONE',  ( 0.000000000000000000, 0.000000000000000000, 1.000000000000000000 ) ) ;
#59107 = ORIENTED_EDGE ( 'NONE', *, *, #64036, .F. ) ;
#59108 = CARTESIAN_POINT ( 'NONE',  ( 19.38287969867323213, 0.6573286442255052986, 11.49999999999999645 ) ) ;
#59109 = FACE_OUTER_BOUND ( 'NONE', #75742, .T. ) ;
#59110 = EDGE_LOOP ( 'NONE', ( #76989, #5745, #58453, #66060 ) ) ;
#59111 = DIRECTION ( 'NONE',  ( -0.000000000000000000, 2.173523156925979552E-06, -0.9999999999976378895 ) ) ;
#59112 = CARTESIAN_POINT ( 'NONE',  ( 8.476323908314187250, 3.316774720514010788, -27.09030197646909599 ) ) ;
#59113 = FACE_OUTER_BOUND ( 'NONE', #70248, .T. ) ;
#59115 = EDGE_CURVE ( 'NONE', #97841, #77005, #75488, .T. ) ;
#59114 = CARTESIAN_POINT ( 'NONE',  ( -130.5728709571500588, -23.47596703998600631, 11.44779298504227860 ) ) ;
#59116 = CARTESIAN_POINT ( 'NONE',  ( 11.71876819965036809, 15.69520123712499249, -1.500000000000002220 ) ) ;
#59117 = DIRECTION ( 'NONE',  ( -0.000000000000000000, -1.000000000000000000, -0.000000000000000000 ) ) ;
#59118 = ORIENTED_EDGE ( 'NONE', *, *, #62372, .T. ) ;
#59119 = AXIS2_PLACEMENT_3D ( 'NONE', #98523, #69468, #54258 ) ;
#59120 = CARTESIAN_POINT ( 'NONE',  ( -14.38888013576714719, -16.06800976983558726, 11.49999999999998934 ) ) ;
#59121 = CARTESIAN_POINT ( 'NONE',  ( -86.22287095715007865, -23.47596703998600631, 11.44779298504227860 ) ) ;
#59122 = CARTESIAN_POINT ( 'NONE',  ( -108.9545715455115129, -29.50249205131699526, 4.170135655464190627 ) ) ;
#59123 = CARTESIAN_POINT ( 'NONE',  ( -40.61244325972609914, -23.85016227208580730, -0.8807180028928393023 ) ) ;
#59124 = EDGE_CURVE ( 'NONE', #23703, #87143, #2598, .T. ) ;
#59125 = LINE ( 'NONE', #90060, #98999 ) ;
#59126 = CARTESIAN_POINT ( 'NONE',  ( 2.177599385301639323, -22.86303409451243596, -1.500000000000002220 ) ) ;
#59127 = PERSON_AND_ORGANIZATION ( #70597, #27821 ) ;
#59128 = CARTESIAN_POINT ( 'NONE',  ( -4.568292318365942073, -0.3587747205144265483, 30.06720597538392425 ) ) ;
#59129 = CARTESIAN_POINT ( 'NONE',  ( -49.49675345401667670, -25.29249258120279009, 4.255736650380444352 ) ) ;
#59130 = CARTESIAN_POINT ( 'NONE',  ( -3.510519812331947875, -19.85243952969433323, 11.49999999999999645 ) ) ;
#59131 = DIRECTION ( 'NONE',  ( 0.000000000000000000, 0.000000000000000000, 1.000000000000000000 ) ) ;
#59132 = DIRECTION ( 'NONE',  ( -9.527529159155689202E-17, 4.297590679709308564E-16, 1.000000000000000000 ) ) ;
#59133 = DIRECTION ( 'NONE',  ( -1.000000000000000000, 0.000000000000000000, 0.000000000000000000 ) ) ;
#59134 = LINE ( 'NONE', #99651, #50481 ) ;
#59135 = DIRECTION ( 'NONE',  ( 1.000000000000000000, 0.000000000000000000, 0.000000000000000000 ) ) ;
#59136 = CARTESIAN_POINT ( 'NONE',  ( -10.37884456512175291, 16.95428827495986823, -1.500000000000002220 ) ) ;
#59137 = CARTESIAN_POINT ( 'NONE',  ( -113.6235175983584753, -24.65952944569305316, 1.056160979905705011 ) ) ;
#59138 = CARTESIAN_POINT ( 'NONE',  ( 17.76913753361954562, 8.601950719843506121, -1.500000000000002220 ) ) ;
#59139 = CARTESIAN_POINT ( 'NONE',  ( 31.79364159983995464, 6.376774720514426953, -11.59305536555894278 ) ) ;
#59140 = CARTESIAN_POINT ( 'NONE',  ( -22.05275734969026047, 0.3587747205144262708, 31.02402280011862246 ) ) ;
#59141 = LINE ( 'NONE', #81479, #54022 ) ;
#59142 = CARTESIAN_POINT ( 'NONE',  ( -1.398219401198234957, 20.63772364298462847, 11.49999999999999645 ) ) ;
#59143 = CARTESIAN_POINT ( 'NONE',  ( -39.26664729043937996, -25.31628629975991984, 5.049946001168161835 ) ) ;
#59144 = VECTOR ( 'NONE', #70877, 1000.000000000000114 ) ;
#59145 = CARTESIAN_POINT ( 'NONE',  ( -2.499999999999993339, 18.99999999999977618, 2.100000000000000089 ) ) ;
#59146 = CARTESIAN_POINT ( 'NONE',  ( 17.73637878876437668, -14.10177982315242318, 11.49999999999999645 ) ) ;
#59147 = ORIENTED_EDGE ( 'NONE', *, *, #72127, .T. ) ;
#59148 = CARTESIAN_POINT ( 'NONE',  ( -1.044639546681034536, -6.376774720514417183, 20.34213149456667580 ) ) ;
#59149 = CARTESIAN_POINT ( 'NONE',  ( 30.58729439590573307, 4.540774720514427543, 26.14186284044631492 ) ) ;
#59150 = DIRECTION ( 'NONE',  ( -3.773278334444167608E-23, 1.000000000000000000, 0.000000000000000000 ) ) ;
#59151 = AXIS2_PLACEMENT_3D ( 'NONE', #3777, #18981, #41845 ) ;
#59152 = FACE_OUTER_BOUND ( 'NONE', #1073, .T. ) ;
#59153 = ORIENTED_EDGE ( 'NONE', *, *, #16568, .F. ) ;
#59154 = VERTEX_POINT ( 'NONE', #25917 ) ;
#59155 = DIRECTION ( 'NONE',  ( -1.000000000000000000, -0.000000000000000000, -7.994117400814786717E-16 ) ) ;
#59156 = CARTESIAN_POINT ( 'NONE',  ( 0.7049041324096299022, -22.85584899170066109, -1.500000000000002220 ) ) ;
#59157 = CARTESIAN_POINT ( 'NONE',  ( -74.62287095715008434, -24.51283580621365132, 0.6167428607019774800 ) ) ;
#59158 = CARTESIAN_POINT ( 'NONE',  ( 19.98928912078053699, -8.061568661392884749, -1.500000000000002220 ) ) ;
#59159 = CARTESIAN_POINT ( 'NONE',  ( -92.52287095715006160, -29.50248528299804818, 1.056150453629040253 ) ) ;
#59160 = CARTESIAN_POINT ( 'NONE',  ( -71.52287095715007581, -24.64898659630528854, 1.056161002820824368 ) ) ;
#59161 = CARTESIAN_POINT ( 'NONE',  ( 17.82461400791848405, -13.82690402418615960, 11.49999999999999645 ) ) ;
#59162 = VERTEX_POINT ( 'NONE', #100128 ) ;
#59163 = CARTESIAN_POINT ( 'NONE',  ( -29.24566686208495625, -25.21112321003771584, 4.648180976733166325 ) ) ;
#59164 = CARTESIAN_POINT ( 'NONE',  ( 10.07166557822571207, 19.55152498600455857, -1.500000000000002220 ) ) ;
#59165 = FACE_OUTER_BOUND ( 'NONE', #22126, .T. ) ;
#59166 = DIRECTION ( 'NONE',  ( 0.09824042138329625029, 0.9951627101165079203, 3.504396110891627214E-15 ) ) ;
#59168 = ORIENTED_EDGE ( 'NONE', *, *, #28977, .F. ) ;
#59167 = EDGE_CURVE ( 'NONE', #23809, #89711, #87784, .T. ) ;
#59169 = CARTESIAN_POINT ( 'NONE',  ( -89.62287095715008434, -23.96177878511308990, 10.65340807706329862 ) ) ;
#59170 = DIRECTION ( 'NONE',  ( -3.773278334444167608E-23, 1.000000000000000000, 0.000000000000000000 ) ) ;
#59171 = ORIENTED_EDGE ( 'NONE', *, *, #49799, .F. ) ;
#59172 = CARTESIAN_POINT ( 'NONE',  ( -108.5562042904834072, -23.47593901973091235, -1.443836447538999312 ) ) ;
#59173 = EDGE_CURVE ( 'NONE', #80239, #75450, #10700, .T. ) ;
#59174 = ORIENTED_EDGE ( 'NONE', *, *, #22208, .T. ) ;
#59175 = VERTEX_POINT ( 'NONE', #97428 ) ;
#59176 = CARTESIAN_POINT ( 'NONE',  ( -10.59832330691884117, -0.3587747205144061757, -27.05373799718300987 ) ) ;
#59177 = DIRECTION ( 'NONE',  ( -3.773278334453079030E-23, 0.9999999999976377785, 2.173523156925979128E-06 ) ) ;
#59178 = CARTESIAN_POINT ( 'NONE',  ( 32.66876533700882845, -6.475225279485573360, -12.58926540598385557 ) ) ;
#59179 = B_SPLINE_CURVE_WITH_KNOTS ( 'NONE', 3,
 ( #94536, #72215, #56998, #8808, #54987, #85930 ),
 .UNSPECIFIED., .F., .F.,
 ( 4, 2, 4 ),
 ( 0.000000000000000000, 0.001380901958385382473, 0.002761803916770764946 ),
 .UNSPECIFIED. ) ;
#59180 = CARTESIAN_POINT ( 'NONE',  ( -1.067026067711715154, -20.38227831319515460, -1.500000000000002220 ) ) ;
#59181 = ADVANCED_FACE ( 'NONE', ( #3595 ), #4088, .T. ) ;
#59182 = VERTEX_POINT ( 'NONE', #74100 ) ;
#59183 = DIRECTION ( 'NONE',  ( 0.000000000000000000, 0.000000000000000000, 1.000000000000000000 ) ) ;
#59184 = CARTESIAN_POINT ( 'NONE',  ( -60.92287095715005307, -23.47593901973090169, -1.443836447538997536 ) ) ;
#59185 = EDGE_CURVE ( 'NONE', #67908, #13108, #91358, .T. ) ;
#59186 = FACE_OUTER_BOUND ( 'NONE', #43070, .T. ) ;
#59187 = CARTESIAN_POINT ( 'NONE',  ( -70.70237668956666255, -25.03149840991684982, 7.522646895911706544 ) ) ;
#59188 = ORIENTED_EDGE ( 'NONE', *, *, #96536, .T. ) ;
#59189 = LINE ( 'NONE', #91614, #53327 ) ;
#59190 = LINE ( 'NONE', #75389, #84779 ) ;
#59191 = EDGE_CURVE ( 'NONE', #25617, #27620, #5465, .T. ) ;
#59192 = VECTOR ( 'NONE', #62757, 1000.000000000000000 ) ;
#59193 = ORIENTED_EDGE ( 'NONE', *, *, #98965, .T. ) ;
#59194 = EDGE_CURVE ( 'NONE', #40854, #6116, #27219, .T. ) ;
#59195 = CARTESIAN_POINT ( 'NONE',  ( -3.686900873480770002, -20.48319827837541141, 11.49999999999998934 ) ) ;
#59196 = EDGE_LOOP ( 'NONE', ( #38096, #43259, #398, #45076 ) ) ;
#59198 = ORIENTED_EDGE ( 'NONE', *, *, #7999, .T. ) ;
#59197 = FACE_OUTER_BOUND ( 'NONE', #5255, .T. ) ;
#59199 = CARTESIAN_POINT ( 'NONE',  ( 13.91401389203221406, -0.3587747205144265483, 158.0376437107427137 ) ) ;
#59200 = DIRECTION ( 'NONE',  ( -1.000000000000000000, -3.773278334444166432E-23, -8.201307841325785021E-29 ) ) ;
#59201 = ORIENTED_EDGE ( 'NONE', *, *, #27889, .T. ) ;
#59202 = VERTEX_POINT ( 'NONE', #27426 ) ;
#59203 = CARTESIAN_POINT ( 'NONE',  ( -25.53098197642538736, -29.50249373072461623, 4.942801737957442931 ) ) ;
#59204 = CARTESIAN_POINT ( 'NONE',  ( 30.93860345374796594, 0.6647747205144264315, 19.84760796525321780 ) ) ;
#59205 = CARTESIAN_POINT ( 'NONE',  ( 9.150000000000000355, -5.876774720514426953, -15.70000000000000284 ) ) ;
#59206 = CARTESIAN_POINT ( 'NONE',  ( -43.65489518069405506, -23.73791477778911130, 11.05961554403171121 ) ) ;
#59208 = EDGE_LOOP ( 'NONE', ( #99348, #15100, #16690, #21994 ) ) ;
#59207 = CARTESIAN_POINT ( 'NONE',  ( -9.153499762860807465, 20.15527781828815534, 11.49999999999999645 ) ) ;
#59209 = CARTESIAN_POINT ( 'NONE',  ( -72.62287095715007013, -23.96127896941632685, -0.6493128931037881468 ) ) ;
#59210 = CARTESIAN_POINT ( 'NONE',  ( -7.157701736792966507, -21.45640540170154509, 11.49999999999998934 ) ) ;
#59212 = VERTEX_POINT ( 'NONE', #34539 ) ;
#59211 = CARTESIAN_POINT ( 'NONE',  ( -115.5902947577247346, -24.40133493613050675, 9.663955038902797057 ) ) ;
#59213 = EDGE_LOOP ( 'NONE', ( #54922, #100102, #53834, #75532 ) ) ;
#59214 = CARTESIAN_POINT ( 'NONE',  ( -10.12061615367207601, -3.718318319926830373, 30.49412484105965859 ) ) ;
#59215 = AXIS2_PLACEMENT_3D ( 'NONE', #33313, #79494, #86605 ) ;
#59216 = CARTESIAN_POINT ( 'NONE',  ( -78.62287095715005592, -23.47596703998600631, 11.44779298504227860 ) ) ;
#59217 = ORIENTED_EDGE ( 'NONE', *, *, #98144, .F. ) ;
#59218 = CARTESIAN_POINT ( 'NONE',  ( -89.52287095715006160, -24.35013146730203815, 9.818937971375097717 ) ) ;
#59219 = CARTESIAN_POINT ( 'NONE',  ( -17.34812393562427246, -13.96779696820907191, -1.500000000000002220 ) ) ;
#59220 = CARTESIAN_POINT ( 'NONE',  ( -121.5228709571500616, -29.50250243563736774, 8.947779886222134493 ) ) ;
#59221 = AXIS2_PLACEMENT_3D ( 'NONE', #98111, #20988, #83390 ) ;
#59222 = ORIENTED_EDGE ( 'NONE', *, *, #70788, .F. ) ;
#59223 = CARTESIAN_POINT ( 'NONE',  ( -2.704906987277317931, 6.376774720514425177, -28.92935364444904778 ) ) ;
#59224 = CARTESIAN_POINT ( 'NONE',  ( -80.59883725225060402, -25.03321342637004321, 7.561462816580968749 ) ) ;
#59225 = CARTESIAN_POINT ( 'NONE',  ( -28.98875734969026396, 5.965225279485572685, 7.870022800118628759 ) ) ;
#59226 = VECTOR ( 'NONE', #94217, 1000.000000000000000 ) ;
#59227 = CARTESIAN_POINT ( 'NONE',  ( -108.6228709571501128, -24.34917612406838217, 0.1852690917426704775 ) ) ;
#59228 = CARTESIAN_POINT ( 'NONE',  ( -65.62287095715005592, -29.50248528299804818, 1.056150453629036701 ) ) ;
#59229 = CARTESIAN_POINT ( 'NONE',  ( 5.544562197198338538, -18.70016399976332977, 11.49999999999998934 ) ) ;
#59230 = CARTESIAN_POINT ( 'NONE',  ( 19.78805588120126302, 8.271231038663975355, 11.49999999999998934 ) ) ;
#59231 = CARTESIAN_POINT ( 'NONE',  ( -0.8460708837923186509, -5.876774720514410077, 19.21968329462762526 ) ) ;
#59232 = CARTESIAN_POINT ( 'NONE',  ( 22.02124265030973760, -7.835183881457444599, 16.20402280011862217 ) ) ;
#59233 = CARTESIAN_POINT ( 'NONE',  ( -76.52287095715007581, -23.48786465467241769, 11.44779295918254469 ) ) ;
#59234 = EDGE_CURVE ( 'NONE', #52326, #4648, #78052, .T. ) ;
#59235 = CARTESIAN_POINT ( 'NONE',  ( -10.82450569625279613, 20.10975305113172951, -1.500000000000002220 ) ) ;
#59236 = EDGE_CURVE ( 'NONE', #96161, #78575, #51484, .T. ) ;
#59237 = DATE_AND_TIME ( #20161, #5150 ) ;
#59238 = CYLINDRICAL_SURFACE ( 'NONE', #14261, 2.249999999999998668 ) ;
#59239 = FACE_OUTER_BOUND ( 'NONE', #63928, .T. ) ;
#59240 = CARTESIAN_POINT ( 'NONE',  ( 4.608267332293128682, -19.41724391825443874, 11.49999999999999645 ) ) ;
#59241 = DIRECTION ( 'NONE',  ( -3.773278334444166432E-23, 1.000000000000000000, 0.000000000000000000 ) ) ;
#59242 = B_SPLINE_CURVE_WITH_KNOTS ( 'NONE', 3,
 ( #31060, #71531, #25841, #33959 ),
 .UNSPECIFIED., .F., .F.,
 ( 4, 4 ),
 ( 0.000000000000000000, 9.999999999998897304E-05 ),
 .UNSPECIFIED. ) ;
#59243 = CARTESIAN_POINT ( 'NONE',  ( -39.66519142177316581, -23.48786465467240703, 11.44779295918255002 ) ) ;
#59244 = B_SPLINE_CURVE_WITH_KNOTS ( 'NONE', 3,
 ( #45216, #5642, #29471, #76142, #84763, #15250 ),
 .UNSPECIFIED., .F., .F.,
 ( 4, 2, 4 ),
 ( 0.000000000000000000, 0.001380901958385387894, 0.002761803916770775788 ),
 .UNSPECIFIED. ) ;
#59245 = CARTESIAN_POINT ( 'NONE',  ( -101.6228709571500559, -23.94994826722515668, -0.6494450866351716423 ) ) ;
#59246 = ORIENTED_EDGE ( 'NONE', *, *, #46363, .T. ) ;
#59247 = CARTESIAN_POINT ( 'NONE',  ( -25.53615934357976869, -24.91998285861100371, 4.571435626871006797 ) ) ;
#59248 = DIRECTION ( 'NONE',  ( 0.000000000000000000, 0.000000000000000000, -1.000000000000000000 ) ) ;
#59249 = CARTESIAN_POINT ( 'NONE',  ( 3.708801897538985148, -21.39311272803122321, -1.500000000000002220 ) ) ;
#59250 = CARTESIAN_POINT ( 'NONE',  ( -77.52287095715006160, -24.66019654487200086, 8.947790411086113949 ) ) ;
#59251 = CARTESIAN_POINT ( 'NONE',  ( 18.00893756148942870, 7.586210683597776949, -1.500000000000002220 ) ) ;
#59252 = CARTESIAN_POINT ( 'NONE',  ( -99.31324271614009547, -25.24395871390426294, 6.321204267077806804 ) ) ;
#59253 = VERTEX_POINT ( 'NONE', #47886 ) ;
#59254 = COORDINATED_UNIVERSAL_TIME_OFFSET ( 0, 0, .AHEAD. ) ;
#59255 = VECTOR ( 'NONE', #60156, 1000.000000000000114 ) ;
#59256 = CARTESIAN_POINT ( 'NONE',  ( 12.16765770914787304, -5.965225279485572685, -27.57618308014988173 ) ) ;
#59257 = CARTESIAN_POINT ( 'NONE',  ( -110.6228709571500701, -24.92579138211019441, 1.929029949965667123 ) ) ;
#59258 = CARTESIAN_POINT ( 'NONE',  ( -10.82153711268468932, 17.32902648900640230, 11.49999999999999645 ) ) ;
#59259 = CARTESIAN_POINT ( 'NONE',  ( -49.28534510465767937, -25.26380556882021722, 6.011612785043525697 ) ) ;
#59260 = LINE ( 'NONE', #78960, #83693 ) ;
#59261 = EDGE_LOOP ( 'NONE', ( #26242, #89846, #23999, #39594 ) ) ;
#59262 = CARTESIAN_POINT ( 'NONE',  ( -51.62287095715005592, -23.47593901973091235, -1.443836447539009749 ) ) ;
#59263 = FACE_OUTER_BOUND ( 'NONE', #51834, .T. ) ;
#59264 = CARTESIAN_POINT ( 'NONE',  ( -20.27875734969026311, 7.743225279485574042, 24.00402280011862288 ) ) ;
#59265 = LINE ( 'NONE', #29803, #17634 ) ;
#59266 = VERTEX_POINT ( 'NONE', #41270 ) ;
#59267 = CARTESIAN_POINT ( 'NONE',  ( 5.641025641025643189, -6.376774720514420736, 20.78665865384615330 ) ) ;
#59268 = CARTESIAN_POINT ( 'NONE',  ( -22.84742429131147645, -2.885717679200183738, 11.49999999999999645 ) ) ;
#59269 = CARTESIAN_POINT ( 'NONE',  ( -22.16177213047534877, -5.259615592301647879, 11.49999999999998934 ) ) ;
#59270 = CARTESIAN_POINT ( 'NONE',  ( -10.11875734969026297, 5.965225279485572685, 30.51402280011862089 ) ) ;
#59271 = DIRECTION ( 'NONE',  ( 0.000000000000000000, 2.173523156925980399E-06, -0.9999999999976378895 ) ) ;
#59272 = CARTESIAN_POINT ( 'NONE',  ( -108.9545715455114987, -25.28708312187852414, 4.170144817753115518 ) ) ;
#59273 = CARTESIAN_POINT ( 'NONE',  ( -71.62287095715005592, -29.50250786944525672, 11.44777988621623699 ) ) ;
#59274 = CARTESIAN_POINT ( 'NONE',  ( -99.25999413675920380, -25.30157743809076720, 5.189783768456954327 ) ) ;
#59275 = CARTESIAN_POINT ( 'NONE',  ( -14.06357901826416068, -16.81340526219955933, -1.500000000000002220 ) ) ;
#59276 = FACE_OUTER_BOUND ( 'NONE', #29202, .T. ) ;
#59277 = VECTOR ( 'NONE', #11363, 1000.000000000000114 ) ;
#59278 = DIRECTION ( 'NONE',  ( 0.000000000000000000, 0.000000000000000000, 1.000000000000000000 ) ) ;
#59279 = CARTESIAN_POINT ( 'NONE',  ( -71.27032225721183067, -25.30598519668817303, 4.985731859564575430 ) ) ;
#59280 = CARTESIAN_POINT ( 'NONE',  ( -58.63776290787987477, -24.15543982623907127, -0.2315651400026660645 ) ) ;
#59281 = ORIENTED_EDGE ( 'NONE', *, *, #23176, .T. ) ;
#59282 = VECTOR ( 'NONE', #6655, 1000.000000000000114 ) ;
#59283 = EDGE_CURVE ( 'NONE', #69140, #13751, #99783, .T. ) ;
#59284 = CARTESIAN_POINT ( 'NONE',  ( 20.25987197511681259, 2.754759976156288204, 11.49999999999998934 ) ) ;
#59285 = ORIENTED_EDGE ( 'NONE', *, *, #54149, .F. ) ;
#59286 = CIRCLE ( 'NONE', #83607, 4.299999999999999822 ) ;
#59287 = EDGE_LOOP ( 'NONE', ( #46830, #38064, #61158, #30957 ) ) ;
#59288 = ORIENTED_EDGE ( 'NONE', *, *, #98913, .F. ) ;
#59289 = ORIENTED_EDGE ( 'NONE', *, *, #71467, .F. ) ;
#59290 = CARTESIAN_POINT ( 'NONE',  ( -16.13607370526515794, 16.44073208242836159, -1.500000000000002220 ) ) ;
#59291 = CARTESIAN_POINT ( 'NONE',  ( -63.62287095715004881, -24.66019654487199020, 8.947790411086131712 ) ) ;
#59292 = CARTESIAN_POINT ( 'NONE',  ( -20.17641613807547785, 1.360797614858565874, -1.500000000000002220 ) ) ;
#59293 = AXIS2_PLACEMENT_3D ( 'NONE', #87175, #56249, #49134 ) ;
#59294 = EDGE_CURVE ( 'NONE', #17515, #56546, #28455, .T. ) ;
#59295 = ORIENTED_EDGE ( 'NONE', *, *, #47078, .T. ) ;
#59296 = CARTESIAN_POINT ( 'NONE',  ( -98.62287095715008434, -24.50321055353806443, 9.387540953477520489 ) ) ;
#59297 = CARTESIAN_POINT ( 'NONE',  ( 6.316086099857336045, 1.335655600570672119, 18.31352460785937097 ) ) ;
#59298 = VECTOR ( 'NONE', #87872, 1000.000000000000227 ) ;
#59299 = ADVANCED_FACE ( 'NONE', ( #32647 ), #64637, .F. ) ;
#59300 = CARTESIAN_POINT ( 'NONE',  ( -101.5228709571501042, -24.35013146730203104, 9.818937971375097717 ) ) ;
#59301 = CARTESIAN_POINT ( 'NONE',  ( -99.58504437842513823, -24.66019654487200086, 8.947790411086115725 ) ) ;
#59303 = ORIENTED_EDGE ( 'NONE', *, *, #12334, .F. ) ;
#59302 = CARTESIAN_POINT ( 'NONE',  ( 9.988417798295188277, 18.97302403871600518, 11.49999999999999645 ) ) ;
#59304 = PLANE ( 'NONE',  #37089 ) ;
#59305 = ADVANCED_FACE ( 'NONE', ( #50886 ), #57511, .T. ) ;
#59306 = VERTEX_POINT ( 'NONE', #67118 ) ;
#59307 = CARTESIAN_POINT ( 'NONE',  ( 21.95989154999629278, -3.605859658025859282, -1.500000000000002220 ) ) ;
#59308 = EDGE_CURVE ( 'NONE', #34190, #53709, #46637, .T. ) ;
#59309 = CARTESIAN_POINT ( 'NONE',  ( 12.98984941077313415, -16.12360325096057423, -1.500000000000002220 ) ) ;
#59310 = VERTEX_POINT ( 'NONE', #98029 ) ;
#59311 = CARTESIAN_POINT ( 'NONE',  ( 3.750000000000001332, 25.69999999999999574, 2.100000000000000089 ) ) ;
#59312 = ORIENTED_EDGE ( 'NONE', *, *, #49814, .F. ) ;
#59313 = DIRECTION ( 'NONE',  ( 0.000000000000000000, 0.9999999999976377785, 2.173523156925979975E-06 ) ) ;
#59314 = ORIENTED_EDGE ( 'NONE', *, *, #29263, .T. ) ;
#59315 = CARTESIAN_POINT ( 'NONE',  ( 19.98859412959824411, 6.261702723725245612, -1.500000000000002220 ) ) ;
#59316 = EDGE_CURVE ( 'NONE', #34477, #46605, #16413, .T. ) ;
#59317 = CARTESIAN_POINT ( 'NONE',  ( -8.322136096487577461, -20.27582920440508829, 11.49999999999999645 ) ) ;
#59318 = CARTESIAN_POINT ( 'NONE',  ( -37.51295737854163548, -23.73791477778911130, 11.05961554403171299 ) ) ;
#59319 = CARTESIAN_POINT ( 'NONE',  ( -0.06565682164858396841, -22.51586213336150166, 11.49999999999998934 ) ) ;
#59320 = CARTESIAN_POINT ( 'NONE',  ( -7.049398010371669798, 19.71092172866906012, 11.49999999999998934 ) ) ;
#59321 = CARTESIAN_POINT ( 'NONE',  ( 6.273728352332436309, -5.876774720514415407, 20.10092598260902008 ) ) ;
#59322 = CARTESIAN_POINT ( 'NONE',  ( -91.58953762381672448, -23.48783264082478794, -1.443836473390063713 ) ) ;
#59323 = CARTESIAN_POINT ( 'NONE',  ( 5.766314450391940127, -6.376774720514424288, 21.17177008079512035 ) ) ;
#59324 = ORIENTED_EDGE ( 'NONE', *, *, #78333, .T. ) ;
#59325 = VERTEX_POINT ( 'NONE', #28527 ) ;
#59326 = ORIENTED_EDGE ( 'NONE', *, *, #24091, .F. ) ;
#59327 = CARTESIAN_POINT ( 'NONE',  ( -128.6228709571500417, -24.51387760970725083, 9.387446482453409402 ) ) ;
#59328 = CARTESIAN_POINT ( 'NONE',  ( -16.68621059303058018, 13.52761613308161870, -1.500000000000002220 ) ) ;
#59329 = CARTESIAN_POINT ( 'NONE',  ( -105.5228709571500758, -23.47596703998600631, 11.44779298504228038 ) ) ;
#59330 = VERTEX_POINT ( 'NONE', #59489 ) ;
#59331 = CARTESIAN_POINT ( 'NONE',  ( -16.97324839047195866, 12.58421825509937442, -1.500000000000002220 ) ) ;
#59332 = LINE ( 'NONE', #12648, #23847 ) ;
#59333 = CARTESIAN_POINT ( 'NONE',  ( -119.6228709571500559, -29.50250243563736774, 8.947779886222134493 ) ) ;
#59334 = CARTESIAN_POINT ( 'NONE',  ( 27.53860345374771867, 5.356774720514425603, -9.482392034746240483 ) ) ;
#59335 = CARTESIAN_POINT ( 'NONE',  ( 9.422519371942208011, 3.316774720514425567, -27.03574706870085720 ) ) ;
#59336 = LINE ( 'NONE', #29877, #85908 ) ;
#59337 = CARTESIAN_POINT ( 'NONE',  ( -7.692412698405892257, 20.70400481474656118, -1.500000000000002220 ) ) ;
#59338 = CARTESIAN_POINT ( 'NONE',  ( -81.58232365645901041, -24.66019654487198665, 8.947790411086131712 ) ) ;
#59339 = CARTESIAN_POINT ( 'NONE',  ( -51.92928322226379123, -25.31633332227261235, 6.080069373430273316 ) ) ;
#59340 = DIRECTION ( 'NONE',  ( -3.773278334453079618E-23, 0.9999999999976377785, 2.173523156925979975E-06 ) ) ;
#59341 = VECTOR ( 'NONE', #75447, 1000.000000000000000 ) ;
#59342 = EDGE_CURVE ( 'NONE', #68399, #87052, #90432, .T. ) ;
#59343 = CARTESIAN_POINT ( 'NONE',  ( -12.64432969575899968, -0.3587747205143967943, -26.13179214487285407 ) ) ;
#59344 = CARTESIAN_POINT ( 'NONE',  ( -14.39514105012195344, 13.04300321504834947, -1.500000000000002220 ) ) ;
#59345 = CARTESIAN_POINT ( 'NONE',  ( 4.555389213293416617, -20.86945110937667280, 11.49999999999998934 ) ) ;
#59346 = DIRECTION ( 'NONE',  ( 0.9903949459893286456, -0.09776975748869043414, 0.09776975748869007332 ) ) ;
#59347 = CARTESIAN_POINT ( 'NONE',  ( -50.91713042577481474, -25.30060005375479903, 6.009289253917323492 ) ) ;
#59348 = ADVANCED_FACE ( 'NONE', ( #43274 ), #20907, .T. ) ;
#59349 = CARTESIAN_POINT ( 'NONE',  ( -64.60984581131128834, -23.48786465467241058, 11.44779295918254824 ) ) ;
#59350 = CARTESIAN_POINT ( 'NONE',  ( -126.6228709571500843, -24.66019654487200441, 8.947790411086119278 ) ) ;
#59351 = CARTESIAN_POINT ( 'NONE',  ( 8.023449251107201974, -21.19570997880782670, -1.500000000000002220 ) ) ;
#59352 = VECTOR ( 'NONE', #6978, 1000.000000000000000 ) ;
#59353 = ORIENTED_EDGE ( 'NONE', *, *, #5909, .F. ) ;
#59354 = VECTOR ( 'NONE', #23086, 1000.000000000000227 ) ;
#59356 = CARTESIAN_POINT ( 'NONE',  ( -87.52287095715006160, -23.48786465467241058, 11.44779295918254292 ) ) ;
#59355 = B_SPLINE_CURVE_WITH_KNOTS ( 'NONE', 3,
 ( #52687, #60811, #13109, #22213, #84126, #35960 ),
 .UNSPECIFIED., .F., .F.,
 ( 4, 2, 4 ),
 ( 0.000000000000000000, 0.001380764517853256840, 0.002761529035706513681 ),
 .UNSPECIFIED. ) ;
#59357 = CARTESIAN_POINT ( 'NONE',  ( -69.92287095715005307, -23.47593901973090169, -1.443836447538997536 ) ) ;
#59358 = CARTESIAN_POINT ( 'NONE',  ( -11.05534852661189937, -16.44151763790470966, 11.49999999999999645 ) ) ;
#59359 = DIRECTION ( 'NONE',  ( -0.000000000000000000, 1.000000000000000000, -0.000000000000000000 ) ) ;
#59360 = AXIS2_PLACEMENT_3D ( 'NONE', #66694, #29089, #60063 ) ;
#59361 = DIRECTION ( 'NONE',  ( 0.9822594791677485837, 0.000000000000000000, -0.1875268396392986980 ) ) ;
#59362 = ORIENTED_EDGE ( 'NONE', *, *, #19667, .F. ) ;
#59363 = B_SPLINE_CURVE_WITH_KNOTS ( 'NONE', 3,
 ( #51856, #67095, #22367, #75661 ),
 .UNSPECIFIED., .F., .F.,
 ( 4, 4 ),
 ( 0.000000000000000000, 9.999999999998206125E-05 ),
 .UNSPECIFIED. ) ;
#59364 = AXIS2_PLACEMENT_3D ( 'NONE', #90919, #28516, #30009 ) ;
#59365 = CARTESIAN_POINT ( 'NONE',  ( -128.6228709571500417, -24.64965695001469115, 8.947790433994173398 ) ) ;
#59366 = CARTESIAN_POINT ( 'NONE',  ( -70.52287095715007581, -25.00182538069145366, 7.747789668545101094 ) ) ;
#59367 = CARTESIAN_POINT ( 'NONE',  ( -100.6597906528727577, -25.12268562698065111, 7.087518430423694227 ) ) ;
#59368 = CARTESIAN_POINT ( 'NONE',  ( -12.93760099376155104, 17.33828479246177423, -1.500000000000002220 ) ) ;
#59369 = CARTESIAN_POINT ( 'NONE',  ( -49.10668015502195516, -25.27518120313465033, 3.950017688817143213 ) ) ;
#59371 = CARTESIAN_POINT ( 'NONE',  ( -5.798782886354239885, 18.49141925852020663, -1.500000000000002220 ) ) ;
#59370 = AXIS2_PLACEMENT_3D ( 'NONE', #96328, #65908, #96823 ) ;
#59372 = DIRECTION ( 'NONE',  ( 1.000000000000000000, 3.491481338843132961E-15, 2.352173255807796056E-16 ) ) ;
#59373 = CARTESIAN_POINT ( 'NONE',  ( -82.62287095714999907, -23.96177878511307568, 10.65340807706330395 ) ) ;
#59374 = CARTESIAN_POINT ( 'NONE',  ( -12.28770250403618114, -15.54288071925545722, 11.49999999999998934 ) ) ;
#59375 = VERTEX_POINT ( 'NONE', #74215 ) ;
#59376 = CARTESIAN_POINT ( 'NONE',  ( 16.63042848490962555, -11.55671354112608817, 11.49999999999999645 ) ) ;
#59377 = CARTESIAN_POINT ( 'NONE',  ( -71.70841769935766763, -29.50249644799903592, 6.192972193920951440 ) ) ;
#59378 = B_SPLINE_CURVE_WITH_KNOTS ( 'NONE', 3,
 ( #81973, #49173, #1488, #10088 ),
 .UNSPECIFIED., .F., .F.,
 ( 4, 4 ),
 ( 0.8303788777084928352, 0.8393853089806082579 ),
 .UNSPECIFIED. ) ;
#59379 = PRODUCT_RELATED_PRODUCT_CATEGORY ( 'detail', '', ( #90652 ) ) ;
#59380 = CARTESIAN_POINT ( 'NONE',  ( -111.6228709571500559, -23.48783264082479505, -1.443836473390060604 ) ) ;
#59381 = ORIENTED_EDGE ( 'NONE', *, *, #40048, .T. ) ;
#59382 = LINE ( 'NONE', #42179, #76673 ) ;
#59383 = CARTESIAN_POINT ( 'NONE',  ( 31.60706529141452137, 4.540774720514427543, 26.12024523944105070 ) ) ;
#59384 = CARTESIAN_POINT ( 'NONE',  ( -99.62287095715005592, -23.48786465467241769, 11.44779295918254114 ) ) ;
#59385 = DIRECTION ( 'NONE',  ( 0.000000000000000000, 0.000000000000000000, 1.000000000000000000 ) ) ;
#59386 = CARTESIAN_POINT ( 'NONE',  ( -31.52287095715006160, -24.64965694238574656, 8.947790433994207149 ) ) ;
#59387 = CARTESIAN_POINT ( 'NONE',  ( -19.96166555454951208, -2.086822695551191043, 11.49999999999998934 ) ) ;
#59388 = DIRECTION ( 'NONE',  ( 0.000000000000000000, -1.000000000000000000, -1.224646799147353207E-16 ) ) ;
#59389 = ORIENTED_EDGE ( 'NONE', *, *, #21910, .F. ) ;
#59390 = AXIS2_PLACEMENT_3D ( 'NONE', #15030, #22631, #98265 ) ;
#59391 = CARTESIAN_POINT ( 'NONE',  ( -49.62307173802614102, -25.31297133582045333, 4.349864010778793144 ) ) ;
#59392 = DIRECTION ( 'NONE',  ( -2.352173255807804438E-16, 2.352173255807796056E-16, 1.000000000000000000 ) ) ;
#59393 = DIRECTION ( 'NONE',  ( 0.7512896232465891000, 0.000000000000000000, 0.6599726524652351767 ) ) ;
#59394 = CARTESIAN_POINT ( 'NONE',  ( -6.499999999999992895, -1.267509437117509414E-15, -2.500000000000001332 ) ) ;
#59395 = LINE ( 'NONE', #14201, #80278 ) ;
#59396 = CARTESIAN_POINT ( 'NONE',  ( 14.42577177192597482, -17.14957960503723911, 11.49999999999999645 ) ) ;
#59397 = DIRECTION ( 'NONE',  ( 0.000000000000000000, 0.9999999999976377785, 2.173523156925979128E-06 ) ) ;
#59398 = ORIENTED_EDGE ( 'NONE', *, *, #71139, .F. ) ;
#59399 = CARTESIAN_POINT ( 'NONE',  ( 2.178911383790714584, -20.24183328246387958, -1.500000000000002220 ) ) ;
#59400 = VERTEX_POINT ( 'NONE', #82810 ) ;
#59401 = EDGE_CURVE ( 'NONE', #73893, #61226, #80831, .T. ) ;
#59402 = CARTESIAN_POINT ( 'NONE',  ( 12.10309942457327992, -19.51426552955538085, -1.500000000000002220 ) ) ;
#59403 = CARTESIAN_POINT ( 'NONE',  ( -53.52287095715006870, -23.48786465467241058, 11.44779295918255002 ) ) ;
#59404 = EDGE_LOOP ( 'NONE', ( #75767, #95768 ) ) ;
#59405 = CARTESIAN_POINT ( 'NONE',  ( -49.17793306806408538, -25.29053177449054957, 4.390131398629820048 ) ) ;
#59406 = AXIS2_PLACEMENT_3D ( 'NONE', #67000, #96933, #27427 ) ;
#59407 = CARTESIAN_POINT ( 'NONE',  ( -29.49875734969026198, -5.965225279485572685, 10.11402280011862587 ) ) ;
#59408 = CARTESIAN_POINT ( 'NONE',  ( -95.62287095715007013, -23.48786465467241769, 11.44779295918254114 ) ) ;
#59410 = ORIENTED_EDGE ( 'NONE', *, *, #44637, .F. ) ;
#59409 = CARTESIAN_POINT ( 'NONE',  ( 20.41123533131232648, 5.719371238976541427, 11.49999999999999645 ) ) ;
#59411 = EDGE_CURVE ( 'NONE', #33824, #628, #30154, .T. ) ;
#59412 = EDGE_LOOP ( 'NONE', ( #67635, #63147, #3324 ) ) ;
#59413 = CARTESIAN_POINT ( 'NONE',  ( -7.471142097702432316, -20.87072022463130239, 11.49999999999998934 ) ) ;
#59414 = EDGE_CURVE ( 'NONE', #71994, #87941, #86862, .T. ) ;
#59415 = CARTESIAN_POINT ( 'NONE',  ( -10.57813111170615983, 17.65445453266677234, -1.500000000000002220 ) ) ;
#59416 = VECTOR ( 'NONE', #92910, 1000.000000000000114 ) ;
#59417 = ORIENTED_EDGE ( 'NONE', *, *, #72123, .F. ) ;
#59418 = EDGE_LOOP ( 'NONE', ( #39580, #3304, #78492, #78309, #6619 ) ) ;
#59419 = LINE ( 'NONE', #44698, #49535 ) ;
#59420 = CARTESIAN_POINT ( 'NONE',  ( -40.43756433397305017, -25.12049752546737835, 2.832404795212222659 ) ) ;
#59421 = ORIENTED_EDGE ( 'NONE', *, *, #92375, .T. ) ;
#59422 = VECTOR ( 'NONE', #75758, 1000.000000000000114 ) ;
#59423 = VERTEX_POINT ( 'NONE', #89935 ) ;
#59424 = CIRCLE ( 'NONE', #15675, 130.7884398600581335 ) ;
#59425 = ORIENTED_EDGE ( 'NONE', *, *, #23529, .F. ) ;
#59426 = FACE_OUTER_BOUND ( 'NONE', #39814, .T. ) ;
#59428 = CARTESIAN_POINT ( 'NONE',  ( -28.67154396960757268, -23.33526543178592050, 11.44779300624183982 ) ) ;
#59427 = B_SPLINE_CURVE_WITH_KNOTS ( 'NONE', 3,
 ( #85002, #7376, #38330, #54080, #15486, #77379 ),
 .UNSPECIFIED., .F., .F.,
 ( 4, 2, 4 ),
 ( 6.391158118956848875E-06, 0.001387004593080773136, 0.002767618028042589419 ),
 .UNSPECIFIED. ) ;
#59429 = CARTESIAN_POINT ( 'NONE',  ( -33.52287095715006160, -23.47593901973090169, -1.443836447538997314 ) ) ;
#59430 = CARTESIAN_POINT ( 'NONE',  ( 14.61947915221463923, 14.71393552341326760, -1.500000000000002220 ) ) ;
#59431 = ADVANCED_FACE ( 'NONE', ( #3228 ), #34162, .T. ) ;
#59432 = CARTESIAN_POINT ( 'NONE',  ( -9.282276271697774916, -19.63344595494797673, 11.49999999999999645 ) ) ;
#59433 = VERTEX_POINT ( 'NONE', #27041 ) ;
#59434 = CARTESIAN_POINT ( 'NONE',  ( -40.41683116089613748, -25.31583771263539973, 5.082404370641117275 ) ) ;
#59435 = CARTESIAN_POINT ( 'NONE',  ( -37.52287095715006870, -24.66019654487199375, 8.947790411086122830 ) ) ;
#59436 = CARTESIAN_POINT ( 'NONE',  ( -115.5505219823595979, -24.92564183028979130, 1.928384488918252870 ) ) ;
#59437 = CARTESIAN_POINT ( 'NONE',  ( -22.41777205227948855, 0.6913007675000180097, 11.49999999999998934 ) ) ;
#59438 = VECTOR ( 'NONE', #35916, 1000.000000000000114 ) ;
#59439 = CARTESIAN_POINT ( 'NONE',  ( -51.28074245548943111, -25.31296633745817815, 4.131999440082223529 ) ) ;
#59440 = CARTESIAN_POINT ( 'NONE',  ( -124.5228709571500190, -24.66019654487200441, 8.947790411086112172 ) ) ;
#59441 = ORIENTED_EDGE ( 'NONE', *, *, #2502, .F. ) ;
#59442 = CARTESIAN_POINT ( 'NONE',  ( -75.52287095715009002, -24.62226745350438506, 0.9660975649728140713 ) ) ;
#59443 = CARTESIAN_POINT ( 'NONE',  ( 32.76111974776238611, 3.316774720514426900, -3.850861272813261849 ) ) ;
#59444 = EDGE_LOOP ( 'NONE', ( #69270, #16974, #46545, #37511 ) ) ;
#59445 = ORIENTED_EDGE ( 'NONE', *, *, #83495, .F. ) ;
#59446 = CARTESIAN_POINT ( 'NONE',  ( -100.0593466484916831, -25.31258597278857536, 5.273631863065838310 ) ) ;
#59447 = ORIENTED_EDGE ( 'NONE', *, *, #67524, .F. ) ;
#59448 = CARTESIAN_POINT ( 'NONE',  ( -20.90244970016518877, -3.954922567530639199, -1.500000000000002220 ) ) ;
#59449 = ORIENTED_EDGE ( 'NONE', *, *, #84335, .T. ) ;
#59450 = DIRECTION ( 'NONE',  ( -1.000000000000000000, 0.000000000000000000, -0.000000000000000000 ) ) ;
#59451 = CARTESIAN_POINT ( 'NONE',  ( 17.34737195785526609, 13.27887811287985187, 11.49999999999998934 ) ) ;
#59452 = CARTESIAN_POINT ( 'NONE',  ( -55.58953762381671737, -23.47596703998600276, 11.44779298504227505 ) ) ;
#59453 = CARTESIAN_POINT ( 'NONE',  ( 2.290073164716609710, 22.57640404599860418, 11.49999999999998934 ) ) ;
#59454 = CARTESIAN_POINT ( 'NONE',  ( -40.84535658588885099, -25.28892436072735705, 3.358264504957044760 ) ) ;
#59455 = CARTESIAN_POINT ( 'NONE',  ( -28.92287095928432095, -23.34274621196139421, 11.44779298504227860 ) ) ;
#59456 = CARTESIAN_POINT ( 'NONE',  ( -21.55542221127511482, -4.010009934288176758, -1.500000000000002220 ) ) ;
#59457 = CARTESIAN_POINT ( 'NONE',  ( -87.51421903235882382, -23.96119346886881729, -0.6495511937831870419 ) ) ;
#59458 = EDGE_LOOP ( 'NONE', ( #51533, #38292, #52451, #98723 ) ) ;
#59459 = CARTESIAN_POINT ( 'NONE',  ( -37.62287095715007013, -23.47596703998600276, 11.44779298504227505 ) ) ;
#59460 = EDGE_CURVE ( 'NONE', #23749, #94938, #58010, .T. ) ;
#59461 = VECTOR ( 'NONE', #69283, 1000.000000000000114 ) ;
#59462 = ORIENTED_EDGE ( 'NONE', *, *, #71191, .T. ) ;
#59463 = CARTESIAN_POINT ( 'NONE',  ( -116.6228709571500701, -23.72747288104470087, -1.053458166803224350 ) ) ;
#59464 = B_SPLINE_CURVE_WITH_KNOTS ( 'NONE', 3,
 ( #53226, #84658, #69934, #84154 ),
 .UNSPECIFIED., .F., .F.,
 ( 4, 4 ),
 ( 0.000000000000000000, 1.000000000000000000 ),
 .UNSPECIFIED. ) ;
#59465 = CARTESIAN_POINT ( 'NONE',  ( -128.5228709571500474, -23.48783264083417066, -1.443836473375472274 ) ) ;
#59466 = CIRCLE ( 'NONE', #51354, 0.3000000000000016542 ) ;
#59467 = CARTESIAN_POINT ( 'NONE',  ( -0.1256113942619183077, -21.42386179076044073, -0.9709657327914291702 ) ) ;
#59468 = CARTESIAN_POINT ( 'NONE',  ( -8.014198274750887308, -19.69740135394370384, -1.500000000000002220 ) ) ;
#59469 = CARTESIAN_POINT ( 'NONE',  ( -112.5150172138885694, -24.51314013834317151, 0.6176544820404297198 ) ) ;
#59470 = CARTESIAN_POINT ( 'NONE',  ( -32.30247028140506416, -1.684774720514426560, 27.60502002861223048 ) ) ;
#59471 = CARTESIAN_POINT ( 'NONE',  ( -114.5228709571500332, -24.34917612407039655, 0.1852690917479089538 ) ) ;
#59472 = CARTESIAN_POINT ( 'NONE',  ( -70.52287095715009002, -24.51163499207179797, 0.6490370598555543769 ) ) ;
#59473 = EDGE_CURVE ( 'NONE', #50385, #22003, #50387, .T. ) ;
#59474 = B_SPLINE_SURFACE_WITH_KNOTS ( 'NONE', 3, 1, ( 
 ( #43483, #42497 ),
 ( #3929, #88657 ),
 ( #90640, #12019 ),
 ( #67317, #80533 ),
 ( #4422, #73432 ),
 ( #35372, #59709 ),
 ( #96758, #11027 ),
 ( #66833, #27257 ),
 ( #58211, #34367 ),
 ( #20624, #13006 ),
 ( #41997, #65347 ),
 ( #72934, #97754 ),
 ( #12516, #51591 ),
 ( #81545, #43972 ),
 ( #96265, #66335 ),
 ( #82036, #28747 ),
 ( #82526, #89648 ),
 ( #98242, #20130 ),
 ( #74904, #3434 ) ),
 .UNSPECIFIED., .F., .F., .F.,
 ( 4, 1, 1, 1, 1, 1, 1, 1, 1, 1, 1, 1, 1, 1, 1, 1, 4 ),
 ( 2, 2 ),
 ( 0.000000000000000000, 0.07059928943359371212, 0.1379009210036218069, 0.2031961978097392985, 0.2667897246502602959, 0.3291063872214292640, 0.3906535452348646187, 0.4526530569344794919, 0.5157480403003763536, 0.5779263408004525759, 0.6389300116184458700, 0.6983507176418246587, 0.7572960374442720966, 0.8163937673501532322, 0.8762669096141292302, 0.9368171089060849388, 1.000000000000000000 ),
 ( 0.000000000000000000, 1.000000000000000000 ),
 .UNSPECIFIED. ) ;
#59475 = CARTESIAN_POINT ( 'NONE',  ( -117.5198278380623123, -23.96169478059714564, 10.65365249895717170 ) ) ;
#59476 = ORIENTED_EDGE ( 'NONE', *, *, #22151, .T. ) ;
#59477 = CARTESIAN_POINT ( 'NONE',  ( -16.94305004876727239, 9.801747318927828800, 11.49999999999999645 ) ) ;
#59478 = DIRECTION ( 'NONE',  ( 0.000000000000000000, -2.173523156925979552E-06, 0.9999999999976378895 ) ) ;
#59479 = CARTESIAN_POINT ( 'NONE',  ( -100.6228709571500985, -24.14406661707771207, 10.28769366152061160 ) ) ;
#59480 = VERTEX_POINT ( 'NONE', #73712 ) ;
#59481 = CARTESIAN_POINT ( 'NONE',  ( -117.5228709571500616, -24.50321055353804311, 9.387540953477508054 ) ) ;
#59482 = CARTESIAN_POINT ( 'NONE',  ( -40.58953762381672448, -23.47596703998600276, 11.44779298504227505 ) ) ;
#59483 = AXIS2_PLACEMENT_3D ( 'NONE', #92150, #93646, #23126 ) ;
#59484 = CARTESIAN_POINT ( 'NONE',  ( -116.5228709571499905, -23.48783264083416711, -1.443836473375476270 ) ) ;
#59485 = CARTESIAN_POINT ( 'NONE',  ( -50.40445135320379677, -25.12298712672050982, 7.101635559041870494 ) ) ;
#59486 = CARTESIAN_POINT ( 'NONE',  ( -19.67082186522023690, -1.387426831159568108, 11.49999999999998934 ) ) ;
#59487 = ORIENTED_EDGE ( 'NONE', *, *, #86747, .F. ) ;
#59488 = PLANE ( 'NONE',  #8407 ) ;
#59489 = CARTESIAN_POINT ( 'NONE',  ( -112.5228709571500616, -24.64898659630529210, 1.056161002820831474 ) ) ;
#59490 = VECTOR ( 'NONE', #95221, 1000.000000000000114 ) ;
#59491 = EDGE_CURVE ( 'NONE', #54673, #53154, #97477, .T. ) ;
#59492 = COORDINATED_UNIVERSAL_TIME_OFFSET ( 0, 0, .AHEAD. ) ;
#59493 = ORIENTED_EDGE ( 'NONE', *, *, #37125, .F. ) ;
#59494 = DIRECTION ( 'NONE',  ( -0.000000000000000000, -0.000000000000000000, -1.000000000000000000 ) ) ;
#59495 = CARTESIAN_POINT ( 'NONE',  ( -45.62287095715004170, -23.85229601348996198, 10.88205029486207742 ) ) ;
#59496 = CARTESIAN_POINT ( 'NONE',  ( -47.58717649367020641, -24.34968618360933590, 0.1864209137778879144 ) ) ;
#59497 = CARTESIAN_POINT ( 'NONE',  ( -50.55620429048339304, -24.99156044556202261, 7.747789690856172307 ) ) ;
#59498 = FACE_OUTER_BOUND ( 'NONE', #86616, .T. ) ;
#59499 = CIRCLE ( 'NONE', #64158, 1.149999999999999911 ) ;
#59500 = EDGE_CURVE ( 'NONE', #1528, #5079, #59286, .T. ) ;
#59501 = VECTOR ( 'NONE', #36253, 1000.000000000000000 ) ;
#59502 = CARTESIAN_POINT ( 'NONE',  ( -6.741682653110981249, 5.965225279485572685, 30.62569541381301619 ) ) ;
#59503 = CARTESIAN_POINT ( 'NONE',  ( -112.5228709571500332, -23.94994826722564696, -0.6494450866342713624 ) ) ;
#59504 = CARTESIAN_POINT ( 'NONE',  ( -18.20579941527595480, -8.200869797747142087, -1.500000000000002220 ) ) ;
#59505 = B_SPLINE_CURVE_WITH_KNOTS ( 'NONE', 3,
 ( #18907, #18416, #26537, #80315 ),
 .UNSPECIFIED., .F., .F.,
 ( 4, 4 ),
 ( 0.000000000000000000, 9.999999999998897304E-05 ),
 .UNSPECIFIED. ) ;
#59506 = DIRECTION ( 'NONE',  ( 0.000000000000000000, -1.000000000000000000, 0.000000000000000000 ) ) ;
#59507 = CARTESIAN_POINT ( 'NONE',  ( -0.1426030150137701236, -21.20389190742571373, -1.497999999999532594 ) ) ;
#59508 = EDGE_LOOP ( 'NONE', ( #58917, #79155, #99768, #91498 ) ) ;
#59509 = ADVANCED_FACE ( 'NONE', ( #52375 ), #52877, .T. ) ;
#59510 = CARTESIAN_POINT ( 'NONE',  ( -2.768609665556983845, 5.965225279485594001, -29.41086200512614823 ) ) ;
#59511 = CARTESIAN_POINT ( 'NONE',  ( 4.653846153846159517, -5.876774720514415407, 19.99999999999999289 ) ) ;
#59512 = EDGE_CURVE ( 'NONE', #21092, #40713, #53381, .T. ) ;
#59514 = EDGE_CURVE ( 'NONE', #24841, #4424, #25310, .T. ) ;
#59513 = CARTESIAN_POINT ( 'NONE',  ( -119.5532611137347914, -24.51314013834316086, 0.6176544820404233915 ) ) ;
#59515 = DIRECTION ( 'NONE',  ( 0.000000000000000000, -0.9999999999976377785, -2.173523156925979975E-06 ) ) ;
#59516 = CARTESIAN_POINT ( 'NONE',  ( -126.3652925398622529, -25.21789590547953352, 6.462002543204359739 ) ) ;
#59517 = CARTESIAN_POINT ( 'NONE',  ( -39.62372002940962545, -24.65952944569304250, 1.056160979905697017 ) ) ;
#59518 = CARTESIAN_POINT ( 'NONE',  ( -72.62287095715009855, -23.95044443724992433, 10.65354141964649948 ) ) ;
#59519 = CARTESIAN_POINT ( 'NONE',  ( -51.53844848903055009, -25.31574372701962616, 4.526031553223371695 ) ) ;
#59520 = ORIENTED_EDGE ( 'NONE', *, *, #4977, .T. ) ;
#59521 = CARTESIAN_POINT ( 'NONE',  ( -2.285970405126252825, -5.876774720514409189, 19.14905311829361167 ) ) ;
#59522 = CARTESIAN_POINT ( 'NONE',  ( -127.5552457623996787, -24.51314013834318217, 0.6176544820404269442 ) ) ;
#59523 = EDGE_LOOP ( 'NONE', ( #80536, #69899, #81667, #94321 ) ) ;
#59524 = CARTESIAN_POINT ( 'NONE',  ( 20.24638344296597836, 0.1212440198127159030, 11.49999999999998934 ) ) ;
#59525 = ADVANCED_FACE ( 'NONE', ( #60991 ), #37142, .F. ) ;
#59526 = CARTESIAN_POINT ( 'NONE',  ( 6.467769777575680834, -5.876774720514427841, 21.83821538399986650 ) ) ;
#59527 = DIRECTION ( 'NONE',  ( -3.773278334453079030E-23, 0.9999999999976377785, 2.173523156925979128E-06 ) ) ;
#59528 = AXIS2_PLACEMENT_3D ( 'NONE', #53329, #90379, #14239 ) ;
#59529 = DIRECTION ( 'NONE',  ( 0.000000000000000000, -0.9999999999976377785, -2.173523156925979975E-06 ) ) ;
#59530 = ORIENTED_EDGE ( 'NONE', *, *, #57149, .F. ) ;
#59531 = CARTESIAN_POINT ( 'NONE',  ( -80.26322933785027658, -25.30551634214781132, 4.507558500180725680 ) ) ;
#59532 = LINE ( 'NONE', #81365, #14636 ) ;
#59533 = CARTESIAN_POINT ( 'NONE',  ( 14.85562765054232059, -13.46834898924134372, -1.500000000000002220 ) ) ;
#59534 = CARTESIAN_POINT ( 'NONE',  ( -5.295558097854481616, 20.35707381486366785, 11.49999999999999645 ) ) ;
#59535 = AXIS2_PLACEMENT_3D ( 'NONE', #6432, #12160, #89299 ) ;
#59536 = CARTESIAN_POINT ( 'NONE',  ( -27.68651082257923690, -24.80976250947271211, 7.605672514646787619 ) ) ;
#59537 = CARTESIAN_POINT ( 'NONE',  ( -70.50070265878940745, -24.40133493613049964, 9.663955038902802386 ) ) ;
#59538 = CARTESIAN_POINT ( 'NONE',  ( -16.08457400211760913, 15.13120210334024662, 11.49999999999998934 ) ) ;
#59539 = ADVANCED_FACE ( 'NONE', ( #21398 ), #29522, .F. ) ;
#59540 = CARTESIAN_POINT ( 'NONE',  ( -19.23287947355762384, -7.152392467615741545, 11.49999999999998934 ) ) ;
#59541 = PLANE ( 'NONE',  #86797 ) ;
#59542 = CARTESIAN_POINT ( 'NONE',  ( -55.52287095715005449, -24.99132157543083821, 2.256160258750667502 ) ) ;
#59543 = CARTESIAN_POINT ( 'NONE',  ( -78.62287095715005592, -29.50250786944525672, 11.44777988621623521 ) ) ;
#59544 = ORIENTED_EDGE ( 'NONE', *, *, #89286, .F. ) ;
#59545 = EDGE_CURVE ( 'NONE', #11247, #24018, #76190, .T. ) ;
#59546 = DIRECTION ( 'NONE',  ( -0.000000000000000000, -1.000000000000000000, -0.000000000000000000 ) ) ;
#59547 = FACE_OUTER_BOUND ( 'NONE', #20404, .T. ) ;
#59548 = B_SPLINE_CURVE_WITH_KNOTS ( 'NONE', 3,
 ( #31289, #62256, #16056, #24174, #55148, #16554 ),
 .UNSPECIFIED., .F., .F.,
 ( 4, 2, 4 ),
 ( 0.000000000000000000, 0.001380901958385383124, 0.002761803916770766247 ),
 .UNSPECIFIED. ) ;
#59549 = VERTEX_POINT ( 'NONE', #68104 ) ;
#59550 = VERTEX_POINT ( 'NONE', #29025 ) ;
#59551 = CARTESIAN_POINT ( 'NONE',  ( -55.52287095715007581, -24.83602698348158810, 1.605859176311263070 ) ) ;
#59552 = DIRECTION ( 'NONE',  ( -1.000000000000000000, 0.000000000000000000, 0.000000000000000000 ) ) ;
#59553 = CARTESIAN_POINT ( 'NONE',  ( -76.63826584465937231, -23.96119346886880663, -0.6495511937832059157 ) ) ;
#59554 = CARTESIAN_POINT ( 'NONE',  ( -4.563637348303267949, -20.04915943051449645, -1.500000000000002220 ) ) ;
#59555 = ADVANCED_FACE ( 'NONE', ( #76679 ), #5692, .F. ) ;
#59556 = CARTESIAN_POINT ( 'NONE',  ( -10.34410514300256523, -18.92461576200269491, 11.49999999999999645 ) ) ;
#59557 = ORIENTED_EDGE ( 'NONE', *, *, #42798, .F. ) ;
#59558 = CARTESIAN_POINT ( 'NONE',  ( -49.92862301476790066, -25.14597343102002824, 7.027096283259375298 ) ) ;
#59559 = CARTESIAN_POINT ( 'NONE',  ( -99.57239932359995294, -25.30502750817439761, 4.874438929701363499 ) ) ;
#59560 = CARTESIAN_POINT ( 'NONE',  ( -35.52287095715005449, -23.48783264083451883, -1.443836473374936258 ) ) ;
#59561 = CARTESIAN_POINT ( 'NONE',  ( 19.44376294880228428, 11.01865886811674677, 11.49999999999998934 ) ) ;
#59562 = CIRCLE ( 'NONE', #74117, 1.249999999999999112 ) ;
#59563 = ADVANCED_FACE ( 'NONE', ( #6689 ), #92420, .F. ) ;
#59564 = PLANE ( 'NONE',  #17300 ) ;
#59565 = CARTESIAN_POINT ( 'NONE',  ( -61.58953762381672448, -24.64898659630528854, 1.056161002820822148 ) ) ;
#59566 = VERTEX_POINT ( 'NONE', #53876 ) ;
#59567 = EDGE_CURVE ( 'NONE', #13108, #90802, #88860, .T. ) ;
#59568 = CARTESIAN_POINT ( 'NONE',  ( -94.52287095715001897, -24.34917612406837151, 0.1852690917426572381 ) ) ;
#59569 = CARTESIAN_POINT ( 'NONE',  ( 3.448102555317568374, -5.876774720514424288, 21.39871091031772110 ) ) ;
#59570 = CARTESIAN_POINT ( 'NONE',  ( -2.496121100066326814, 20.73550571027955769, 11.49999999999998934 ) ) ;
#59571 = ORIENTED_EDGE ( 'NONE', *, *, #37561, .T. ) ;
#59572 = B_SPLINE_CURVE_WITH_KNOTS ( 'NONE', 3,
 ( #96268, #65842, #26753, #94757, #87658, #34370 ),
 .UNSPECIFIED., .F., .F.,
 ( 4, 2, 4 ),
 ( 1.570887131794638196E-05, 0.001396322306279761940, 0.002776935741241577573 ),
 .UNSPECIFIED. ) ;
#59574 = EDGE_LOOP ( 'NONE', ( #25794, #1469, #26650, #51953, #36899 ) ) ;
#59573 = CARTESIAN_POINT ( 'NONE',  ( -67.62364353413191509, -24.66019654487199730, 8.947790411086115725 ) ) ;
#59575 = CIRCLE ( 'NONE', #54724, 1.325999999999969647 ) ;
#59576 = ORIENTED_EDGE ( 'NONE', *, *, #65273, .F. ) ;
#59577 = CARTESIAN_POINT ( 'NONE',  ( -50.38822539166533687, -25.30267106383720943, 4.736250553104468075 ) ) ;
#59578 = CARTESIAN_POINT ( 'NONE',  ( 5.126256225908648823, -20.47799061884807870, -1.500000000000002220 ) ) ;
#59579 = ORIENTED_EDGE ( 'NONE', *, *, #89298, .F. ) ;
#59580 = CARTESIAN_POINT ( 'NONE',  ( -34.52287095715006160, -24.64965694238575011, 8.947790433994207149 ) ) ;
#59581 = CARTESIAN_POINT ( 'NONE',  ( -63.62287095715004881, -23.48786465467241058, 11.44779295918254824 ) ) ;
#59582 = CARTESIAN_POINT ( 'NONE',  ( -25.92875734969026169, -3.316774720514426456, 26.43402280011862615 ) ) ;
#59583 = VECTOR ( 'NONE', #54246, 1000.000000000000000 ) ;
#59584 = CARTESIAN_POINT ( 'NONE',  ( -76.59623078494088588, -23.96169478059713143, 10.65365249895718058 ) ) ;
#59585 = FACE_OUTER_BOUND ( 'NONE', #54189, .T. ) ;
#59586 = CARTESIAN_POINT ( 'NONE',  ( -19.25911440464646063, 10.06369110047026538, -1.500000000000002220 ) ) ;
#59587 = LINE ( 'NONE', #98117, #12256 ) ;
#59589 = ORIENTED_EDGE ( 'NONE', *, *, #78158, .F. ) ;
#59588 = CARTESIAN_POINT ( 'NONE',  ( 18.42719714020066846, 12.55551944762973626, 11.49999999999999645 ) ) ;
#59590 = CARTESIAN_POINT ( 'NONE',  ( -33.52287095715006160, -24.51283580621449687, 0.6167428607045510880 ) ) ;
#59591 = CARTESIAN_POINT ( 'NONE',  ( 7.010993867624484288, -6.376774720514417183, 20.34381700913260715 ) ) ;
#59592 = CARTESIAN_POINT ( 'NONE',  ( -106.5228709571500758, -23.47596703998600631, 11.44779298504228038 ) ) ;
#59593 = VERTEX_POINT ( 'NONE', #21895 ) ;
#59594 = ORIENTED_EDGE ( 'NONE', *, *, #7401, .F. ) ;
#59595 = EDGE_LOOP ( 'NONE', ( #86218, #4394, #197, #96997 ) ) ;
#59596 = CARTESIAN_POINT ( 'NONE',  ( -75.52287095715011844, -23.48783264082477373, -1.443836473390087694 ) ) ;
#59597 = DIRECTION ( 'NONE',  ( 0.000000000000000000, -1.000000000000000000, 0.000000000000000000 ) ) ;
#59598 = CARTESIAN_POINT ( 'NONE',  ( -78.94388818075310610, -25.03137962884571266, 6.014208626624816922 ) ) ;
#59599 = CARTESIAN_POINT ( 'NONE',  ( -67.52287095715006160, -23.48786465467241769, 11.44779295918254647 ) ) ;
#59600 = CARTESIAN_POINT ( 'NONE',  ( -2.960655606634402748, -19.13016773636607581, -1.500000000000002220 ) ) ;
#59601 = CARTESIAN_POINT ( 'NONE',  ( 16.30000000000000071, 0.000000000000000000, 0.000000000000000000 ) ) ;
#59602 = ORIENTED_EDGE ( 'NONE', *, *, #82074, .T. ) ;
#59604 = CARTESIAN_POINT ( 'NONE',  ( -18.68205546197936684, -5.105407162728520021, 11.49999999999999645 ) ) ;
#59603 = APPLICATION_CONTEXT ( 'configuration controlled 3d designs of mechanical parts and assemblies' ) ;
#59605 = CARTESIAN_POINT ( 'NONE',  ( 10.57556460110582996, 0.7139560615726621151, -8.999999999999991118 ) ) ;
#59606 = EDGE_LOOP ( 'NONE', ( #96975, #51562, #22348, #33200 ) ) ;
#59607 = CARTESIAN_POINT ( 'NONE',  ( 2.968164339864655332, -6.376774720514408301, 19.33154224050496595 ) ) ;
#59608 = CARTESIAN_POINT ( 'NONE',  ( 7.491841679052118508, 5.356774720514426491, -25.13395656343690021 ) ) ;
#59609 = VECTOR ( 'NONE', #90895, 1000.000000000000114 ) ;
#59610 = CARTESIAN_POINT ( 'NONE',  ( -13.89275734969026388, -5.965225279485572685, 31.02402280011862246 ) ) ;
#59611 = FACE_OUTER_BOUND ( 'NONE', #20490, .T. ) ;
#59612 = B_SPLINE_CURVE_WITH_KNOTS ( 'NONE', 3,
 ( #36872, #14016, #29756, #36372 ),
 .UNSPECIFIED., .F., .F.,
 ( 4, 4 ),
 ( 0.000000000000000000, 0.9302372224392947420 ),
 .UNSPECIFIED. ) ;
#59613 = CARTESIAN_POINT ( 'NONE',  ( 15.22544387773384500, -12.34335808662847178, 11.49999999999998934 ) ) ;
#59614 = B_SPLINE_SURFACE_WITH_KNOTS ( 'NONE', 3, 3, ( 
 ( #88796, #83657, #59843, #100359 ),
 ( #68940, #76531, #45611, #6544 ),
 ( #44608, #36486, #37491, #67451 ),
 ( #52225, #99379, #14139, #98376 ),
 ( #28880, #90781, #21251, #30372 ),
 ( #61344, #75040, #13140, #91276 ),
 ( #7038, #51724, #37990, #5535 ) ),
 .UNSPECIFIED., .F., .F., .F.,
 ( 4, 3, 4 ),
 ( 4, 4 ),
 ( 0.0004766839783815509496, 0.1029713700210891786, 0.2054660560637968092 ),
 ( 0.6596618039411151768, 0.6609788952414030749 ),
 .UNSPECIFIED. ) ;
#59615 = CYLINDRICAL_SURFACE ( 'NONE', #63990, 1.000000000000000000 ) ;
#59616 = EDGE_LOOP ( 'NONE', ( #51853, #43479, #4137, #87778, #63296, #57824, #90647, #79776, #73303, #92589, #4811, #99344 ) ) ;
#59617 = CARTESIAN_POINT ( 'NONE',  ( -0.8629811567608781653, -21.54619324973139172, 11.49999999999998934 ) ) ;
#59618 = CARTESIAN_POINT ( 'NONE',  ( -32.62287095715004881, -29.50248528299804818, 1.056150453629029817 ) ) ;
#59619 = DIRECTION ( 'NONE',  ( -3.773278334453079618E-23, 0.9999999999976377785, 2.173523156925979975E-06 ) ) ;
#59620 = CARTESIAN_POINT ( 'NONE',  ( -81.58953762381669605, -24.64965694238407323, 8.947790433994653014 ) ) ;
#59621 = CARTESIAN_POINT ( 'NONE',  ( -99.92039718326317654, -25.18439361145108180, 3.410800908530512654 ) ) ;
#59622 = CARTESIAN_POINT ( 'NONE',  ( -12.06219892284564388, 19.56905390912838172, -1.500000000000002220 ) ) ;
#59623 = EDGE_CURVE ( 'NONE', #57615, #17980, #58333, .T. ) ;
#59624 = APPROVAL_STATUS ( 'not_yet_approved' ) ;
#59625 = CARTESIAN_POINT ( 'NONE',  ( -118.5228709571500758, -24.64965694238408034, 8.947790433994191162 ) ) ;
#59626 = FACE_OUTER_BOUND ( 'NONE', #59796, .T. ) ;
#59627 = CARTESIAN_POINT ( 'NONE',  ( 13.66866334921533799, -14.80927461459226890, 11.49999999999999645 ) ) ;
#59628 = CARTESIAN_POINT ( 'NONE',  ( -70.62287095715005592, -23.47593901973091235, -1.443836447539006196 ) ) ;
#59629 = PLANE ( 'NONE',  #61408 ) ;
#59630 = PRODUCT_DEFINITION_SHAPE ( 'NONE', 'NONE',  #100424 ) ;
#59631 = CARTESIAN_POINT ( 'NONE',  ( -4.141025641025641413, -5.876774720514419847, 20.67377804487180271 ) ) ;
#59632 = CARTESIAN_POINT ( 'NONE',  ( -76.62287095715007013, -29.50248528299804818, 1.056150453629038477 ) ) ;
#59633 = CARTESIAN_POINT ( 'NONE',  ( -75.52287095715006160, -24.99132157543084176, 2.256160258750667502 ) ) ;
#59634 = CARTESIAN_POINT ( 'NONE',  ( -17.31707178780640533, -9.736581320607820444, 11.49999999999998934 ) ) ;
#59636 = EDGE_CURVE ( 'NONE', #95120, #63086, #82152, .T. ) ;
#59635 = CARTESIAN_POINT ( 'NONE',  ( -113.6295937444302524, -23.73766607897670156, -1.055555164236448240 ) ) ;
#59637 = CARTESIAN_POINT ( 'NONE',  ( 12.99534586470982234, -14.87506298573330632, -1.500000000000002220 ) ) ;
#59638 = EDGE_CURVE ( 'NONE', #44200, #32974, #23393, .T. ) ;
#59639 = AXIS2_PLACEMENT_3D ( 'NONE', #5321, #28169, #36284 ) ;
#59640 = CARTESIAN_POINT ( 'NONE',  ( -126.5215128601554255, -23.96169478059714208, 10.65365249895716637 ) ) ;
#59641 = EDGE_CURVE ( 'NONE', #89889, #82876, #20242, .T. ) ;
#59642 = EDGE_CURVE ( 'NONE', #99983, #96134, #97381, .T. ) ;
#59643 = CARTESIAN_POINT ( 'NONE',  ( -125.6228709571500843, -24.91570333823101180, 8.075032458375559941 ) ) ;
#59644 = CARTESIAN_POINT ( 'NONE',  ( -94.62287095715005592, -29.50250243563736774, 8.947779886222139822 ) ) ;
#59645 = CARTESIAN_POINT ( 'NONE',  ( 19.89799572200132971, -5.707369160466581270, 11.49999999999999645 ) ) ;
#59646 = FACE_OUTER_BOUND ( 'NONE', #75619, .T. ) ;
#59647 = AXIS2_PLACEMENT_3D ( 'NONE', #37701, #6252, #35720 ) ;
#59648 = CARTESIAN_POINT ( 'NONE',  ( 30.61866831821571111, 5.272393720821680674, 0.8164977272573440414 ) ) ;
#59649 = DIRECTION ( 'NONE',  ( 0.000000000000000000, -2.173523156925979552E-06, 0.9999999999976378895 ) ) ;
#59650 = CARTESIAN_POINT ( 'NONE',  ( 22.61316900856233403, 2.020702135111208442, 11.49999999999999645 ) ) ;
#59651 = ORIENTED_EDGE ( 'NONE', *, *, #70339, .F. ) ;
#59652 = CARTESIAN_POINT ( 'NONE',  ( 0.5999240985075944277, 1.411520799013914917, -8.999999999999998224 ) ) ;
#59653 = CARTESIAN_POINT ( 'NONE',  ( 29.71903944837828604, 4.668615314384465087, 27.69752233256919993 ) ) ;
#59654 = CIRCLE ( 'NONE', #23987, 1.000000000000000000 ) ;
#59655 = EDGE_CURVE ( 'NONE', #11783, #66705, #16238, .T. ) ;
#59656 = CARTESIAN_POINT ( 'NONE',  ( -63.57960882203882136, -24.65952944569304250, 1.056160979905695463 ) ) ;
#59657 = DIRECTION ( 'NONE',  ( 0.000000000000000000, 0.000000000000000000, -1.000000000000000000 ) ) ;
#59658 = ORIENTED_EDGE ( 'NONE', *, *, #47764, .T. ) ;
#59659 = VERTEX_POINT ( 'NONE', #83137 ) ;
#59660 = ADVANCED_FACE ( 'NONE', ( #6022 ), #43598, .T. ) ;
#59661 = CARTESIAN_POINT ( 'NONE',  ( -99.30666603356964117, -25.23741546797077362, 6.288603370249809643 ) ) ;
#59662 = CARTESIAN_POINT ( 'NONE',  ( 4.181975289622855918, -22.47981636197143374, 11.49999999999998934 ) ) ;
#59663 = CARTESIAN_POINT ( 'NONE',  ( -29.55259386707723124, -23.87806136140024194, -0.6495508823503305385 ) ) ;
#59664 = CARTESIAN_POINT ( 'NONE',  ( 14.45009471711328786, 16.04676183837579373, -1.500000000000002220 ) ) ;
#59665 = VECTOR ( 'NONE', #43898, 1000.000000000000000 ) ;
#59666 = DIRECTION ( 'NONE',  ( -0.000000000000000000, 1.000000000000000000, -0.000000000000000000 ) ) ;
#59667 = CARTESIAN_POINT ( 'NONE',  ( 0.000000000000000000, -2.682774720514426559, 0.000000000000000000 ) ) ;
#59668 = CARTESIAN_POINT ( 'NONE',  ( 9.831018646898828095, -20.30805102056165623, 11.49999999999999645 ) ) ;
#59669 = ORIENTED_EDGE ( 'NONE', *, *, #19452, .F. ) ;
#59670 = CARTESIAN_POINT ( 'NONE',  ( -70.13845683480205651, -25.31612421240863142, 4.855284239541365565 ) ) ;
#59671 = CARTESIAN_POINT ( 'NONE',  ( 8.537626919312410578, 20.26776412955123163, 11.49999999999998934 ) ) ;
#59672 = ADVANCED_FACE ( 'NONE', ( #34983 ), #36100, .T. ) ;
#59673 = CARTESIAN_POINT ( 'NONE',  ( -105.6271209236252275, -24.63419186844610920, 9.035850630976920428 ) ) ;
#59674 = CARTESIAN_POINT ( 'NONE',  ( -41.58766378979927936, -25.29087150074615309, 3.364589589010316573 ) ) ;
#59675 = ORIENTED_EDGE ( 'NONE', *, *, #84833, .F. ) ;
#59676 = CARTESIAN_POINT ( 'NONE',  ( -89.62287095715004170, -23.48786465467241413, 11.44779295918254114 ) ) ;
#59677 = CARTESIAN_POINT ( 'NONE',  ( -90.50788615195934028, -24.40133493613049964, 9.663955038902805939 ) ) ;
#59678 = ORIENTED_EDGE ( 'NONE', *, *, #28249, .T. ) ;
#59679 = CARTESIAN_POINT ( 'NONE',  ( -49.62287095715005592, -23.48786465467241058, 11.44779295918254824 ) ) ;
#59680 = ORIENTED_EDGE ( 'NONE', *, *, #36840, .T. ) ;
#59681 = ORIENTED_EDGE ( 'NONE', *, *, #35893, .F. ) ;
#59682 = FACE_OUTER_BOUND ( 'NONE', #31788, .T. ) ;
#59683 = CARTESIAN_POINT ( 'NONE',  ( -104.5228709571501327, -24.34917612406838572, 0.1852690917426617068 ) ) ;
#59684 = CARTESIAN_POINT ( 'NONE',  ( -36.51286536810861350, -23.73766607897670156, -1.055555164236459120 ) ) ;
#59685 = CARTESIAN_POINT ( 'NONE',  ( 7.241121213506172438, 19.11196469071355963, -1.500000000000002220 ) ) ;
#59686 = EDGE_CURVE ( 'NONE', #2769, #11988, #32733, .T. ) ;
#59687 = VERTEX_POINT ( 'NONE', #54220 ) ;
#59688 = CARTESIAN_POINT ( 'NONE',  ( -3.054691362729579751, -6.376774720514413630, 19.78730719034165375 ) ) ;
#59689 = CARTESIAN_POINT ( 'NONE',  ( -30.56688274934923655, -25.56688301298833821, 3.825958421598584014 ) ) ;
#59690 = ADVANCED_FACE ( 'NONE', ( #92750 ), #38479, .F. ) ;
#59691 = DIRECTION ( 'NONE',  ( -1.000000000000000000, -3.773278334444166432E-23, -8.201307841325785021E-29 ) ) ;
#59692 = CARTESIAN_POINT ( 'NONE',  ( -8.159999999999998366, 9.922373532429842768, -0.8680951993573241543 ) ) ;
#59693 = VERTEX_POINT ( 'NONE', #86520 ) ;
#59694 = PLANE ( 'NONE',  #14408 ) ;
#59695 = DIRECTION ( 'NONE',  ( -1.000000000000000000, -3.491481338843133355E-15, -2.352173255807796056E-16 ) ) ;
#59696 = CARTESIAN_POINT ( 'NONE',  ( -6.767879454864726974, -19.68250801024624508, 11.49999999999998934 ) ) ;
#59697 = EDGE_CURVE ( 'NONE', #46565, #98443, #98240, .T. ) ;
#59698 = ORIENTED_EDGE ( 'NONE', *, *, #6101, .F. ) ;
#59700 = EDGE_LOOP ( 'NONE', ( #57976, #64714, #58827, #76621, #75961, #33321 ) ) ;
#59699 = CARTESIAN_POINT ( 'NONE',  ( 25.83488407601165093, -3.407774720514426647, -11.31196583263649558 ) ) ;
#59701 = B_SPLINE_SURFACE_WITH_KNOTS ( 'NONE', 3, 3, ( 
 ( #86639, #55712, #46587, #31352 ),
 ( #9515, #55211, #39965, #67547 ),
 ( #906, #401, #39469, #38961 ),
 ( #54704, #62316, #85133, #75628 ),
 ( #29459, #98465, #31860, #69916 ),
 ( #94247, #9015, #70929, #44703 ),
 ( #85636, #1416, #32351, #78510 ) ),
 .UNSPECIFIED., .F., .F., .F.,
 ( 4, 3, 4 ),
 ( 4, 4 ),
 ( 0.7945040050992231428, 0.8970133687736494554, 0.9995227324480756570 ),
 ( 0.1895421625358439111, 0.1906423923308985524 ),
 .UNSPECIFIED. ) ;
#59702 = DIRECTION ( 'NONE',  ( 0.000000000000000000, 1.000000000000000000, 0.000000000000000000 ) ) ;
#59703 = CARTESIAN_POINT ( 'NONE',  ( -33.52287095715006160, -23.47593901973090169, -1.443836447538997314 ) ) ;
#59704 = VERTEX_POINT ( 'NONE', #45598 ) ;
#59705 = ORIENTED_EDGE ( 'NONE', *, *, #81643, .F. ) ;
#59706 = CARTESIAN_POINT ( 'NONE',  ( 31.74473449900405697, -4.976825198871215328, -4.259190951192157293 ) ) ;
#59707 = DIRECTION ( 'NONE',  ( -0.000000000000000000, -0.000000000000000000, 1.000000000000000000 ) ) ;
#59708 = CARTESIAN_POINT ( 'NONE',  ( -60.62287095715005592, -23.48786465467241058, 11.44779295918254824 ) ) ;
#59709 = CARTESIAN_POINT ( 'NONE',  ( -70.74035176281489612, -25.24515055801344587, 5.376056033097980524 ) ) ;
#59711 = ORIENTED_EDGE ( 'NONE', *, *, #77312, .T. ) ;
#59710 = CARTESIAN_POINT ( 'NONE',  ( 19.07224962250127831, -11.27678277851665634, 11.49999999999999645 ) ) ;
#59712 = B_SPLINE_CURVE_WITH_KNOTS ( 'NONE', 3,
 ( #55319, #1018, #70025, #61925, #31464, #39578 ),
 .UNSPECIFIED., .F., .F.,
 ( 4, 2, 4 ),
 ( 0.000000000000000000, 0.001380901958385389195, 0.002761803916770778390 ),
 .UNSPECIFIED. ) ;
#59713 = CARTESIAN_POINT ( 'NONE',  ( -108.5942885673410672, -23.73766607897671932, -1.055555164236429366 ) ) ;
#59714 = CARTESIAN_POINT ( 'NONE',  ( -7.157701736792966507, -21.45640540170154509, -1.500000000000002220 ) ) ;
#59715 = AXIS2_PLACEMENT_3D ( 'NONE', #61264, #94182, #86577 ) ;
#59716 = B_SPLINE_CURVE_WITH_KNOTS ( 'NONE', 3,
 ( #28679, #91070, #53027, #44416, #5343, #84453, #21546, #37789, #52519, #37296, #75339, #29673, #68741, #91564, #36299 ),
 .UNSPECIFIED., .F., .F.,
 ( 4, 1, 1, 1, 1, 1, 1, 1, 1, 1, 1, 1, 4 ),
 ( 0.000000000000000000, 0.07176606415833945707, 0.1412255357663688426, 0.2091158524974623678, 0.2748396534685264014, 0.3394829303752206484, 0.4024762667353993240, 0.4649418891713267277, 0.5268326406463827993, 0.6474148160608228508, 0.7655615117859491114, 0.8816150870393308914, 1.000000000000000000 ),
 .UNSPECIFIED. ) ;
#59718 = ORIENTED_EDGE ( 'NONE', *, *, #91676, .F. ) ;
#59717 = CARTESIAN_POINT ( 'NONE',  ( -88.62287095715004170, -29.50247984919015209, -1.443849546365051806 ) ) ;
#59719 = ORIENTED_EDGE ( 'NONE', *, *, #35373, .T. ) ;
#59720 = B_SPLINE_CURVE_WITH_KNOTS ( 'NONE', 3,
 ( #53981, #29629, #38234, #6785 ),
 .UNSPECIFIED., .F., .F.,
 ( 4, 4 ),
 ( 0.000000000000000000, 9.999999999998897304E-05 ),
 .UNSPECIFIED. ) ;
#59721 = DIRECTION ( 'NONE',  ( 0.000000000000000000, 0.000000000000000000, 1.000000000000000000 ) ) ;
#59722 = CARTESIAN_POINT ( 'NONE',  ( -11.83016301840747175, -16.26703346747452983, 11.49999999999998934 ) ) ;
#59723 = CARTESIAN_POINT ( 'NONE',  ( -57.51495926866731168, -23.73791477778911840, 11.05961554403170588 ) ) ;
#59724 = EDGE_LOOP ( 'NONE', ( #43121, #94627, #81928, #100349 ) ) ;
#59725 = VECTOR ( 'NONE', #13805, 1000.000000000000114 ) ;
#59726 = CARTESIAN_POINT ( 'NONE',  ( -40.25541618970063240, -25.29345417698259624, 5.538673509577355603 ) ) ;
#59727 = CARTESIAN_POINT ( 'NONE',  ( -3.941980378682776287, 21.93750326593198352, -1.500000000000002220 ) ) ;
#59728 = DIRECTION ( 'NONE',  ( 0.000000000000000000, 1.000000000000000000, 0.000000000000000000 ) ) ;
#59729 = EDGE_LOOP ( 'NONE', ( #48206, #5969, #21020, #47833 ) ) ;
#59730 = CARTESIAN_POINT ( 'NONE',  ( -29.49875734969025842, -0.3587747205144265483, 25.61802280011862720 ) ) ;
#59731 = DIRECTION ( 'NONE',  ( 0.000000000000000000, 0.9999999999976377785, 2.173523156925979975E-06 ) ) ;
#59732 = CARTESIAN_POINT ( 'NONE',  ( -27.61175609890311478, -24.59808689224374589, 1.630391722295341461 ) ) ;
#59733 = CARTESIAN_POINT ( 'NONE',  ( -111.5895376238167245, -24.65952944569304606, 1.056160979905705455 ) ) ;
#59734 = CARTESIAN_POINT ( 'NONE',  ( -129.5228709571500474, -24.66019654487199730, 8.947790411086115725 ) ) ;
#59736 = VECTOR ( 'NONE', #18448, 1000.000000000000000 ) ;
#59735 = CARTESIAN_POINT ( 'NONE',  ( -19.08498223313328168, 4.104482590468319536, -1.500000000000002220 ) ) ;
#59737 = CARTESIAN_POINT ( 'NONE',  ( -21.39523464106120088, -1.845724655749456433, 11.49999999999998934 ) ) ;
#59738 = CARTESIAN_POINT ( 'NONE',  ( -2.780940648273603433, -5.876774720514411854, 20.02088365235843881 ) ) ;
#59739 = CARTESIAN_POINT ( 'NONE',  ( -120.5228709571500332, -24.15431212366390312, -0.2830839119429085504 ) ) ;
#59740 = CARTESIAN_POINT ( 'NONE',  ( -125.6228709571500843, -25.00182538069146432, 7.747789668545100206 ) ) ;
#59741 = CARTESIAN_POINT ( 'NONE',  ( 13.80103769381473811, 18.14473668730428813, -1.500000000000002220 ) ) ;
#59742 = B_SPLINE_CURVE_WITH_KNOTS ( 'NONE', 3,
 ( #3779, #48952, #42353, #88008, #73285, #32710 ),
 .UNSPECIFIED., .F., .F.,
 ( 4, 2, 4 ),
 ( 6.384118678611711726E-06, 0.001386860460828375418, 0.002767336802978138856 ),
 .UNSPECIFIED. ) ;
#59743 = CALENDAR_DATE ( 2026, 9, 10 ) ;
#59744 = CARTESIAN_POINT ( 'NONE',  ( -106.5572848214566477, -23.73791477778912551, 11.05961554403169700 ) ) ;
#59745 = CARTESIAN_POINT ( 'NONE',  ( 31.31283134548411340, 4.772774720514425972, -10.20862453625735533 ) ) ;
#59746 = CARTESIAN_POINT ( 'NONE',  ( 16.79105032741591330, -10.77411451815220822, 11.49999999999999645 ) ) ;
#59747 = CARTESIAN_POINT ( 'NONE',  ( -118.5228709571501184, -24.66019654487200441, 8.947790411086110396 ) ) ;
#59748 = ADVANCED_FACE ( 'NONE', ( #99365 ), #94633, .F. ) ;
#59749 = EDGE_CURVE ( 'NONE', #33110, #5456, #87022, .T. ) ;
#59750 = CARTESIAN_POINT ( 'NONE',  ( -57.55620429048338593, -23.48786465467241413, 11.44779295918254824 ) ) ;
#59751 = DIRECTION ( 'NONE',  ( -1.000000000000000000, -3.773278334444167608E-23, -8.201307833595939069E-29 ) ) ;
#59752 = ORIENTED_EDGE ( 'NONE', *, *, #5960, .F. ) ;
#59753 = CARTESIAN_POINT ( 'NONE',  ( -26.49745401032653191, -24.63815014598046460, 2.058893537102744364 ) ) ;
#59754 = CARTESIAN_POINT ( 'NONE',  ( -59.52287095715006160, -24.65952944569304961, 1.056160979905695463 ) ) ;
#59755 = EDGE_CURVE ( 'NONE', #66631, #3013, #51285, .T. ) ;
#59756 = CARTESIAN_POINT ( 'NONE',  ( 14.84582651547613352, 15.88809324551894520, 11.49999999999998934 ) ) ;
#59757 = CYLINDRICAL_SURFACE ( 'NONE', #26956, 27.94799999999999685 ) ;
#59758 = CARTESIAN_POINT ( 'NONE',  ( 19.11985901488480621, -4.296470200863222288, -1.500000000000002220 ) ) ;
#59759 = EDGE_CURVE ( 'NONE', #58114, #48360, #22230, .T. ) ;
#59760 = CARTESIAN_POINT ( 'NONE',  ( -69.52287095715006160, -29.50250243563736774, 8.947779886222143375 ) ) ;
#59761 = VERTEX_POINT ( 'NONE', #53214 ) ;
#59762 = DATE_AND_TIME ( #83570, #79889 ) ;
#59763 = CARTESIAN_POINT ( 'NONE',  ( 13.74975846015576586, -6.475225279485573360, -27.72022515045486557 ) ) ;
#59764 = CARTESIAN_POINT ( 'NONE',  ( 26.73860345374794889, 5.162006989575464999, -6.453654992509125776 ) ) ;
#59765 = CARTESIAN_POINT ( 'NONE',  ( 10.21088607376515789, 17.76353854702842483, 11.49999999999999645 ) ) ;
#59766 = CARTESIAN_POINT ( 'NONE',  ( -47.52287095715006870, -23.73934037231757088, 11.05740245334329508 ) ) ;
#59767 = B_SPLINE_CURVE_WITH_KNOTS ( 'NONE', 3,
 ( #61704, #92628, #13505, #23106 ),
 .UNSPECIFIED., .F., .F.,
 ( 4, 4 ),
 ( 0.000000000000000000, 9.999999999997510880E-05 ),
 .UNSPECIFIED. ) ;
#59768 = CARTESIAN_POINT ( 'NONE',  ( -40.62287095715005592, -23.48783264082478084, -1.443836473390072817 ) ) ;
#59769 = EDGE_CURVE ( 'NONE', #24728, #29559, #9394, .T. ) ;
#59770 = ORIENTED_EDGE ( 'NONE', *, *, #22393, .F. ) ;
#59771 = CARTESIAN_POINT ( 'NONE',  ( -117.6228709571500559, -29.50247984919015209, -1.443849546365046699 ) ) ;
#59772 = CARTESIAN_POINT ( 'NONE',  ( 19.75748517575715368, 0.3587747205144265483, 28.87153971905864580 ) ) ;
#59773 = AXIS2_PLACEMENT_3D ( 'NONE', #4617, #51784, #66539 ) ;
#59774 = CARTESIAN_POINT ( 'NONE',  ( -78.62287095715005592, -23.94994826722515668, -0.6494450866351704210 ) ) ;
#59775 = VECTOR ( 'NONE', #11856, 1000.000000000000114 ) ;
#59776 = CARTESIAN_POINT ( 'NONE',  ( -49.52287095715006160, -29.50247984919015209, -1.443849546365058689 ) ) ;
#59777 = ORIENTED_EDGE ( 'NONE', *, *, #3284, .F. ) ;
#59778 = DIRECTION ( 'NONE',  ( 1.000000000000000000, -0.000000000000000000, -0.000000000000000000 ) ) ;
#59779 = VECTOR ( 'NONE', #20723, 1000.000000000000114 ) ;
#59780 = CARTESIAN_POINT ( 'NONE',  ( -7.156825135384894843, 21.90021990432103038, 11.49999999999999645 ) ) ;
#59781 = CARTESIAN_POINT ( 'NONE',  ( -15.20078144808659992, 16.97451310947862169, -1.500000000000002220 ) ) ;
#59782 = CARTESIAN_POINT ( 'NONE',  ( 3.036358173076929123, -6.376774720514420736, 20.87990785256409865 ) ) ;
#59783 = CARTESIAN_POINT ( 'NONE',  ( 33.74607884027702909, -0.3587747205144265483, -4.999864028243830916 ) ) ;
#59784 = CARTESIAN_POINT ( 'NONE',  ( 2.499999999999995115, 19.99999999999999645, 0.000000000000000000 ) ) ;
#59785 = VECTOR ( 'NONE', #74966, 1000.000000000000114 ) ;
#59786 = B_SPLINE_CURVE_WITH_KNOTS ( 'NONE', 3,
 ( #33325, #26725, #65320, #8121, #499, #4, #31451, #61915, #96241, #92840, #17610, #23323, #54308, #2904, #85234, #15722 ),
 .UNSPECIFIED., .F., .F.,
 ( 4, 2, 2, 2, 2, 2, 2, 4 ),
 ( 0.000000000000000000, 0.0001736386538236284779, 0.0003472773076472569559, 0.0006945546152945145622, 0.0008681932691181433112, 0.001041831922941772277, 0.001215470576765400809, 0.001389109230589029775 ),
 .UNSPECIFIED. ) ;
#59787 = CARTESIAN_POINT ( 'NONE',  ( -108.8968792378191921, -25.05712065398430966, 7.447789548358837663 ) ) ;
#59788 = CARTESIAN_POINT ( 'NONE',  ( -110.5124727292759985, -24.73486907724917572, 1.287355809206965240 ) ) ;
#59789 = CARTESIAN_POINT ( 'NONE',  ( -17.52905966558703454, -13.16386835867055716, 11.49999999999998934 ) ) ;
#59790 = CARTESIAN_POINT ( 'NONE',  ( 6.955725288069978696, -5.876774720514425177, 21.70430095680336890 ) ) ;
#59791 = FACE_OUTER_BOUND ( 'NONE', #53088, .T. ) ;
#59792 = CARTESIAN_POINT ( 'NONE',  ( -41.46611000704998418, -25.28830591450888932, 4.188173661249235735 ) ) ;
#59793 = CARTESIAN_POINT ( 'NONE',  ( -86.62287095715004170, -29.50250786944525672, 11.44777988621623344 ) ) ;
#59794 = DIRECTION ( 'NONE',  ( -3.773278334453079030E-23, 0.9999999999976377785, 2.173523156925979128E-06 ) ) ;
#59795 = CARTESIAN_POINT ( 'NONE',  ( -101.3738023147422780, -29.50249165161862663, 3.986241424695394109 ) ) ;
#59796 = EDGE_LOOP ( 'NONE', ( #65453, #21606, #91156, #2269 ) ) ;
#59797 = VECTOR ( 'NONE', #67885, 1000.000000000000000 ) ;
#59798 = CARTESIAN_POINT ( 'NONE',  ( 5.028806042385554953, -19.83023610923392610, -1.500000000000002220 ) ) ;
#59799 = ORIENTED_EDGE ( 'NONE', *, *, #29676, .F. ) ;
#59800 = ORIENTED_EDGE ( 'NONE', *, *, #41708, .F. ) ;
#59801 = EDGE_LOOP ( 'NONE', ( #8517, #6365, #15714, #24483 ) ) ;
#59802 = ORIENTED_EDGE ( 'NONE', *, *, #61338, .T. ) ;
#59803 = CARTESIAN_POINT ( 'NONE',  ( 21.75825945658488436, -7.631246777643061030, 11.49999999999998934 ) ) ;
#59804 = CARTESIAN_POINT ( 'NONE',  ( -95.55620429048339304, -25.00158670708909980, 2.256160236439165967 ) ) ;
#59805 = CARTESIAN_POINT ( 'NONE',  ( -18.82339984186270598, 7.397194320553815317, -1.500000000000002220 ) ) ;
#59806 = ORIENTED_EDGE ( 'NONE', *, *, #22607, .T. ) ;
#59807 = CARTESIAN_POINT ( 'NONE',  ( 0.6000000000000007550, 0.000000000000000000, 0.000000000000000000 ) ) ;
#59808 = CARTESIAN_POINT ( 'NONE',  ( -41.86767815140794369, -25.29562010035766662, 4.300008416864591787 ) ) ;
#59809 = EDGE_CURVE ( 'NONE', #77123, #97163, #17503, .T. ) ;
#59810 = CARTESIAN_POINT ( 'NONE',  ( -101.5228709571500900, -24.66019654487200441, 8.947790411086119278 ) ) ;
#59811 = CARTESIAN_POINT ( 'NONE',  ( -70.62989412486773233, -24.73486907724917572, 1.287355809206963908 ) ) ;
#59813 = ORIENTED_EDGE ( 'NONE', *, *, #25363, .T. ) ;
#59812 = CARTESIAN_POINT ( 'NONE',  ( -2.751442626040462081, 21.25944542233241563, 11.49999999999999645 ) ) ;
#59814 = CARTESIAN_POINT ( 'NONE',  ( -61.62287095715004881, -29.50250243563736774, 8.947779886222145151 ) ) ;
#59815 = ORIENTED_EDGE ( 'NONE', *, *, #44583, .F. ) ;
#59816 = CARTESIAN_POINT ( 'NONE',  ( 2.909938941155331360, -20.50406750007545398, -1.500000000000002220 ) ) ;
#59817 = EDGE_CURVE ( 'NONE', #43562, #70264, #71309, .T. ) ;
#59819 = ORIENTED_EDGE ( 'NONE', *, *, #16697, .F. ) ;
#59818 = VECTOR ( 'NONE', #55636, 1000.000000000000000 ) ;
#59820 = DIRECTION ( 'NONE',  ( 0.000000000000000000, 1.478457507934778393E-16, -1.000000000000000000 ) ) ;
#59821 = ORIENTED_EDGE ( 'NONE', *, *, #29719, .T. ) ;
#59822 = CARTESIAN_POINT ( 'NONE',  ( -3.108974358974359475, -5.876774720514418071, 20.36458333333334281 ) ) ;
#59823 = ORIENTED_EDGE ( 'NONE', *, *, #94734, .F. ) ;
#59824 = CARTESIAN_POINT ( 'NONE',  ( -20.94189920129180038, 1.864940847883316488, -1.500000000000002220 ) ) ;
#59825 = CARTESIAN_POINT ( 'NONE',  ( -15.01370250125036421, 16.05796621403891677, 11.49999999999999645 ) ) ;
#59826 = FACE_OUTER_BOUND ( 'NONE', #19123, .T. ) ;
#59827 = CARTESIAN_POINT ( 'NONE',  ( -0.06565682164858396841, -22.51586213336150166, -1.500000000000002220 ) ) ;
#59828 = CARTESIAN_POINT ( 'NONE',  ( 0.9685562702117149758, 20.96446713366763248, 11.49999999999998934 ) ) ;
#59829 = CARTESIAN_POINT ( 'NONE',  ( 5.642655980204820843, -6.376774720514418959, 20.71586687040766961 ) ) ;
#59830 = CARTESIAN_POINT ( 'NONE',  ( -72.62287095715008434, -24.50216790748099527, 0.6166512839513557109 ) ) ;
#59831 = CARTESIAN_POINT ( 'NONE',  ( -53.62287095715004881, -23.48786465467241058, 11.44779295918255002 ) ) ;
#59832 = ORIENTED_EDGE ( 'NONE', *, *, #9734, .T. ) ;
#59833 = ORIENTED_EDGE ( 'NONE', *, *, #9226, .F. ) ;
#59834 = VERTEX_POINT ( 'NONE', #15134 ) ;
#59835 = FACE_OUTER_BOUND ( 'NONE', #36574, .T. ) ;
#59836 = ADVANCED_BREP_SHAPE_REPRESENTATION ( '', ( #76408, #37391 ), #82851 ) ;
#59837 = CARTESIAN_POINT ( 'NONE',  ( 15.25824911148008844, 15.06768998368162471, -1.500000000000002220 ) ) ;
#59838 = LINE ( 'NONE', #91272, #55383 ) ;
#59839 = ORIENTED_EDGE ( 'NONE', *, *, #44755, .F. ) ;
#59840 = CARTESIAN_POINT ( 'NONE',  ( -12.37649675270136918, 17.12833386298736471, 11.49999999999998934 ) ) ;
#59841 = LINE ( 'NONE', #27879, #7700 ) ;
#59842 = AXIS2_PLACEMENT_3D ( 'NONE', #40686, #76353, #22556 ) ;
#59843 = CARTESIAN_POINT ( 'NONE',  ( -64.56596238235714225, -23.48783264082477018, -1.443836473390096353 ) ) ;
#59845 = CARTESIAN_POINT ( 'NONE',  ( -83.50633554728430852, -24.35071581493543036, 9.817618358456028815 ) ) ;
#59844 = AXIS2_PLACEMENT_3D ( 'NONE', #60164, #91086, #21562 ) ;
#59846 = FACE_OUTER_BOUND ( 'NONE', #7090, .T. ) ;
#59847 = CARTESIAN_POINT ( 'NONE',  ( -0.9257915630711897048, -5.876774720514409189, 19.25892998154168012 ) ) ;
#59848 = CARTESIAN_POINT ( 'NONE',  ( 22.02032638543937182, 1.892999326154024553, -1.500000000000002220 ) ) ;
#59849 = B_SPLINE_CURVE_WITH_KNOTS ( 'NONE', 3,
 ( #4834, #36287, #28666, #29160 ),
 .UNSPECIFIED., .F., .F.,
 ( 4, 4 ),
 ( 0.000000000000000000, 9.999999999998897304E-05 ),
 .UNSPECIFIED. ) ;
#59850 = FACE_OUTER_BOUND ( 'NONE', #380, .T. ) ;
#59851 = CARTESIAN_POINT ( 'NONE',  ( -3.108787716482549701, -6.376774720514417183, 20.32624910079993086 ) ) ;
#59852 = CARTESIAN_POINT ( 'NONE',  ( -34.22287095715005734, -23.47593901973090169, -1.443836447538998202 ) ) ;
#59853 = PLANE ( 'NONE',  #46867 ) ;
#59854 = AXIS2_PLACEMENT_3D ( 'NONE', #57079, #94617, #89013 ) ;
#59855 = CARTESIAN_POINT ( 'NONE',  ( -100.5179258051187787, -23.85016227208580375, -0.8807180028928297544 ) ) ;
#59856 = AXIS2_PLACEMENT_3D ( 'NONE', #52407, #61530, #83343 ) ;
#59857 = CARTESIAN_POINT ( 'NONE',  ( 3.148799746435844593, 19.17640706095922098, 11.49999999999998934 ) ) ;
#59858 = VECTOR ( 'NONE', #37053, 1000.000000000000114 ) ;
#59859 = CARTESIAN_POINT ( 'NONE',  ( 12.64048258313813733, 17.25876517447949610, -1.500000000000002220 ) ) ;
#59860 = LINE ( 'NONE', #44625, #35316 ) ;
#59861 = CARTESIAN_POINT ( 'NONE',  ( -68.62287095715005592, -29.50250786944525672, 11.44777988621623699 ) ) ;
#59862 = CARTESIAN_POINT ( 'NONE',  ( -72.52287095715007581, -24.50321055353804667, 9.387540953477529371 ) ) ;
#59863 = CARTESIAN_POINT ( 'NONE',  ( -128.9228709571500815, -23.47593901973090524, -1.443836447538996204 ) ) ;
#59864 = B_SPLINE_CURVE_WITH_KNOTS ( 'NONE', 3,
 ( #99372, #59327, #60344, #35984, #44103, #75529 ),
 .UNSPECIFIED., .F., .F.,
 ( 4, 2, 4 ),
 ( 1.570887131794795405E-05, 0.001396322306279761940, 0.002776935741241575838 ),
 .UNSPECIFIED. ) ;
#59865 = CARTESIAN_POINT ( 'NONE',  ( -14.08738070862771963, 17.71811851510361535, -1.500000000000002220 ) ) ;
#59866 = EDGE_LOOP ( 'NONE', ( #71612, #11183, #15860, #28739 ) ) ;
#59867 = CARTESIAN_POINT ( 'NONE',  ( 4.016587897052070311, -5.876774720514425177, 21.44459449800855921 ) ) ;
#59868 = CARTESIAN_POINT ( 'NONE',  ( -40.92287095715006018, -23.47596703998600276, 11.44779298504227683 ) ) ;
#59869 = CARTESIAN_POINT ( 'NONE',  ( 18.78060722631472501, -6.265068672152646734, 11.49999999999999645 ) ) ;
#59870 = DIRECTION ( 'NONE',  ( -0.8264557562326033668, -6.845827386180409975E-16, -0.5630016722799281448 ) ) ;
#59871 = EDGE_CURVE ( 'NONE', #50459, #79998, #34401, .T. ) ;
#59872 = CARTESIAN_POINT ( 'NONE',  ( -35.55620429048339304, -25.00158670708909270, 2.256160236439165967 ) ) ;
#59873 = ORIENTED_EDGE ( 'NONE', *, *, #38191, .F. ) ;
#59874 = CARTESIAN_POINT ( 'NONE',  ( -53.62287095715004881, -24.65952944569303895, 1.056160979905692576 ) ) ;
#59875 = CARTESIAN_POINT ( 'NONE',  ( -78.94303308397306296, -25.26612693627497208, 5.977536690229215743 ) ) ;
#59876 = EDGE_CURVE ( 'NONE', #69684, #16998, #1696, .T. ) ;
#59877 = LINE ( 'NONE', #75070, #56145 ) ;
#59878 = CARTESIAN_POINT ( 'NONE',  ( -13.25059585359799108, -17.08168364658555305, -1.500000000000002220 ) ) ;
#59879 = FACE_OUTER_BOUND ( 'NONE', #809, .T. ) ;
#59880 = CARTESIAN_POINT ( 'NONE',  ( -101.5895376238167245, -23.48786465467242479, 11.44779295918254114 ) ) ;
#59881 = ADVANCED_FACE ( 'NONE', ( #21733 ), #83644, .F. ) ;
#59882 = DIRECTION ( 'NONE',  ( 0.000000000000000000, 0.9999999999976377785, 2.173523156925979128E-06 ) ) ;
#59883 = PLANE ( 'NONE',  #31223 ) ;
#59884 = CARTESIAN_POINT ( 'NONE',  ( -14.51517298184297289, -13.48802281452852725, 11.49999999999998934 ) ) ;
#59885 = ORIENTED_EDGE ( 'NONE', *, *, #58278, .F. ) ;
#59886 = EDGE_CURVE ( 'NONE', #86736, #3834, #9153, .T. ) ;
#59887 = CARTESIAN_POINT ( 'NONE',  ( 14.56535739210195857, -14.21638276092092745, 11.49999999999999645 ) ) ;
#59888 = CARTESIAN_POINT ( 'NONE',  ( 6.184520403203634942, 6.376774720514426953, -25.32021290018218451 ) ) ;
#59889 = EDGE_CURVE ( 'NONE', #81557, #50597, #49962, .T. ) ;
#59890 = FACE_OUTER_BOUND ( 'NONE', #17070, .T. ) ;
#59891 = ORIENTED_EDGE ( 'NONE', *, *, #75986, .F. ) ;
#59892 = B_SPLINE_SURFACE_WITH_KNOTS ( 'NONE', 3, 1, ( 
 ( #49624, #47621 ),
 ( #11049, #42013 ),
 ( #86167, #72956 ),
 ( #3452, #78538 ),
 ( #86665, #70956 ),
 ( #32382, #9543 ),
 ( #40505, #19149 ),
 ( #43988, #42513 ),
 ( #90166, #19645 ),
 ( #5424, #73451 ),
 ( #36376, #28765 ) ),
 .UNSPECIFIED., .F., .F., .F.,
 ( 4, 1, 1, 1, 1, 1, 1, 1, 4 ),
 ( 2, 2 ),
 ( 0.000000000000000000, 0.1192834503733694734, 0.2370928820686294958, 0.3547960442151275040, 0.4745763009408505706, 0.5974600658149772370, 0.7249261546156138269, 0.8588831991927623477, 1.000000000000000000 ),
 ( 0.000000000000000000, 1.000000000000000000 ),
 .UNSPECIFIED. ) ;
#59893 = CARTESIAN_POINT ( 'NONE',  ( -102.5602270407120926, -23.48786465467241058, 11.44779295918254292 ) ) ;
#59894 = CARTESIAN_POINT ( 'NONE',  ( 11.86515846156731335, -5.152774720514426754, -28.09350142571734921 ) ) ;
#59895 = CARTESIAN_POINT ( 'NONE',  ( -75.62287095715005592, -23.48783264082478084, -1.443836473390065489 ) ) ;
#59896 = CARTESIAN_POINT ( 'NONE',  ( 14.76093561896379214, 5.965225279485572685, -26.55548769130089681 ) ) ;
#59897 = CARTESIAN_POINT ( 'NONE',  ( 32.98733314340959311, -0.3587747205144265483, 2.074222136288530027 ) ) ;
#59898 = CARTESIAN_POINT ( 'NONE',  ( -1.290058840521481454, 20.04182742388497473, -1.500000000000002220 ) ) ;
#59899 = EDGE_CURVE ( 'NONE', #79071, #30912, #59742, .T. ) ;
#59900 = CARTESIAN_POINT ( 'NONE',  ( -79.55620429048342146, -23.47593901973091235, -1.443836447539004642 ) ) ;
#59901 = ORIENTED_EDGE ( 'NONE', *, *, #40383, .T. ) ;
#59902 = DIRECTION ( 'NONE',  ( 0.000000000000000000, 0.000000000000000000, -1.000000000000000000 ) ) ;
#59903 = CARTESIAN_POINT ( 'NONE',  ( 15.09361930729867574, -17.17024899132524496, 11.49999999999999645 ) ) ;
#59904 = CARTESIAN_POINT ( 'NONE',  ( -49.51279233427662518, -25.31297074183165563, 4.076580152408665114 ) ) ;
#59905 = CYLINDRICAL_SURFACE ( 'NONE', #62333, 1.149999999999998135 ) ;
#59906 = DIRECTION ( 'NONE',  ( 0.000000000000000000, 0.000000000000000000, -1.000000000000000000 ) ) ;
#59907 = DIRECTION ( 'NONE',  ( 0.000000000000000000, -1.000000000000000000, -8.393823270855521221E-16 ) ) ;
#59908 = AXIS2_PLACEMENT_3D ( 'NONE', #48128, #435, #39507 ) ;
#59909 = FACE_OUTER_BOUND ( 'NONE', #62413, .T. ) ;
#59910 = CARTESIAN_POINT ( 'NONE',  ( -99.90881925540746522, -25.03707831087709934, 7.590867751134624974 ) ) ;
#59911 = ORIENTED_EDGE ( 'NONE', *, *, #63607, .F. ) ;
#59912 = AXIS2_PLACEMENT_3D ( 'NONE', #98449, #36558, #69015 ) ;
#59913 = CARTESIAN_POINT ( 'NONE',  ( -0.9335293527496063559, -20.33857301660709638, -1.500000000000002220 ) ) ;
#59914 = VERTEX_POINT ( 'NONE', #79382 ) ;
#59915 = EDGE_CURVE ( 'NONE', #53379, #27734, #44105, .T. ) ;
#59916 = CARTESIAN_POINT ( 'NONE',  ( 13.56796309060646166, -18.52494293750034871, -1.500000000000002220 ) ) ;
#59917 = DIRECTION ( 'NONE',  ( 0.000000000000000000, 0.9999999999976377785, 2.173523156925979975E-06 ) ) ;
#59918 = ORIENTED_EDGE ( 'NONE', *, *, #43030, .T. ) ;
#59919 = VECTOR ( 'NONE', #10283, 1000.000000000000114 ) ;
#59920 = CARTESIAN_POINT ( 'NONE',  ( -49.10457154551148307, -25.26416398485831749, 3.999772271414141489 ) ) ;
#59922 = EDGE_CURVE ( 'NONE', #74381, #39047, #26972, .T. ) ;
#59921 = DIRECTION ( 'NONE',  ( 0.000000000000000000, 0.000000000000000000, -1.000000000000000000 ) ) ;
#59923 = VECTOR ( 'NONE', #64453, 1000.000000000000000 ) ;
#59924 = CARTESIAN_POINT ( 'NONE',  ( -74.55620429048340725, -23.47593901973091235, -1.443836447539006196 ) ) ;
#59926 = ORIENTED_EDGE ( 'NONE', *, *, #89279, .T. ) ;
#59925 = CARTESIAN_POINT ( 'NONE',  ( -20.48789480994130230, 5.740754632170482097, 11.49999999999999645 ) ) ;
#59927 = AXIS2_PLACEMENT_3D ( 'NONE', #89320, #64013, #17810 ) ;
#59928 = VERTEX_POINT ( 'NONE', #34717 ) ;
#59929 = CARTESIAN_POINT ( 'NONE',  ( 9.107982344273736430, -20.20341329189913537, -1.500000000000002220 ) ) ;
#59930 = CARTESIAN_POINT ( 'NONE',  ( -20.60850594246137035, -0.7621957659720622891, -1.500000000000002220 ) ) ;
#59932 = ORIENTED_EDGE ( 'NONE', *, *, #85079, .T. ) ;
#59931 = VECTOR ( 'NONE', #77762, 1000.000000000000000 ) ;
#59933 = VERTEX_POINT ( 'NONE', #48452 ) ;
#59934 = DIRECTION ( 'NONE',  ( -1.000000000000000000, -3.773278334444167608E-23, -8.201307833595939069E-29 ) ) ;
#59935 = ADVANCED_FACE ( 'NONE', ( #65692 ), #10881, .T. ) ;
#59936 = CARTESIAN_POINT ( 'NONE',  ( -121.6228709571500417, -23.48783264082478794, -1.443836473390058384 ) ) ;
#59937 = VERTEX_POINT ( 'NONE', #94612 ) ;
#59938 = ORIENTED_EDGE ( 'NONE', *, *, #70134, .T. ) ;
#59939 = CARTESIAN_POINT ( 'NONE',  ( -49.52287095715007581, -23.95044443724991723, 10.65354141964649592 ) ) ;
#59940 = FACE_OUTER_BOUND ( 'NONE', #61317, .T. ) ;
#59941 = CARTESIAN_POINT ( 'NONE',  ( 14.47435193673551090, -3.621805754661552523, -28.36943713414519763 ) ) ;
#59942 = CARTESIAN_POINT ( 'NONE',  ( -16.75865769207039335, -12.26659692683164593, -1.500000000000002220 ) ) ;
#59944 = ADVANCED_FACE ( 'NONE', ( #49459 ), #18488, .T. ) ;
#59943 = CARTESIAN_POINT ( 'NONE',  ( 21.06710269851327766, -5.618397932909799941, 11.49999999999999645 ) ) ;
#59945 = CARTESIAN_POINT ( 'NONE',  ( -50.60256128385139363, -25.03406269411437179, 7.557545390615620029 ) ) ;
#59946 = DIRECTION ( 'NONE',  ( -1.000000000000000000, 0.000000000000000000, 0.000000000000000000 ) ) ;
#59947 = CARTESIAN_POINT ( 'NONE',  ( -96.58953762381671027, -24.65952944569304606, 1.056160979905704123 ) ) ;
#59948 = CARTESIAN_POINT ( 'NONE',  ( 20.43785579724129420, 9.289222182981756504, 11.49999999999998934 ) ) ;
#59949 = FACE_OUTER_BOUND ( 'NONE', #18108, .T. ) ;
#59950 = ORIENTED_EDGE ( 'NONE', *, *, #67369, .F. ) ;
#59951 = PLANE ( 'NONE',  #56667 ) ;
#59952 = CARTESIAN_POINT ( 'NONE',  ( -51.70072539166533687, -25.26311289191998455, 3.987152081390995306 ) ) ;
#59953 = ORIENTED_EDGE ( 'NONE', *, *, #99252, .F. ) ;
#59954 = VERTEX_POINT ( 'NONE', #27104 ) ;
#59955 = CARTESIAN_POINT ( 'NONE',  ( -99.63657171274012114, -25.30666370342169813, 5.471494451533469139 ) ) ;
#59956 = APPROVAL ( #75693, 'UNSPECIFIED' ) ;
#59957 = VERTEX_POINT ( 'NONE', #79881 ) ;
#59958 = CARTESIAN_POINT ( 'NONE',  ( -16.96849063341007380, -12.82450338531451450, -1.500000000000002220 ) ) ;
#59959 = ORIENTED_EDGE ( 'NONE', *, *, #83202, .F. ) ;
#59960 = DIRECTION ( 'NONE',  ( 0.000000000000000000, 0.000000000000000000, 1.000000000000000000 ) ) ;
#59961 = CARTESIAN_POINT ( 'NONE',  ( -14.15979099334852798, -15.53166555317341135, -1.500000000000002220 ) ) ;
#59962 = DIRECTION ( 'NONE',  ( 1.000000000000000000, -0.000000000000000000, -0.000000000000000000 ) ) ;
#59963 = CARTESIAN_POINT ( 'NONE',  ( -11.11902432501355342, 19.77583997595719367, 11.49999999999998934 ) ) ;
#59964 = CARTESIAN_POINT ( 'NONE',  ( -41.46611000704998418, -25.18431065692472615, 4.188173887285336683 ) ) ;
#59965 = CARTESIAN_POINT ( 'NONE',  ( 5.109298100548420152, -3.316774720514426456, -27.55941679637948383 ) ) ;
#59966 = CARTESIAN_POINT ( 'NONE',  ( 6.492371748702247203, -20.92784845389783399, -1.500000000000002220 ) ) ;
#59967 = CARTESIAN_POINT ( 'NONE',  ( -62.62287095715004881, -23.47596703998600276, 11.44779298504227505 ) ) ;
#59968 = ORIENTED_EDGE ( 'NONE', *, *, #29489, .T. ) ;
#59969 = CARTESIAN_POINT ( 'NONE',  ( 29.68604458549361169, -6.066877414785177614, 27.51520267613161153 ) ) ;
#59970 = DIRECTION ( 'NONE',  ( -1.000000000000000000, -3.773278334444167608E-23, -8.201307833595939069E-29 ) ) ;
#59971 = CARTESIAN_POINT ( 'NONE',  ( -130.5728709571500872, -25.14081846633249739, 7.291654623549849390 ) ) ;
#59972 = CARTESIAN_POINT ( 'NONE',  ( -46.62287095715004881, -29.50250243563736774, 8.947779886222146928 ) ) ;
#59973 = B_SPLINE_CURVE_WITH_KNOTS ( 'NONE', 3,
 ( #94466, #10232, #77720, #33074 ),
 .UNSPECIFIED., .F., .F.,
 ( 4, 4 ),
 ( 0.000000000000000000, 0.0001000000000000028644 ),
 .UNSPECIFIED. ) ;
#59974 = CARTESIAN_POINT ( 'NONE',  ( -9.505907188867841029, -19.02311915605711690, -1.500000000000002220 ) ) ;
#59975 = CARTESIAN_POINT ( 'NONE',  ( -112.6256797069762143, -24.34968618360934656, 0.1864209137779000991 ) ) ;
#59976 = CARTESIAN_POINT ( 'NONE',  ( -6.660000000000001030, -0.2368809837866516499, 5.288828319098142217 ) ) ;
#59977 = VECTOR ( 'NONE', #94099, 1000.000000000000000 ) ;
#59978 = CARTESIAN_POINT ( 'NONE',  ( -85.50025541002817420, -24.73486907724917927, 1.287355809206964796 ) ) ;
#59979 = CARTESIAN_POINT ( 'NONE',  ( -114.5228709571500616, -24.65952944569305316, 1.056160979905704123 ) ) ;
#59980 = CARTESIAN_POINT ( 'NONE',  ( -90.55620429048337883, -24.99132157543166599, 2.256160258750667058 ) ) ;
#59981 = ORIENTED_EDGE ( 'NONE', *, *, #70564, .F. ) ;
#59982 = CARTESIAN_POINT ( 'NONE',  ( -119.6228709571500417, -24.65952944569304961, 1.056160979905704789 ) ) ;
#59983 = CARTESIAN_POINT ( 'NONE',  ( 14.19269941865516671, -13.59168563846684563, 11.49999999999999645 ) ) ;
#59984 = CARTESIAN_POINT ( 'NONE',  ( -78.52287095715006160, -23.48786465467241769, 11.44779295918254469 ) ) ;
#59985 = CIRCLE ( 'NONE', #85897, 27.94799999999999685 ) ;
#59986 = EDGE_CURVE ( 'NONE', #57023, #45709, #56067, .T. ) ;
#59987 = CARTESIAN_POINT ( 'NONE',  ( -119.6228709571500559, -23.47593901973091235, -1.443836447538997536 ) ) ;
#59988 = VERTEX_POINT ( 'NONE', #65197 ) ;
#59989 = CARTESIAN_POINT ( 'NONE',  ( -55.62287095715005592, -29.50250786944525672, 11.44777988621623876 ) ) ;
#59990 = CARTESIAN_POINT ( 'NONE',  ( -44.62287095715004881, -24.65952944569303895, 1.056160979905693686 ) ) ;
#59991 = CIRCLE ( 'NONE', #97056, 0.8500000000000017542 ) ;
#59992 = CARTESIAN_POINT ( 'NONE',  ( -26.97977519014201064, -24.63279798339582172, 8.111117997598707774 ) ) ;
#59993 = CARTESIAN_POINT ( 'NONE',  ( -40.62287095715004170, -24.91570333823099048, 8.075032458375556388 ) ) ;
#59994 = CARTESIAN_POINT ( 'NONE',  ( -18.83419513347712737, -5.836681878196540829, 11.49999999999998934 ) ) ;
#59995 = VECTOR ( 'NONE', #34362, 1000.000000000000227 ) ;
#59996 = ORIENTED_EDGE ( 'NONE', *, *, #60899, .T. ) ;
#59997 = EDGE_CURVE ( 'NONE', #48335, #96746, #76782, .T. ) ;
#59998 = AXIS2_PLACEMENT_3D ( 'NONE', #17083, #76969, #63285 ) ;
#59999 = CARTESIAN_POINT ( 'NONE',  ( -33.62287095715005592, -29.50250786944525672, 11.44777988621624409 ) ) ;
#60000 = CARTESIAN_POINT ( 'NONE',  ( -70.62287095715004170, -24.15431212366388891, -0.2830839119429064410 ) ) ;
#60001 = EDGE_CURVE ( 'NONE', #41039, #82023, #80434, .T. ) ;
#60002 = AXIS2_PLACEMENT_3D ( 'NONE', #5176, #27023, #90413 ) ;
#60003 = PERSON_AND_ORGANIZATION ( #70597, #27821 ) ;
#60004 = ORIENTED_EDGE ( 'NONE', *, *, #26995, .T. ) ;
#60005 = CARTESIAN_POINT ( 'NONE',  ( -54.52287095715006870, -24.50321055353805377, 9.387540953477524042 ) ) ;
#60006 = AXIS2_PLACEMENT_3D ( 'NONE', #86608, #32323, #9984 ) ;
#60007 = DIRECTION ( 'NONE',  ( 0.000000000000000000, -1.224646799147353207E-16, 1.000000000000000000 ) ) ;
#60008 = CARTESIAN_POINT ( 'NONE',  ( -55.64123101047048436, -24.40034930558990922, 0.3402023900116022959 ) ) ;
#60009 = CARTESIAN_POINT ( 'NONE',  ( -50.52287095715006160, -24.99156044556120193, 7.747789690856173195 ) ) ;
#60010 = CARTESIAN_POINT ( 'NONE',  ( -31.62287095715005236, -23.47596703998600276, 11.44779298504227505 ) ) ;
#60011 = CARTESIAN_POINT ( 'NONE',  ( -70.06086327669997615, -25.31201598263180941, 5.348962284489573449 ) ) ;
#60012 = CARTESIAN_POINT ( 'NONE',  ( -91.52287095715006160, -24.50321055353804667, 9.387540953477515160 ) ) ;
#60013 = CARTESIAN_POINT ( 'NONE',  ( -19.59816365915598979, -3.832847594873297403, 11.49999999999998934 ) ) ;
#60014 = EDGE_CURVE ( 'NONE', #46913, #70257, #96120, .T. ) ;
#60015 = CARTESIAN_POINT ( 'NONE',  ( -125.6228709571500843, -24.52323809116984776, 9.355190652339411272 ) ) ;
#60016 = CARTESIAN_POINT ( 'NONE',  ( 30.93860345374796239, 5.965225279485572685, 28.07639619989137003 ) ) ;
#60017 = EDGE_LOOP ( 'NONE', ( #66304, #35880, #47166, #81976 ) ) ;
#60018 = CARTESIAN_POINT ( 'NONE',  ( -63.52287095715006160, -23.72747288104470087, -1.053458166803227014 ) ) ;
#60019 = DIRECTION ( 'NONE',  ( 0.000000000000000000, 1.000000000000000000, -0.000000000000000000 ) ) ;
#60020 = LINE ( 'NONE', #68122, #97217 ) ;
#60021 = DIRECTION ( 'NONE',  ( -0.000000000000000000, 1.000000000000000000, -0.000000000000000000 ) ) ;
#60022 = CARTESIAN_POINT ( 'NONE',  ( -28.55620429048340725, -24.49093714213148232, 1.056161671301197424 ) ) ;
#60023 = CARTESIAN_POINT ( 'NONE',  ( -39.63466154761483295, -24.34968618360933235, 0.1864209137778788383 ) ) ;
#60024 = CARTESIAN_POINT ( 'NONE',  ( -76.52287095715007581, -29.50247984919015209, -1.443849546365053582 ) ) ;
#60025 = CARTESIAN_POINT ( 'NONE',  ( -1.359251851468251449, -6.376774720514420736, 20.71116975788854120 ) ) ;
#60026 = ORIENTED_EDGE ( 'NONE', *, *, #9801, .T. ) ;
#60027 = B_SPLINE_CURVE_WITH_KNOTS ( 'NONE', 3,
 ( #72526, #74018, #19710, #3019, #12103, #82124, #95352, #4513 ),
 .UNSPECIFIED., .F., .F.,
 ( 4, 2, 2, 4 ),
 ( 6.384118678609614472E-06, 0.002007151183507257988, 0.003007534715921583810, 0.004007918248335909199 ),
 .UNSPECIFIED. ) ;
#60028 = LINE ( 'NONE', #82838, #64129 ) ;
#60029 = CARTESIAN_POINT ( 'NONE',  ( -93.52287095715006160, -29.50248528299804818, 1.056150453629040253 ) ) ;
#60030 = VERTEX_POINT ( 'NONE', #2283 ) ;
#60031 = CARTESIAN_POINT ( 'NONE',  ( -8.335131950130996614, 18.48905954037022781, 11.49999999999998934 ) ) ;
#60032 = CARTESIAN_POINT ( 'NONE',  ( 6.420673076923079314, -5.876774720514427841, 21.83974358974358765 ) ) ;
#60033 = CARTESIAN_POINT ( 'NONE',  ( 22.33191539159815164, 4.132774720514426292, -16.26852658953823649 ) ) ;
#60034 = LINE ( 'NONE', #43801, #99469 ) ;
#60035 = VERTEX_POINT ( 'NONE', #33213 ) ;
#60037 = EDGE_CURVE ( 'NONE', #56810, #33445, #64193, .T. ) ;
#60036 = CARTESIAN_POINT ( 'NONE',  ( -95.22287095715005023, -23.47596703998600631, 11.44779298504227860 ) ) ;
#60038 = CARTESIAN_POINT ( 'NONE',  ( -4.993225604111834137, 0.3587747205143964613, -29.11654937215279304 ) ) ;
#60039 = CARTESIAN_POINT ( 'NONE',  ( -12.91570554291229023, -15.35452705144416896, -1.500000000000002220 ) ) ;
#60040 = CARTESIAN_POINT ( 'NONE',  ( 5.126256225908648823, -20.47799061884807870, 11.49999999999999645 ) ) ;
#60041 = CARTESIAN_POINT ( 'NONE',  ( -28.24657929368988718, -24.87968172495813590, 7.481726558560294116 ) ) ;
#60042 = CARTESIAN_POINT ( 'NONE',  ( -70.55208003325599009, -24.15602025860895807, 10.28564288303535967 ) ) ;
#60043 = CARTESIAN_POINT ( 'NONE',  ( 14.53198226072946220, 16.64418356588832992, -1.500000000000002220 ) ) ;
#60044 = VECTOR ( 'NONE', #22102, 1000.000000000000000 ) ;
#60045 = EDGE_CURVE ( 'NONE', #27205, #18719, #33720, .T. ) ;
#60046 = CARTESIAN_POINT ( 'NONE',  ( -9.284664653622879626, 18.31210316397345395, -1.500000000000002220 ) ) ;
#60047 = DIRECTION ( 'NONE',  ( 3.773278334444166432E-23, -1.000000000000000000, 0.000000000000000000 ) ) ;
#60048 = EDGE_CURVE ( 'NONE', #82714, #98447, #64700, .T. ) ;
#60049 = CARTESIAN_POINT ( 'NONE',  ( 31.44923352942285177, 5.094381739198088788, -4.378347922178638107 ) ) ;
#60050 = CARTESIAN_POINT ( 'NONE',  ( -53.52287095715006870, -23.48786465467241058, 11.44779295918255002 ) ) ;
#60051 = EDGE_LOOP ( 'NONE', ( #55269, #79138 ) ) ;
#60052 = CARTESIAN_POINT ( 'NONE',  ( -89.40841769935761363, -25.36026716165461892, 4.902505258696291612 ) ) ;
#60053 = CARTESIAN_POINT ( 'NONE',  ( -29.58953762381673869, -23.39421443057875294, -1.443836134715248631 ) ) ;
#60054 = ORIENTED_EDGE ( 'NONE', *, *, #12289, .T. ) ;
#60055 = ORIENTED_EDGE ( 'NONE', *, *, #44106, .F. ) ;
#60056 = LINE ( 'NONE', #90983, #48624 ) ;
#60057 = LINE ( 'NONE', #74268, #77751 ) ;
#60058 = CARTESIAN_POINT ( 'NONE',  ( -76.49748031141828619, -24.65952944569303895, 1.056160979905700570 ) ) ;
#60059 = CARTESIAN_POINT ( 'NONE',  ( 11.80677006232881254, 16.86875346446678137, -1.500000000000002220 ) ) ;
#60060 = CARTESIAN_POINT ( 'NONE',  ( -15.55086147716002110, 14.89234021980106881, 11.49999999999999645 ) ) ;
#60061 = VERTEX_POINT ( 'NONE', #87505 ) ;
#60062 = FACE_OUTER_BOUND ( 'NONE', #28855, .T. ) ;
#60063 = DIRECTION ( 'NONE',  ( 0.000000000000000000, 0.9999999999976377785, 2.173523156925979975E-06 ) ) ;
#60064 = CARTESIAN_POINT ( 'NONE',  ( 20.23429811176546167, 9.490607074118958764, 11.49999999999998934 ) ) ;
#60065 = CARTESIAN_POINT ( 'NONE',  ( -34.52287095715007581, -24.51387760970724017, 9.387446482453404073 ) ) ;
#60066 = PLANE ( 'NONE',  #41622 ) ;
#60067 = ORIENTED_EDGE ( 'NONE', *, *, #7325, .T. ) ;
#60068 = CARTESIAN_POINT ( 'NONE',  ( -112.5228709571500616, -29.50250786944525672, 11.44777988621622988 ) ) ;
#60069 = AXIS2_PLACEMENT_3D ( 'NONE', #62595, #53497, #68709 ) ;
#60070 = CARTESIAN_POINT ( 'NONE',  ( -49.52204948630863157, -23.48786465467241058, 11.44779295918254824 ) ) ;
#60071 = VECTOR ( 'NONE', #85115, 1000.000000000000000 ) ;
#60072 = CARTESIAN_POINT ( 'NONE',  ( -2.496121100066326814, 20.73550571027955769, -1.500000000000002220 ) ) ;
#60073 = ORIENTED_EDGE ( 'NONE', *, *, #72679, .F. ) ;
#60074 = EDGE_CURVE ( 'NONE', #43349, #39981, #62622, .T. ) ;
#60076 = ORIENTED_EDGE ( 'NONE', *, *, #92289, .T. ) ;
#60075 = CARTESIAN_POINT ( 'NONE',  ( -98.62287095715007013, -23.72747288104442021, -1.053458166803661333 ) ) ;
#60077 = ORIENTED_EDGE ( 'NONE', *, *, #43587, .F. ) ;
#60078 = VECTOR ( 'NONE', #66859, 1000.000000000000000 ) ;
#60079 = CARTESIAN_POINT ( 'NONE',  ( -100.5838740427371789, -25.00182538069146787, 7.747789668545043362 ) ) ;
#60080 = CARTESIAN_POINT ( 'NONE',  ( 19.72786461798894209, 7.474574171381012100, -1.500000000000002220 ) ) ;
#60081 = ORIENTED_EDGE ( 'NONE', *, *, #77380, .F. ) ;
#60082 = CARTESIAN_POINT ( 'NONE',  ( -117.5893284022649965, -24.34968618360934656, 0.1864209137778901626 ) ) ;
#60083 = CARTESIAN_POINT ( 'NONE',  ( -99.78066557477396259, -25.12215640787303528, 6.943018770401670814 ) ) ;
#60084 = CARTESIAN_POINT ( 'NONE',  ( -9.857415191643349672, 19.42730305858377449, 11.49999999999998934 ) ) ;
#60085 = CARTESIAN_POINT ( 'NONE',  ( 9.616142118701272778, -1.335431525194935798, 19.26533332368850182 ) ) ;
#60086 = DIRECTION ( 'NONE',  ( -1.257682986112628908E-16, -0.000000000000000000, -1.000000000000000000 ) ) ;
#60087 = CARTESIAN_POINT ( 'NONE',  ( -10.34999999999997833, 22.00000000000000000, 2.100000000000000089 ) ) ;
#60088 = CARTESIAN_POINT ( 'NONE',  ( 7.827691340095081607, 20.28360254610759839, -1.500000000000002220 ) ) ;
#60089 = CARTESIAN_POINT ( 'NONE',  ( 19.75748517575715368, 0.3587747205144265483, 28.87153971905864580 ) ) ;
#60091 = ORIENTED_EDGE ( 'NONE', *, *, #72494, .F. ) ;
#60090 = CARTESIAN_POINT ( 'NONE',  ( 9.404896790668452411, 20.21284700076377305, 11.49999999999999645 ) ) ;
#60092 = DIRECTION ( 'NONE',  ( -3.773278334453080206E-23, 0.9999999999976377785, 2.173523156925979975E-06 ) ) ;
#60093 = FACE_OUTER_BOUND ( 'NONE', #48693, .T. ) ;
#60095 = DIRECTION ( 'NONE',  ( -0.000000000000000000, -1.000000000000000000, 0.000000000000000000 ) ) ;
#60094 = B_SPLINE_CURVE_WITH_KNOTS ( 'NONE', 3,
 ( #91218, #75983, #52168, #6492, #20701, #52667 ),
 .UNSPECIFIED., .F., .F.,
 ( 4, 2, 4 ),
 ( 0.000000000000000000, 0.001380764517853253371, 0.002761529035706506742 ),
 .UNSPECIFIED. ) ;
#60096 = ORIENTED_EDGE ( 'NONE', *, *, #91518, .F. ) ;
#60097 = EDGE_CURVE ( 'NONE', #90882, #41242, #7790, .T. ) ;
#60098 = ADVANCED_FACE ( 'NONE', ( #73773 ), #56189, .T. ) ;
#60099 = VERTEX_POINT ( 'NONE', #50950 ) ;
#60100 = B_SPLINE_CURVE_WITH_KNOTS ( 'NONE', 3,
 ( #75560, #60866, #59868, #76067 ),
 .UNSPECIFIED., .F., .F.,
 ( 4, 4 ),
 ( 0.8911363386465329661, 0.9001427699186484999 ),
 .UNSPECIFIED. ) ;
#60101 = ORIENTED_EDGE ( 'NONE', *, *, #4660, .T. ) ;
#60102 = EDGE_CURVE ( 'NONE', #89509, #43699, #79134, .T. ) ;
#60103 = CARTESIAN_POINT ( 'NONE',  ( -41.52287095715006870, -23.47596703998600631, 11.44779298504229281 ) ) ;
#60104 = CARTESIAN_POINT ( 'NONE',  ( -69.62287095715005592, -24.64965695001468404, 8.947790433994184056 ) ) ;
#60105 = CARTESIAN_POINT ( 'NONE',  ( 29.75292639967170771, -5.303223407918566501, 26.69524796275325684 ) ) ;
#60106 = CARTESIAN_POINT ( 'NONE',  ( -63.62287095715004881, -24.65952944569303895, 1.056160979905696129 ) ) ;
#60107 = CARTESIAN_POINT ( 'NONE',  ( -8.550378450311910683, 17.38971893761031851, 11.49999999999998934 ) ) ;
#60108 = CARTESIAN_POINT ( 'NONE',  ( -31.52287095715006870, -24.51387760970724372, 9.387446482453428942 ) ) ;
#60109 = VERTEX_POINT ( 'NONE', #51942 ) ;
#60110 = CARTESIAN_POINT ( 'NONE',  ( -16.98888496755095545, 9.415225082695979353, 11.49999999999999645 ) ) ;
#60111 = CARTESIAN_POINT ( 'NONE',  ( -130.5728709571500588, -23.56000036390796737, 11.50200000000000244 ) ) ;
#60112 = EDGE_CURVE ( 'NONE', #93818, #21767, #69437, .T. ) ;
#60113 = ORIENTED_EDGE ( 'NONE', *, *, #98310, .T. ) ;
#60114 = CARTESIAN_POINT ( 'NONE',  ( 3.450324536843889067, -6.376774720514404748, 18.60429515659643229 ) ) ;
#60115 = CARTESIAN_POINT ( 'NONE',  ( 3.183477995988301945, -5.876774720514405637, 18.35601591497023577 ) ) ;
#60116 = CARTESIAN_POINT ( 'NONE',  ( -102.6228709571500559, -24.65952944569304606, 1.056160979905702124 ) ) ;
#60117 = CARTESIAN_POINT ( 'NONE',  ( -64.52287095715006160, -29.50250243563736774, 8.947779886222145151 ) ) ;
#60118 = CARTESIAN_POINT ( 'NONE',  ( 16.84789977498956404, 10.09486508543780481, -1.500000000000002220 ) ) ;
#60119 = CARTESIAN_POINT ( 'NONE',  ( -46.57704074403396532, -24.65952944569304606, 1.056160979905696351 ) ) ;
#60120 = EDGE_LOOP ( 'NONE', ( #93247, #32324, #7152, #10270 ) ) ;
#60121 = CARTESIAN_POINT ( 'NONE',  ( 4.073501596442082651, -21.17334570714589859, -1.500000000000002220 ) ) ;
#60122 = CARTESIAN_POINT ( 'NONE',  ( -33.66794373389784312, -23.48786465467240347, 11.44779295918255535 ) ) ;
#60123 = DIRECTION ( 'NONE',  ( -3.773278334453080206E-23, 0.9999999999976377785, 2.173523156925979975E-06 ) ) ;
#60124 = CARTESIAN_POINT ( 'NONE',  ( -62.58953762381672448, -24.64965694238406968, 8.947790433994660120 ) ) ;
#60125 = VECTOR ( 'NONE', #22510, 1000.000000000000000 ) ;
#60126 = CARTESIAN_POINT ( 'NONE',  ( -99.54260921963015107, -25.18439459044040873, 3.861216775032092929 ) ) ;
#60127 = CARTESIAN_POINT ( 'NONE',  ( -9.967090755842360039, -20.75144515299163217, -1.500000000000002220 ) ) ;
#60128 = EDGE_CURVE ( 'NONE', #45825, #86005, #28105, .T. ) ;
#60129 = ADVANCED_FACE ( 'NONE', ( #20971 ), #51444, .T. ) ;
#60130 = DATE_AND_TIME ( #44899, #94308 ) ;
#60131 = DIRECTION ( 'NONE',  ( -0.000000000000000000, -1.000000000000000000, -0.000000000000000000 ) ) ;
#60132 = CARTESIAN_POINT ( 'NONE',  ( -51.30795378556842223, -25.25249061358302782, 3.767456410489268936 ) ) ;
#60133 = CARTESIAN_POINT ( 'NONE',  ( 19.96388892861992659, -2.714421270036905032, 11.49999999999999645 ) ) ;
#60134 = CARTESIAN_POINT ( 'NONE',  ( -13.36367879947601445, -5.876774720514426953, 20.00000000000000355 ) ) ;
#60135 = PLANE ( 'NONE',  #25761 ) ;
#60136 = B_SPLINE_CURVE_WITH_KNOTS ( 'NONE', 3,
 ( #86382, #38698, #69663, #54438, #16865, #93478 ),
 .UNSPECIFIED., .F., .F.,
 ( 4, 2, 4 ),
 ( 6.384118678612497773E-06, 0.001386860460828374768, 0.002767336802978137122 ),
 .UNSPECIFIED. ) ;
#60137 = CARTESIAN_POINT ( 'NONE',  ( -4.243469080022288509, -5.876774720514412742, 19.94806476610987644 ) ) ;
#60138 = DIRECTION ( 'NONE',  ( -3.773278334453079618E-23, 0.9999999999976377785, 2.173523156925979552E-06 ) ) ;
#60139 = CARTESIAN_POINT ( 'NONE',  ( -38.55620429048340014, -24.64898659630527789, 1.056161002820819039 ) ) ;
#60140 = CARTESIAN_POINT ( 'NONE',  ( 15.68239283413728735, 12.23493734220040530, -1.500000000000002220 ) ) ;
#60141 = ADVANCED_FACE ( 'NONE', ( #97605 ), #36711, .T. ) ;
#60142 = DIRECTION ( 'NONE',  ( -0.6392559695863496705, 6.845827386180411947E-16, -0.7689940216596069522 ) ) ;
#60143 = CARTESIAN_POINT ( 'NONE',  ( 15.11087362536062173, -12.71848776332401521, -1.500000000000002220 ) ) ;
#60144 = CARTESIAN_POINT ( 'NONE',  ( -126.5566010655604146, -23.48786465467241769, 11.44779295918253759 ) ) ;
#60145 = EDGE_CURVE ( 'NONE', #10246, #50276, #42843, .T. ) ;
#60146 = AXIS2_PLACEMENT_3D ( 'NONE', #64762, #3839, #50018 ) ;
#60147 = UNCERTAINTY_MEASURE_WITH_UNIT (LENGTH_MEASURE( 1.000000000000000082E-05 ), #1366, 'distance_accuracy_value', 'NONE');
#60148 = CARTESIAN_POINT ( 'NONE',  ( -72.62287095715005592, -23.47596703998600631, 11.44779298504227860 ) ) ;
#60149 = CARTESIAN_POINT ( 'NONE',  ( -37.52287095715006870, -29.50250243563736774, 8.947779886222148704 ) ) ;
#60150 = CARTESIAN_POINT ( 'NONE',  ( -10.41657757243416604, 17.86655067824183618, 11.49999999999999645 ) ) ;
#60151 = PLANE ( 'NONE',  #45107 ) ;
#60152 = CARTESIAN_POINT ( 'NONE',  ( 31.31121903262429029, 5.174141622015902442, 0.9154248472334550746 ) ) ;
#60153 = CARTESIAN_POINT ( 'NONE',  ( -79.55620429048339304, -23.47596703998600276, 11.44779298504227683 ) ) ;
#60154 = CARTESIAN_POINT ( 'NONE',  ( -7.854035805165779927, 21.33931789143995417, 11.49999999999999645 ) ) ;
#60155 = ORIENTED_EDGE ( 'NONE', *, *, #79480, .T. ) ;
#60156 = DIRECTION ( 'NONE',  ( -3.773278334453079618E-23, 0.9999999999976377785, 2.173523156925979975E-06 ) ) ;
#60157 = CARTESIAN_POINT ( 'NONE',  ( 29.70220533163293908, 3.584876737299458771, 28.20564067568759015 ) ) ;
#60158 = CARTESIAN_POINT ( 'NONE',  ( -8.513533612778267923, 18.29693335657625042, 11.49999999999998934 ) ) ;
#60159 = CARTESIAN_POINT ( 'NONE',  ( 8.271845302688321411, -0.3854532800250839442, -3.722136940144805450 ) ) ;
#60160 = FACE_OUTER_BOUND ( 'NONE', #62150, .T. ) ;
#60161 = VERTEX_POINT ( 'NONE', #29587 ) ;
#60162 = VERTEX_POINT ( 'NONE', #11872 ) ;
#60163 = EDGE_CURVE ( 'NONE', #92445, #71754, #86942, .T. ) ;
#60164 = CARTESIAN_POINT ( 'NONE',  ( 15.00000000000000533, 0.000000000000000000, 0.000000000000000000 ) ) ;
#60165 = CARTESIAN_POINT ( 'NONE',  ( 0.7049041324096299022, -22.85584899170066109, 11.49999999999998934 ) ) ;
#60166 = DIRECTION ( 'NONE',  ( 0.000000000000000000, 0.000000000000000000, -1.000000000000000000 ) ) ;
#60167 = CARTESIAN_POINT ( 'NONE',  ( -19.30636564405121902, 9.640216152154000184, -1.500000000000002220 ) ) ;
#60168 = CARTESIAN_POINT ( 'NONE',  ( -123.5570537027430333, -23.48783264082477373, -1.443836473390086361 ) ) ;
#60169 = LINE ( 'NONE', #21076, #100284 ) ;
#60170 = CARTESIAN_POINT ( 'NONE',  ( 3.584315319034878211, 22.25550262085195286, 11.49999999999999645 ) ) ;
#60171 = VERTEX_POINT ( 'NONE', #19981 ) ;
#60172 = CARTESIAN_POINT ( 'NONE',  ( -29.16972745157253399, -25.14850294581162515, 3.778578365308990161 ) ) ;
#60173 = CARTESIAN_POINT ( 'NONE',  ( 16.16784302627978320, -14.93143893958281154, 11.49999999999998934 ) ) ;
#60174 = FACE_BOUND ( 'NONE', #54082, .T. ) ;
#60175 = CARTESIAN_POINT ( 'NONE',  ( -41.46538131673724337, -25.10925854964650128, 3.231378914883284992 ) ) ;
#60177 = ORIENTED_EDGE ( 'NONE', *, *, #27462, .T. ) ;
#60176 = ADVANCED_FACE ( 'NONE', ( #83371 ), #35721, .T. ) ;
#60178 = CARTESIAN_POINT ( 'NONE',  ( -118.6228709571500559, -24.66019654487200086, 8.947790411086117501 ) ) ;
#60179 = CARTESIAN_POINT ( 'NONE',  ( -90.56379504561553517, -23.48786465467241769, 11.44779295918255180 ) ) ;
#60180 = ORIENTED_EDGE ( 'NONE', *, *, #56785, .T. ) ;
#60181 = DIRECTION ( 'NONE',  ( 0.000000000000000000, 0.000000000000000000, -1.000000000000000000 ) ) ;
#60182 = ORIENTED_EDGE ( 'NONE', *, *, #21671, .T. ) ;
#60183 = ORIENTED_EDGE ( 'NONE', *, *, #84339, .T. ) ;
#60184 = LINE ( 'NONE', #50559, #69609 ) ;
#60185 = DIRECTION ( 'NONE',  ( -1.000000000000000000, 0.000000000000000000, 0.000000000000000000 ) ) ;
#60186 = CARTESIAN_POINT ( 'NONE',  ( -57.64347623875748639, -23.96119346886880663, -0.6495511937832122440 ) ) ;
#60187 = CARTESIAN_POINT ( 'NONE',  ( -2.125485521908593078, 20.27274140177646444, -1.500000000000002220 ) ) ;
#60188 = ORIENTED_EDGE ( 'NONE', *, *, #16004, .T. ) ;
#60189 = CARTESIAN_POINT ( 'NONE',  ( -2.285970405126252825, -6.376774720514408301, 19.14905311829361167 ) ) ;
#60190 = CARTESIAN_POINT ( 'NONE',  ( -115.6228709571500559, -23.47596703998600631, 11.44779298504227860 ) ) ;
#60191 = DIRECTION ( 'NONE',  ( 0.000000000000000000, 2.173523156925980399E-06, -0.9999999999976378895 ) ) ;
#60192 = CARTESIAN_POINT ( 'NONE',  ( -51.55620429048339304, -24.64965694238574656, 8.947790433994207149 ) ) ;
#60193 = EDGE_LOOP ( 'NONE', ( #23576, #84795, #44722, #32332 ) ) ;
#60194 = CARTESIAN_POINT ( 'NONE',  ( 30.53060340732036337, -2.682774720514426559, 3.744237563515920634E-15 ) ) ;
#60195 = DIRECTION ( 'NONE',  ( 0.000000000000000000, -0.9999999999976377785, -2.173523156925979128E-06 ) ) ;
#60196 = CARTESIAN_POINT ( 'NONE',  ( 19.16185898538474675, 8.078635803559651052, 11.49999999999998934 ) ) ;
#60197 = AXIS2_PLACEMENT_3D ( 'NONE', #51019, #66262, #88082 ) ;
#60198 = ORIENTED_EDGE ( 'NONE', *, *, #47736, .T. ) ;
#60200 = EDGE_LOOP ( 'NONE', ( #72524, #88370 ) ) ;
#60199 = DIRECTION ( 'NONE',  ( -1.000000000000000000, -3.773278334444166432E-23, -8.201307841325785021E-29 ) ) ;
#60201 = ADVANCED_FACE ( 'NONE', ( #4273 ), #35222, .F. ) ;
#60202 = CARTESIAN_POINT ( 'NONE',  ( 14.43441819135929194, 3.316774720514426456, -28.36222020317710957 ) ) ;
#60203 = ORIENTED_EDGE ( 'NONE', *, *, #37889, .F. ) ;
#60204 = ORIENTED_EDGE ( 'NONE', *, *, #8404, .F. ) ;
#60205 = DIRECTION ( 'NONE',  ( -1.000000000000000000, -0.000000000000000000, -0.000000000000000000 ) ) ;
#60206 = CARTESIAN_POINT ( 'NONE',  ( 6.650000000000004796, 0.000000000000000000, 19.30000000000000071 ) ) ;
#60207 = CARTESIAN_POINT ( 'NONE',  ( -55.62287095715004881, -23.48783264082478084, -1.443836473390068820 ) ) ;
#60208 = DIRECTION ( 'NONE',  ( 0.000000000000000000, -0.3081562241202474572, -0.9513357669802769978 ) ) ;
#60210 = ORIENTED_EDGE ( 'NONE', *, *, #40044, .T. ) ;
#60209 = CARTESIAN_POINT ( 'NONE',  ( -10.67647856527443473, 19.39090429279614369, 11.49999999999999645 ) ) ;
#60211 = DIRECTION ( 'NONE',  ( 0.000000000000000000, 0.9999999999976377785, 2.173523156925979128E-06 ) ) ;
#60212 = CARTESIAN_POINT ( 'NONE',  ( 17.19246737676917292, 14.74310579602587090, 11.49999999999998934 ) ) ;
#60213 = EDGE_CURVE ( 'NONE', #91720, #29240, #83987, .T. ) ;
#60214 = EDGE_CURVE ( 'NONE', #82905, #41074, #37985, .T. ) ;
#60215 = EDGE_CURVE ( 'NONE', #52789, #28486, #23968, .T. ) ;
#60217 = ORIENTED_EDGE ( 'NONE', *, *, #56229, .T. ) ;
#60216 = CARTESIAN_POINT ( 'NONE',  ( -115.6239650023384797, -24.92592662359561473, 8.075495903017996469 ) ) ;
#60218 = VECTOR ( 'NONE', #66627, 1000.000000000000114 ) ;
#60219 = B_SPLINE_CURVE_WITH_KNOTS ( 'NONE', 3,
 ( #4638, #43206, #65564, #74146, #65065, #10750, #89369, #4140 ),
 .UNSPECIFIED., .F., .F.,
 ( 4, 2, 2, 4 ),
 ( -0.001240355328176664289, -0.0002398155169398015051, 0.0007607242942970612789, 0.002761803916770779257 ),
 .UNSPECIFIED. ) ;
#60220 = ORIENTED_EDGE ( 'NONE', *, *, #41109, .F. ) ;
#60222 = ADVANCED_FACE ( 'NONE', ( #85880 ), #30587, .T. ) ;
#60221 = SECURITY_CLASSIFICATION ( '', '', #40396 ) ;
#60223 = CARTESIAN_POINT ( 'NONE',  ( -10.22992732494356005, -5.749436596009021017, 29.32115093811272288 ) ) ;
#60224 = CARTESIAN_POINT ( 'NONE',  ( -19.30929855918770954, 5.666966705251045511, -1.500000000000002220 ) ) ;
#60225 = DIRECTION ( 'NONE',  ( -0.000000000000000000, 1.000000000000000000, -0.000000000000000000 ) ) ;
#60226 = ORIENTED_EDGE ( 'NONE', *, *, #48770, .F. ) ;
#60227 = FACE_OUTER_BOUND ( 'NONE', #16241, .T. ) ;
#60228 = CARTESIAN_POINT ( 'NONE',  ( -15.13915969582853549, -16.40262476207453801, -1.500000000000002220 ) ) ;
#60229 = EDGE_CURVE ( 'NONE', #44309, #32299, #61056, .T. ) ;
#60230 = EDGE_CURVE ( 'NONE', #36357, #56116, #74289, .T. ) ;
#60231 = ORIENTED_EDGE ( 'NONE', *, *, #38542, .T. ) ;
#60232 = ORIENTED_EDGE ( 'NONE', *, *, #10765, .F. ) ;
#60233 = DIRECTION ( 'NONE',  ( -3.773278334453079030E-23, 0.9999999999976377785, 2.173523156925979128E-06 ) ) ;
#60234 = DIRECTION ( 'NONE',  ( 3.773278334444167608E-23, -1.000000000000000000, 0.000000000000000000 ) ) ;
#60235 = DIRECTION ( 'NONE',  ( 0.000000000000000000, 0.000000000000000000, 1.000000000000000000 ) ) ;
#60236 = PLANE ( 'NONE',  #78931 ) ;
#60237 = CARTESIAN_POINT ( 'NONE',  ( -73.62287095715007013, -24.66019654487199020, 8.947790411086131712 ) ) ;
#60238 = CARTESIAN_POINT ( 'NONE',  ( 15.80261042061247068, 11.49252619723154112, -1.500000000000002220 ) ) ;
#60239 = DIRECTION ( 'NONE',  ( -3.773278334453079618E-23, 0.9999999999976377785, 2.173523156925979975E-06 ) ) ;
#60240 = CARTESIAN_POINT ( 'NONE',  ( 10.45947017991876926, -18.73710855793504848, -1.500000000000002220 ) ) ;
#60241 = CARTESIAN_POINT ( 'NONE',  ( -25.97212670940007584, -24.57999732512023883, 2.712287346642571428 ) ) ;
#60242 = CARTESIAN_POINT ( 'NONE',  ( -120.5228709571501184, -23.48783264082477373, -1.443836473390081698 ) ) ;
#60243 = PLANE ( 'NONE',  #76551 ) ;
#60244 = CARTESIAN_POINT ( 'NONE',  ( -15.20078144808659992, 16.97451310947862169, -1.500000000000002220 ) ) ;
#60245 = EDGE_CURVE ( 'NONE', #7198, #8989, #52943, .T. ) ;
#60246 = VECTOR ( 'NONE', #79410, 1000.000000000000114 ) ;
#60247 = DATE_TIME_ROLE ( 'creation_date' ) ;
#60248 = CARTESIAN_POINT ( 'NONE',  ( 22.02124265030973760, -6.143225279485574397, 16.20402280011862217 ) ) ;
#60249 = CARTESIAN_POINT ( 'NONE',  ( -33.52287095715007581, -23.48783264083359512, -1.443836473376374441 ) ) ;
#60250 = CARTESIAN_POINT ( 'NONE',  ( -11.44242300287478820, -16.35863574123370512, 11.49999999999999645 ) ) ;
#60251 = DIRECTION ( 'NONE',  ( -0.000000000000000000, -1.000000000000000000, -0.000000000000000000 ) ) ;
#60252 = CARTESIAN_POINT ( 'NONE',  ( -74.59647172187636954, -23.96169478059713498, 10.65365249895717881 ) ) ;
#60253 = DIRECTION ( 'NONE',  ( 3.773278334444167608E-23, -1.000000000000000000, 0.000000000000000000 ) ) ;
#60254 = VERTEX_POINT ( 'NONE', #91986 ) ;
#60255 = PLANE ( 'NONE',  #86632 ) ;
#60256 = CARTESIAN_POINT ( 'NONE',  ( -124.5228709571501042, -24.51283580621365132, 0.6167428607019898035 ) ) ;
#60257 = EDGE_CURVE ( 'NONE', #66619, #79051, #92422, .T. ) ;
#60258 = CARTESIAN_POINT ( 'NONE',  ( -11.39883337241029793, 18.50525654427185884, -1.500000000000002220 ) ) ;
#60259 = DIRECTION ( 'NONE',  ( -3.773278334453079030E-23, 0.9999999999976377785, 2.173523156925979128E-06 ) ) ;
#60260 = CARTESIAN_POINT ( 'NONE',  ( -0.9579564967699066846, 19.55851204243107233, -1.500000000000002220 ) ) ;
#60261 = DIRECTION ( 'NONE',  ( -3.773278334453079030E-23, 0.9999999999976377785, 2.173523156925979128E-06 ) ) ;
#60262 = ADVANCED_FACE ( 'NONE', ( #47325 ), #76252, .F. ) ;
#60263 = ADVANCED_FACE ( 'NONE', ( #62052 ), #1149, .F. ) ;
#60264 = ORIENTED_EDGE ( 'NONE', *, *, #44669, .T. ) ;
#60265 = APPROVAL_STATUS ( 'not_yet_approved' ) ;
#60266 = CARTESIAN_POINT ( 'NONE',  ( 5.184553252003285984, -5.965225279485572685, -28.06387035751381731 ) ) ;
#60267 = CARTESIAN_POINT ( 'NONE',  ( 3.398286024651508530, -5.876774720514429617, 21.76255057507181334 ) ) ;
#60268 = CARTESIAN_POINT ( 'NONE',  ( 16.11427877760282001, 12.65940972936023812, 11.49999999999999645 ) ) ;
#60269 = CARTESIAN_POINT ( 'NONE',  ( -39.42646868310482944, -25.31266292137979690, 5.336263692767317934 ) ) ;
#60270 = VECTOR ( 'NONE', #70977, 1000.000000000000114 ) ;
#60271 = CARTESIAN_POINT ( 'NONE',  ( -5.891025641025639636, -6.376774720514420736, 20.75510817307693046 ) ) ;
#60272 = ORIENTED_EDGE ( 'NONE', *, *, #35260, .F. ) ;
#60273 = CARTESIAN_POINT ( 'NONE',  ( -72.52287095715007581, -24.65952944569304606, 1.056160979905697239 ) ) ;
#60274 = CARTESIAN_POINT ( 'NONE',  ( -40.16027052433451416, -25.18430879010554690, 3.329283022737130171 ) ) ;
#60275 = CARTESIAN_POINT ( 'NONE',  ( 20.13489193910630703, 2.682774720514426559, -22.92085183005112370 ) ) ;
#60276 = CARTESIAN_POINT ( 'NONE',  ( -61.59189125704995860, -29.50249900881161835, 7.371157290072014590 ) ) ;
#60277 = ORIENTED_EDGE ( 'NONE', *, *, #34567, .T. ) ;
#60278 = CARTESIAN_POINT ( 'NONE',  ( 32.15269211224249091, 6.376774720514427841, 3.401810532325274750 ) ) ;
#60279 = B_SPLINE_CURVE_WITH_KNOTS ( 'NONE', 3,
 ( #62253, #61759, #85071, #23664 ),
 .UNSPECIFIED., .F., .F.,
 ( 4, 4 ),
 ( 0.000000000000000000, 0.0001000000000000167422 ),
 .UNSPECIFIED. ) ;
#60280 = VECTOR ( 'NONE', #45040, 1000.000000000000000 ) ;
#60281 = CARTESIAN_POINT ( 'NONE',  ( -17.29220519630379016, 15.29500218549028645, 11.49999999999999645 ) ) ;
#60282 = CARTESIAN_POINT ( 'NONE',  ( -22.70586268970451371, -1.818501321912391999, -1.500000000000002220 ) ) ;
#60283 = CARTESIAN_POINT ( 'NONE',  ( -70.32380231474228083, -25.12298712672050982, 7.101635559041870494 ) ) ;
#60284 = CARTESIAN_POINT ( 'NONE',  ( -67.52287095715009002, -24.34917612406836440, 0.1852690917426552120 ) ) ;
#60285 = DIRECTION ( 'NONE',  ( 0.000000000000000000, 0.000000000000000000, 1.000000000000000000 ) ) ;
#60286 = LOCAL_TIME ( 0, 54, 15.00000000000000000, #81462 ) ;
#60287 = DIRECTION ( 'NONE',  ( -0.000000000000000000, 0.000000000000000000, -1.000000000000000000 ) ) ;
#60288 = CARTESIAN_POINT ( 'NONE',  ( -110.5116840983523900, -24.83618233451450763, 1.606449574219537935 ) ) ;
#60289 = CARTESIAN_POINT ( 'NONE',  ( 13.84421170697429737, -16.98027460053469895, 11.49999999999998934 ) ) ;
#60290 = DIRECTION ( 'NONE',  ( 0.000000000000000000, -2.173523156925980399E-06, 0.9999999999976378895 ) ) ;
#60291 = CARTESIAN_POINT ( 'NONE',  ( -87.51095070751176763, -24.15620529776628445, 10.23563542870660292 ) ) ;
#60292 = CARTESIAN_POINT ( 'NONE',  ( -41.31493931824280708, -25.31165118850823603, 4.672661947695956108 ) ) ;
#60293 = CARTESIAN_POINT ( 'NONE',  ( -78.58482598963436772, -24.51314013834315375, 0.6176544820404143987 ) ) ;
#60294 = CARTESIAN_POINT ( 'NONE',  ( -117.6228709571500559, -24.33832256526968862, 0.1851278514119943652 ) ) ;
#60295 = CARTESIAN_POINT ( 'NONE',  ( -48.62287095715004881, -29.50248528299804818, 1.056150453629033370 ) ) ;
#60296 = ORIENTED_EDGE ( 'NONE', *, *, #20454, .F. ) ;
#60297 = CARTESIAN_POINT ( 'NONE',  ( 17.75789855128238770, 10.12834119215567164, -1.500000000000002220 ) ) ;
#60298 = ORIENTED_EDGE ( 'NONE', *, *, #39092, .F. ) ;
#60299 = ORIENTED_EDGE ( 'NONE', *, *, #73734, .T. ) ;
#60300 = ORIENTED_EDGE ( 'NONE', *, *, #91912, .F. ) ;
#60301 = ORIENTED_EDGE ( 'NONE', *, *, #31662, .T. ) ;
#60302 = CARTESIAN_POINT ( 'NONE',  ( -22.27228905017084060, 5.866681652885556986, -1.500000000000002220 ) ) ;
#60303 = CARTESIAN_POINT ( 'NONE',  ( -35.52287095715008292, -24.15431212366874547, -0.2830839119320505692 ) ) ;
#60304 = CARTESIAN_POINT ( 'NONE',  ( -19.33604739795523741, 5.927148246271303655, -1.500000000000002220 ) ) ;
#60305 = ORIENTED_EDGE ( 'NONE', *, *, #84462, .F. ) ;
#60306 = CARTESIAN_POINT ( 'NONE',  ( -27.15357404441686384, -24.72305439599990251, 2.243760839632586546 ) ) ;
#60307 = CARTESIAN_POINT ( 'NONE',  ( -101.5228709571500758, -23.47596703998600631, 11.44779298504228215 ) ) ;
#60308 = CARTESIAN_POINT ( 'NONE',  ( -64.62287095715005592, -24.66019654487198665, 8.947790411086131712 ) ) ;
#60309 = DIRECTION ( 'NONE',  ( -3.773278334453079030E-23, 0.9999999999976377785, 2.173523156925979128E-06 ) ) ;
#60311 = ORIENTED_EDGE ( 'NONE', *, *, #54743, .F. ) ;
#60310 = CARTESIAN_POINT ( 'NONE',  ( 20.36625868517733196, 6.724766957447481097, 11.49999999999999645 ) ) ;
#60312 = PLANE ( 'NONE',  #51659 ) ;
#60313 = CARTESIAN_POINT ( 'NONE',  ( -74.52287095715007581, -24.65952944569304606, 1.056160979905697239 ) ) ;
#60314 = ORIENTED_EDGE ( 'NONE', *, *, #9563, .F. ) ;
#60315 = CARTESIAN_POINT ( 'NONE',  ( -16.63904852704994042, -12.34428335884295969, -1.500000000000002220 ) ) ;
#60317 = VERTEX_POINT ( 'NONE', #22457 ) ;
#60316 = DIRECTION ( 'NONE',  ( -0.000000000000000000, -1.000000000000000000, -0.000000000000000000 ) ) ;
#60318 = AXIS2_PLACEMENT_3D ( 'NONE', #16140, #62848, #24749 ) ;
#60319 = EDGE_CURVE ( 'NONE', #96596, #12582, #14775, .T. ) ;
#60320 = B_SPLINE_SURFACE_WITH_KNOTS ( 'NONE', 3, 3, ( 
 ( #99008, #37126, #52856, #68085 ),
 ( #92402, #62473, #53364, #31009 ),
 ( #38117, #61976, #69073, #93400 ),
 ( #22874, #30004, #99998, #83794 ),
 ( #45248, #30507, #39120, #84794 ),
 ( #15277, #22378, #68581, #60976 ),
 ( #46239, #92902, #84290, #77170 ) ),
 .UNSPECIFIED., .F., .F., .F.,
 ( 4, 3, 4 ),
 ( 4, 4 ),
 ( 0.3389563248807680451, 0.5103010155056330044, 0.6816457061304979081 ),
 ( 0.1860178884124073506, 0.2169648086611711268 ),
 .UNSPECIFIED. ) ;
#60321 = CARTESIAN_POINT ( 'NONE',  ( -28.56161963849136498, -23.57732030158533476, -1.055554491438110309 ) ) ;
#60322 = ORIENTED_EDGE ( 'NONE', *, *, #28443, .F. ) ;
#60323 = EDGE_CURVE ( 'NONE', #40447, #42731, #2765, .T. ) ;
#60324 = CARTESIAN_POINT ( 'NONE',  ( 4.821763668436347849, -6.376774720514406525, 18.93074869776452829 ) ) ;
#60325 = ORIENTED_EDGE ( 'NONE', *, *, #70748, .F. ) ;
#60326 = EDGE_CURVE ( 'NONE', #16463, #71288, #56452, .T. ) ;
#60327 = B_SPLINE_CURVE_WITH_KNOTS ( 'NONE', 3,
 ( #13128, #44097, #5523, #67943, #46602, #7524, #2811, #95646, #33748, #93760 ),
 .UNSPECIFIED., .F., .F.,
 ( 4, 2, 2, 2, 4 ),
 ( 0.000000000000000000, 0.2500000000000000000, 0.5000000000000000000, 0.7500000000000000000, 1.000000000000000000 ),
 .UNSPECIFIED. ) ;
#60328 = CARTESIAN_POINT ( 'NONE',  ( 12.56776941831905070, -16.83212535568997126, -1.500000000000002220 ) ) ;
#60329 = CARTESIAN_POINT ( 'NONE',  ( -19.44315311050126382, -10.23602577120861667, 11.49999999999999645 ) ) ;
#60330 = EDGE_CURVE ( 'NONE', #78100, #91151, #24972, .T. ) ;
#60331 = CARTESIAN_POINT ( 'NONE',  ( -73.51158995227403636, -23.96169478059713143, 10.65365249895718236 ) ) ;
#60332 = CARTESIAN_POINT ( 'NONE',  ( 20.50669422456317292, -9.396423750077818937, 11.49999999999998934 ) ) ;
#60333 = EDGE_CURVE ( 'NONE', #45368, #40450, #88553, .T. ) ;
#60334 = CARTESIAN_POINT ( 'NONE',  ( -20.97355972163249049, 0.1317905507124840780, -1.500000000000002220 ) ) ;
#60335 = CARTESIAN_POINT ( 'NONE',  ( -89.62287095715007013, -24.33832256527049864, 0.1851278514138624265 ) ) ;
#60336 = EDGE_CURVE ( 'NONE', #43450, #100181, #17871, .T. ) ;
#60337 = CARTESIAN_POINT ( 'NONE',  ( -89.40841769935767047, -25.26877885127129986, 5.947789088311301597 ) ) ;
#60338 = FACE_OUTER_BOUND ( 'NONE', #90457, .T. ) ;
#60339 = ORIENTED_EDGE ( 'NONE', *, *, #20821, .F. ) ;
#60340 = CIRCLE ( 'NONE', #86246, 1.000000000000000000 ) ;
#60341 = ORIENTED_EDGE ( 'NONE', *, *, #35638, .F. ) ;
#60342 = VERTEX_POINT ( 'NONE', #49842 ) ;
#60343 = AXIS2_PLACEMENT_3D ( 'NONE', #39147, #61998, #92926 ) ;
#60344 = CARTESIAN_POINT ( 'NONE',  ( -128.6228709571500701, -24.35013146730203815, 9.818937971375104823 ) ) ;
#60345 = CARTESIAN_POINT ( 'NONE',  ( 8.792760106793807040, 19.66521392739144858, -1.500000000000002220 ) ) ;
#60346 = CARTESIAN_POINT ( 'NONE',  ( 5.356969261897235768, 0.3587747205143965168, -28.55262118024313978 ) ) ;
#60347 = ORIENTED_EDGE ( 'NONE', *, *, #75307, .T. ) ;
#60348 = CARTESIAN_POINT ( 'NONE',  ( -19.14942259116913092, -8.910193081567555851, -1.500000000000002220 ) ) ;
#60349 = LINE ( 'NONE', #91275, #38494 ) ;
#60350 = PLANE ( 'NONE',  #21948 ) ;
#60351 = CARTESIAN_POINT ( 'NONE',  ( -83.55852081072703186, -23.73791477778911840, 11.05961554403170588 ) ) ;
#60352 = CARTESIAN_POINT ( 'NONE',  ( -79.52287095715006160, -23.48786465467241058, 11.44779295918254469 ) ) ;
#60353 = DIRECTION ( 'NONE',  ( 1.000000000000000000, -0.000000000000000000, -0.000000000000000000 ) ) ;
#60354 = CARTESIAN_POINT ( 'NONE',  ( 5.627179592841175193, 21.36305014179116668, -1.500000000000002220 ) ) ;
#60355 = DIRECTION ( 'NONE',  ( -3.773278334453079618E-23, 0.9999999999976377785, 2.173523156925979975E-06 ) ) ;
#60356 = EDGE_CURVE ( 'NONE', #60837, #83380, #48329, .T. ) ;
#60357 = ORIENTED_EDGE ( 'NONE', *, *, #55166, .T. ) ;
#60358 = CARTESIAN_POINT ( 'NONE',  ( -51.93149462243456327, -25.24860260566776660, 6.174051151396142245 ) ) ;
#60359 = CARTESIAN_POINT ( 'NONE',  ( -79.62287095715005592, -23.47593901973091235, -1.443836447539004642 ) ) ;
#60360 = CARTESIAN_POINT ( 'NONE',  ( -99.52287095715006160, -24.64965694238407323, 8.947790433994194714 ) ) ;
#60361 = PLANE ( 'NONE',  #90075 ) ;
#60362 = CIRCLE ( 'NONE', #19765, 2.000000000000000000 ) ;
#60363 = EDGE_CURVE ( 'NONE', #88746, #21831, #51312, .T. ) ;
#60364 = B_SPLINE_CURVE_WITH_KNOTS ( 'NONE', 3,
 ( #61397, #53780, #6090, #68004 ),
 .UNSPECIFIED., .F., .F.,
 ( 4, 4 ),
 ( 2.775557561562891043E-17, 9.999999999998898659E-05 ),
 .UNSPECIFIED. ) ;
#60365 = CARTESIAN_POINT ( 'NONE',  ( -4.672984603565591755, -18.88948546680484242, 11.49999999999998934 ) ) ;
#60366 = APPROVAL_PERSON_ORGANIZATION ( #64901, #75393, #12064 ) ;
#60367 = CARTESIAN_POINT ( 'NONE',  ( -10.59417575825165159, 18.57464501519095279, -1.500000000000002220 ) ) ;
#60368 = LINE ( 'NONE', #20764, #2876 ) ;
#60369 = B_SPLINE_CURVE_WITH_KNOTS ( 'NONE', 3,
 ( #60337, #14127, #47473, #78400 ),
 .UNSPECIFIED., .F., .F.,
 ( 4, 4 ),
 ( 0.000000000000000000, 0.0005192307692308412159 ),
 .UNSPECIFIED. ) ;
#60370 = LINE ( 'NONE', #59861, #23626 ) ;
#60371 = DIRECTION ( 'NONE',  ( 0.000000000000000000, -1.000000000000000000, 0.000000000000000000 ) ) ;
#60372 = DIRECTION ( 'NONE',  ( 0.000000000000000000, 0.000000000000000000, -1.000000000000000000 ) ) ;
#60373 = CARTESIAN_POINT ( 'NONE',  ( 4.697487806458584991, -22.17256498326293013, -1.500000000000002220 ) ) ;
#60374 = VERTEX_POINT ( 'NONE', #80775 ) ;
#60375 = DIRECTION ( 'NONE',  ( 0.000000000000000000, -1.000000000000000000, 0.000000000000000000 ) ) ;
#60376 = CARTESIAN_POINT ( 'NONE',  ( -102.5895376238167387, -24.64965694238575011, 8.947790433994194714 ) ) ;
#60377 = CARTESIAN_POINT ( 'NONE',  ( 12.93213199337649044, -14.99640713134888692, 11.49999999999999645 ) ) ;
#60378 = VECTOR ( 'NONE', #50454, 1000.000000000000000 ) ;
#60379 = CARTESIAN_POINT ( 'NONE',  ( -35.62287095715005592, -25.00158670708908915, 2.256160236439166855 ) ) ;
#60380 = ORIENTED_EDGE ( 'NONE', *, *, #3975, .T. ) ;
#60381 = CARTESIAN_POINT ( 'NONE',  ( -19.80875734969026425, 0.3587747205144265483, 31.02402280011862246 ) ) ;
#60382 = B_SPLINE_CURVE_WITH_KNOTS ( 'NONE', 3,
 ( #34169, #80332, #81336, #40770, #25547, #97054 ),
 .UNSPECIFIED., .F., .F.,
 ( 4, 2, 4 ),
 ( 0.000000000000000000, 0.001380764517854768652, 0.002761529035709537304 ),
 .UNSPECIFIED. ) ;
#60383 = DIRECTION ( 'NONE',  ( 0.000000000000000000, -0.9999999999976377785, -2.173523156925979975E-06 ) ) ;
#60384 = CARTESIAN_POINT ( 'NONE',  ( 20.55956107658784404, -6.795330137259728787, 11.49999999999998934 ) ) ;
#60385 = CARTESIAN_POINT ( 'NONE',  ( -49.59577668750772972, -25.27517929962447951, 3.074245939016678975 ) ) ;
#60386 = CARTESIAN_POINT ( 'NONE',  ( 19.37663158793545293, -0.8356294931911363300, -1.500000000000002220 ) ) ;
#60387 = CARTESIAN_POINT ( 'NONE',  ( -80.52287095715006160, -24.92604778743017846, 8.074972756849362554 ) ) ;
#60388 = DIRECTION ( 'NONE',  ( 1.000000000000000000, 1.387778780781445429E-16, 0.000000000000000000 ) ) ;
#60389 = EDGE_CURVE ( 'NONE', #5644, #87540, #71664, .T. ) ;
#60390 = CARTESIAN_POINT ( 'NONE',  ( -7.013475202606065828, -18.52788797337992222, -1.500000000000002220 ) ) ;
#60391 = VERTEX_POINT ( 'NONE', #16863 ) ;
#60392 = CARTESIAN_POINT ( 'NONE',  ( 3.729398819442638846, -20.01364129133569136, 11.49999999999999645 ) ) ;
#60393 = DIRECTION ( 'NONE',  ( 1.000000000000000000, -0.000000000000000000, -0.000000000000000000 ) ) ;
#60394 = EDGE_CURVE ( 'NONE', #90882, #67798, #24474, .T. ) ;
#60396 = CIRCLE ( 'NONE', #2085, 0.2499999999997798983 ) ;
#60395 = CARTESIAN_POINT ( 'NONE',  ( 33.61456970919608978, -3.316774720514426900, -11.35828564741660962 ) ) ;
#60397 = ORIENTED_EDGE ( 'NONE', *, *, #81178, .T. ) ;
#60398 = DIRECTION ( 'NONE',  ( 1.000000000000000000, 3.773278334444166432E-23, 8.201307841325785021E-29 ) ) ;
#60399 = CARTESIAN_POINT ( 'NONE',  ( -62.62287095715004881, -24.64898659630528854, 1.056161002820822592 ) ) ;
#60400 = PLANE ( 'NONE',  #36981 ) ;
#60401 = CARTESIAN_POINT ( 'NONE',  ( 27.53860345374808105, 5.356774720514427379, 1.647607965253217399 ) ) ;
#60402 = CARTESIAN_POINT ( 'NONE',  ( -51.27501529246699619, -25.17319112662202585, 6.792536120916223830 ) ) ;
#60403 = CARTESIAN_POINT ( 'NONE',  ( -16.72505113720834657, 11.10480813184383742, 11.49999999999998934 ) ) ;
#60404 = DIRECTION ( 'NONE',  ( 0.9890158633619159367, 0.1478094111296165969, 0.000000000000000000 ) ) ;
#60405 = ORIENTED_EDGE ( 'NONE', *, *, #58665, .T. ) ;
#60406 = CARTESIAN_POINT ( 'NONE',  ( -31.52287095715006160, -29.50247984919015209, -1.443849546365062242 ) ) ;
#60407 = CARTESIAN_POINT ( 'NONE',  ( -22.55118551311790753, 3.560990644294375063, 11.49999999999999645 ) ) ;
#60408 = CARTESIAN_POINT ( 'NONE',  ( -105.9228709571500531, -23.47593901973090524, -1.443836447538996870 ) ) ;
#60409 = VECTOR ( 'NONE', #38386, 1000.000000000000114 ) ;
#60410 = CARTESIAN_POINT ( 'NONE',  ( -115.6228709571500417, -23.48783264082478794, -1.443836473390058384 ) ) ;
#60411 = DIRECTION ( 'NONE',  ( -3.773278334444166432E-23, 1.000000000000000000, 0.000000000000000000 ) ) ;
#60412 = CARTESIAN_POINT ( 'NONE',  ( 5.811591729264017125, -5.876774720514422512, 21.22699980322195046 ) ) ;
#60413 = FACE_OUTER_BOUND ( 'NONE', #41117, .T. ) ;
#60414 = CARTESIAN_POINT ( 'NONE',  ( -37.62287095715005592, -24.66019654487199020, 8.947790411086135265 ) ) ;
#60415 = ORIENTED_EDGE ( 'NONE', *, *, #95490, .F. ) ;
#60416 = CARTESIAN_POINT ( 'NONE',  ( -19.47531982339030776, -5.969937916086089480, -1.500000000000002220 ) ) ;
#60417 = EDGE_LOOP ( 'NONE', ( #73416, #11734, #20820, #88154 ) ) ;
#60418 = CARTESIAN_POINT ( 'NONE',  ( 19.50756536182865020, -12.10693203178887423, 11.49999999999998934 ) ) ;
#60419 = CARTESIAN_POINT ( 'NONE',  ( -32.52611253423770421, -24.65952944569304606, 1.056160979905696351 ) ) ;
#60420 = ORIENTED_EDGE ( 'NONE', *, *, #5593, .T. ) ;
#60421 = CARTESIAN_POINT ( 'NONE',  ( -108.6261691894128063, -24.35071581493544102, 9.817618358456016381 ) ) ;
#60422 = CARTESIAN_POINT ( 'NONE',  ( -77.49792482936582871, -24.66019654487200441, 8.947790411086108620 ) ) ;
#60423 = AXIS2_PLACEMENT_3D ( 'NONE', #30012, #13285, #20899 ) ;
#60424 = CARTESIAN_POINT ( 'NONE',  ( -51.57778911984880210, -24.66019654487199730, 8.947790411086117501 ) ) ;
#60426 = ORIENTED_EDGE ( 'NONE', *, *, #81532, .F. ) ;
#60425 = CARTESIAN_POINT ( 'NONE',  ( -7.839647760473957838, 19.78794240023834661, 11.49999999999999645 ) ) ;
#60427 = LOCAL_TIME ( 0, 54, 15.00000000000000000, #79964 ) ;
#60428 = VERTEX_POINT ( 'NONE', #41217 ) ;
#60429 = CARTESIAN_POINT ( 'NONE',  ( 13.39142644571787422, -17.71860720625715757, 11.49999999999998934 ) ) ;
#60430 = CARTESIAN_POINT ( 'NONE',  ( -20.25002411749221665, -3.895867502427604379, 11.49999999999998934 ) ) ;
#60431 = ORIENTED_EDGE ( 'NONE', *, *, #49631, .T. ) ;
#60433 = ORIENTED_EDGE ( 'NONE', *, *, #76806, .F. ) ;
#60432 = VECTOR ( 'NONE', #82201, 1000.000000000000114 ) ;
#60434 = EDGE_CURVE ( 'NONE', #25965, #18516, #37794, .T. ) ;
#60435 = FACE_OUTER_BOUND ( 'NONE', #17767, .T. ) ;
#60436 = CARTESIAN_POINT ( 'NONE',  ( 2.677468215678941110, -5.876774720514418959, 20.83735685176740304 ) ) ;
#60437 = ORIENTED_EDGE ( 'NONE', *, *, #64947, .T. ) ;
#60438 = EDGE_CURVE ( 'NONE', #64588, #38183, #94766, .T. ) ;
#60439 = ORIENTED_EDGE ( 'NONE', *, *, #60526, .T. ) ;
#60440 = CIRCLE ( 'NONE', #42631, 21.89999999999999858 ) ;
#60441 = LINE ( 'NONE', #79139, #38245 ) ;
#60442 = CARTESIAN_POINT ( 'NONE',  ( -41.60044718131246100, -23.96169478059712432, 10.65365249895718591 ) ) ;
#60443 = CARTESIAN_POINT ( 'NONE',  ( -56.62287095715005592, -29.50247984919015209, -1.443849546365056913 ) ) ;
#60444 = CARTESIAN_POINT ( 'NONE',  ( -14.80784184970232431, -14.63167926507950689, -1.500000000000002220 ) ) ;
#60445 = CARTESIAN_POINT ( 'NONE',  ( 11.26692973276593968, -18.67385317477220497, 11.49999999999999645 ) ) ;
#60446 = EDGE_CURVE ( 'NONE', #38706, #80888, #47510, .T. ) ;
#60447 = CARTESIAN_POINT ( 'NONE',  ( -50.79320621498229826, -25.03929677109420027, 7.533075084478241479 ) ) ;
#60448 = CARTESIAN_POINT ( 'NONE',  ( -7.160000000000000142, 7.891155995661686795, 5.788828319098143993 ) ) ;
#60449 = CARTESIAN_POINT ( 'NONE',  ( 4.981011153104904388, 21.88276397462241363, 11.49999999999998934 ) ) ;
#60450 = EDGE_CURVE ( 'NONE', #77746, #53293, #41727, .T. ) ;
#60451 = CARTESIAN_POINT ( 'NONE',  ( -51.08807254026520184, -25.31296702852269576, 4.449946140181717524 ) ) ;
#60452 = ORIENTED_EDGE ( 'NONE', *, *, #38598, .F. ) ;
#60453 = CARTESIAN_POINT ( 'NONE',  ( 5.514125806255895004E-17, -29.50250786944496539, 11.44777975102276812 ) ) ;
#60454 = CARTESIAN_POINT ( 'NONE',  ( 8.499999999999989342, 18.74999999999999645, 2.100000000000000089 ) ) ;
#60455 = B_SPLINE_SURFACE_WITH_KNOTS ( 'NONE', 3, 1, ( 
 ( #11350, #80359 ),
 ( #27581, #5230 ),
 ( #10852, #36186 ),
 ( #97081, #73255 ),
 ( #72763, #42324 ),
 ( #26071, #57044 ),
 ( #50917, #87979 ) ),
 .UNSPECIFIED., .F., .F., .F.,
 ( 4, 1, 1, 1, 4 ),
 ( 2, 2 ),
 ( 0.000000000000000000, 0.1496899112665939224, 0.2993798225331877338, 0.4490697337997815453, 0.5987596450663754677 ),
 ( 0.000000000000000000, 1.000000000000000000 ),
 .UNSPECIFIED. ) ;
#60456 = EDGE_CURVE ( 'NONE', #91001, #100004, #39053, .T. ) ;
#60457 = VERTEX_POINT ( 'NONE', #74646 ) ;
#60458 = EDGE_CURVE ( 'NONE', #26531, #63950, #80504, .T. ) ;
#60459 = ORIENTED_EDGE ( 'NONE', *, *, #10898, .T. ) ;
#60460 = CARTESIAN_POINT ( 'NONE',  ( -95.52287095715006160, -29.50248528299804818, 1.056150453629042030 ) ) ;
#60461 = ORIENTED_EDGE ( 'NONE', *, *, #90920, .F. ) ;
#60462 = CARTESIAN_POINT ( 'NONE',  ( 13.34776491790984210, -16.67230741956907991, -1.500000000000002220 ) ) ;
#60463 = VERTEX_POINT ( 'NONE', #65575 ) ;
#60464 = CARTESIAN_POINT ( 'NONE',  ( -40.62287095715004170, -25.00182538069145011, 7.747789668545099317 ) ) ;
#60465 = CARTESIAN_POINT ( 'NONE',  ( -20.94189920129180038, 1.864940847883316488, -1.500000000000002220 ) ) ;
#60466 = DIRECTION ( 'NONE',  ( 0.000000000000000000, -2.173523156925979552E-06, 0.9999999999976378895 ) ) ;
#60467 = DIRECTION ( 'NONE',  ( -0.000000000000000000, -1.000000000000000000, -0.000000000000000000 ) ) ;
#60468 = LINE ( 'NONE', #29987, #57890 ) ;
#60469 = CARTESIAN_POINT ( 'NONE',  ( 4.863445656156933694, -21.36585520573490626, -1.500000000000002220 ) ) ;
#60470 = CARTESIAN_POINT ( 'NONE',  ( -39.52287095715005449, -24.51283580621365132, 0.6167428607019651565 ) ) ;
#60471 = ORIENTED_EDGE ( 'NONE', *, *, #54143, .T. ) ;
#60472 = CARTESIAN_POINT ( 'NONE',  ( -58.62287095715004881, -24.64965695001468404, 8.947790433994185832 ) ) ;
#60473 = AXIS2_PLACEMENT_3D ( 'NONE', #80275, #41733, #66080 ) ;
#60474 = CARTESIAN_POINT ( 'NONE',  ( -84.51364942372109113, -23.96169478059713498, 10.65365249895717881 ) ) ;
#60475 = B_SPLINE_CURVE_WITH_KNOTS ( 'NONE', 3,
 ( #68360, #5949, #13556, #36407, #59252, #83060, #83568, #67868, #5455, #28794, #98795, #76449, #91679, #29790, #52137, #74469, #52633, #21659 ),
 .UNSPECIFIED., .F., .F.,
 ( 4, 2, 2, 2, 2, 2, 2, 2, 4 ),
 ( 0.000000000000000000, 0.0001035810172459879051, 0.0002071620344919758102, 0.0004143240689839454405, 0.0008286481379678616076, 0.001035810172459820152, 0.001242972206951778588, 0.001450134241443737241, 0.001657296275935695676 ),
 .UNSPECIFIED. ) ;
#60476 = AXIS2_PLACEMENT_3D ( 'NONE', #79337, #24550, #40287 ) ;
#60477 = CARTESIAN_POINT ( 'NONE',  ( -130.5728709571500588, -24.37907397113050934, 9.703205396196688426 ) ) ;
#60478 = CARTESIAN_POINT ( 'NONE',  ( -0.008165308626489691315, -22.94429366319002028, 5.002395802403317049 ) ) ;
#60479 = CARTESIAN_POINT ( 'NONE',  ( 15.78869406909177897, -14.30566568001193950, 11.49999999999998934 ) ) ;
#60480 = CARTESIAN_POINT ( 'NONE',  ( -98.62355868264205583, -24.66019654487200086, 8.947790411086119278 ) ) ;
#60481 = CARTESIAN_POINT ( 'NONE',  ( -54.55620429048339304, -23.47593901973091235, -1.443836447539009749 ) ) ;
#60482 = CARTESIAN_POINT ( 'NONE',  ( 15.34241074214975065, -3.824162593742471028, -28.48848699765728654 ) ) ;
#60483 = CARTESIAN_POINT ( 'NONE',  ( 33.96422015159436114, 5.965225279485572685, -7.233236000911337449 ) ) ;
#60484 = CARTESIAN_POINT ( 'NONE',  ( -8.519796113377745783, 20.75715399588506926, -1.500000000000002220 ) ) ;
#60485 = CARTESIAN_POINT ( 'NONE',  ( 25.61870917940689196, 6.376774720514426953, 28.79814474876424768 ) ) ;
#60486 = EDGE_LOOP ( 'NONE', ( #21271, #23485, #47555, #40336 ) ) ;
#60487 = CARTESIAN_POINT ( 'NONE',  ( -72.52287095715010423, -23.48783264082476308, -1.443836473390092578 ) ) ;
#60488 = CARTESIAN_POINT ( 'NONE',  ( 3.881049643139886207, -19.21785841795820104, 11.49999999999999645 ) ) ;
#60489 = CARTESIAN_POINT ( 'NONE',  ( -108.5228709571500900, -24.33927499327855415, 9.819080762295804732 ) ) ;
#60490 = CARTESIAN_POINT ( 'NONE',  ( -76.58953762381673869, -24.64965694238407679, 8.947790433994653014 ) ) ;
#60491 = ORIENTED_EDGE ( 'NONE', *, *, #56157, .T. ) ;
#60492 = CARTESIAN_POINT ( 'NONE',  ( -88.54555701694573600, -24.51419770103157703, 9.386484678747176957 ) ) ;
#60493 = CARTESIAN_POINT ( 'NONE',  ( -31.62287095715005236, -29.50248528299804818, 1.056150453629029817 ) ) ;
#60494 = CARTESIAN_POINT ( 'NONE',  ( -91.96387813629002039, -25.32379766982192848, 4.367815445636563432 ) ) ;
#60495 = CARTESIAN_POINT ( 'NONE',  ( -108.6228709571500559, -29.50248528299804818, 1.056150453629043584 ) ) ;
#60496 = B_SPLINE_CURVE_WITH_KNOTS ( 'NONE', 3,
 ( #61238, #92158, #4073, #30765, #816, #7925 ),
 .UNSPECIFIED., .F., .F.,
 ( 4, 2, 4 ),
 ( 6.384118695054804036E-06, 0.001386860460836599309, 0.002767336802978144061 ),
 .UNSPECIFIED. ) ;
#60497 = VECTOR ( 'NONE', #33911, 1000.000000000000000 ) ;
#60498 = CARTESIAN_POINT ( 'NONE',  ( -19.67082186522023690, -1.387426831159568108, -1.500000000000002220 ) ) ;
#60499 = ORIENTED_EDGE ( 'NONE', *, *, #39596, .F. ) ;
#60500 = CARTESIAN_POINT ( 'NONE',  ( -120.6228709571500417, -29.50248789122583659, 2.256150453626215580 ) ) ;
#60501 = DIRECTION ( 'NONE',  ( 1.000000000000000000, 0.000000000000000000, 0.000000000000000000 ) ) ;
#60502 = ADVANCED_FACE ( 'NONE', ( #5141 ), #20693, .T. ) ;
#60503 = VECTOR ( 'NONE', #39272, 1000.000000000000000 ) ;
#60504 = DATE_AND_TIME ( #100014, #91124 ) ;
#60505 = EDGE_CURVE ( 'NONE', #62223, #57717, #19364, .T. ) ;
#60506 = VERTEX_POINT ( 'NONE', #81266 ) ;
#60507 = CARTESIAN_POINT ( 'NONE',  ( -56.52287095715006870, -23.48786465467241058, 11.44779295918254824 ) ) ;
#60508 = CARTESIAN_POINT ( 'NONE',  ( -67.62287095715005592, -24.65952944569304606, 1.056160979905697017 ) ) ;
#60509 = FACE_OUTER_BOUND ( 'NONE', #57349, .T. ) ;
#60510 = CARTESIAN_POINT ( 'NONE',  ( 22.02124265030973760, -6.143225279485574397, 19.55402280011862004 ) ) ;
#60511 = CARTESIAN_POINT ( 'NONE',  ( -121.5562042904833930, -24.65952944569305316, 1.056160979905706565 ) ) ;
#60512 = CARTESIAN_POINT ( 'NONE',  ( -31.24388727629348494, -24.86441894802673147, 8.247789967202360017 ) ) ;
#60513 = VECTOR ( 'NONE', #16784, 1000.000000000000000 ) ;
#60514 = CARTESIAN_POINT ( 'NONE',  ( -107.5967310269383574, -23.48783264082479505, -1.443836473390060826 ) ) ;
#60515 = CARTESIAN_POINT ( 'NONE',  ( -3.050325703546597822, 19.74810961616558913, -1.500000000000002220 ) ) ;
#60516 = CARTESIAN_POINT ( 'NONE',  ( 8.349999999999972999, 27.69999999999999574, 2.100000000000000089 ) ) ;
#60517 = DIRECTION ( 'NONE',  ( 3.773278334444167608E-23, -1.000000000000000000, 0.000000000000000000 ) ) ;
#60518 = ORIENTED_EDGE ( 'NONE', *, *, #13386, .T. ) ;
#60519 = CARTESIAN_POINT ( 'NONE',  ( -24.90875734969025501, 5.965225279485572685, 30.00402280011862288 ) ) ;
#60520 = CARTESIAN_POINT ( 'NONE',  ( -119.6241227149520228, -24.51314013834316086, 0.6176544820404245018 ) ) ;
#60521 = CARTESIAN_POINT ( 'NONE',  ( -80.50429440537433834, -24.40133493613049964, 9.663955038902802386 ) ) ;
#60522 = CARTESIAN_POINT ( 'NONE',  ( -81.52287095715010423, -23.48783264083388289, -1.443836473375922580 ) ) ;
#60523 = CARTESIAN_POINT ( 'NONE',  ( -39.49835484170713329, -24.15543982623906416, -0.2315651400026678131 ) ) ;
#60524 = CARTESIAN_POINT ( 'NONE',  ( -118.6228709571500559, -29.50250243563736774, 8.947779886222134493 ) ) ;
#60526 = EDGE_CURVE ( 'NONE', #16871, #28343, #13705, .T. ) ;
#60525 = CC_DESIGN_PERSON_AND_ORGANIZATION_ASSIGNMENT ( #84572, #69357, ( #2120 ) ) ;
#60527 = CARTESIAN_POINT ( 'NONE',  ( -1.845912073933368536, -6.376774720514408301, 19.53740760792477360 ) ) ;
#60528 = B_SPLINE_SURFACE_WITH_KNOTS ( 'NONE', 3, 1, ( 
 ( #37708, #92984 ),
 ( #83880, #45337 ),
 ( #68169, #6754 ),
 ( #68668, #29095 ),
 ( #99586, #7248 ) ),
 .UNSPECIFIED., .F., .F., .F.,
 ( 4, 1, 4 ),
 ( 2, 2 ),
 ( 0.000000000000000000, 0.4873406636582197082, 0.9999999999999998890 ),
 ( 0.000000000000000000, 1.000000000000000000 ),
 .UNSPECIFIED. ) ;
#60529 = DIRECTION ( 'NONE',  ( 0.000000000000000000, -1.000000000000000000, 0.000000000000000000 ) ) ;
#60530 = FACE_OUTER_BOUND ( 'NONE', #85232, .T. ) ;
#60531 = ORIENTED_EDGE ( 'NONE', *, *, #4542, .F. ) ;
#60532 = CARTESIAN_POINT ( 'NONE',  ( -8.335131950130996614, 18.48905954037022781, -1.500000000000002220 ) ) ;
#60533 = CARTESIAN_POINT ( 'NONE',  ( -68.94617219721770596, -25.27411024655319238, 6.009931644431809161 ) ) ;
#60534 = DIRECTION ( 'NONE',  ( 0.000000000000000000, 0.000000000000000000, 1.000000000000000000 ) ) ;
#60535 = AXIS2_PLACEMENT_3D ( 'NONE', #88783, #80160, #51212 ) ;
#60536 = DIRECTION ( 'NONE',  ( -0.000000000000000000, 1.000000000000000000, -0.000000000000000000 ) ) ;
#60537 = VERTEX_POINT ( 'NONE', #97489 ) ;
#60538 = FACE_OUTER_BOUND ( 'NONE', #93101, .T. ) ;
#60539 = CARTESIAN_POINT ( 'NONE',  ( -62.52287095715006160, -23.47596703998600631, 11.44779298504228926 ) ) ;
#60540 = CARTESIAN_POINT ( 'NONE',  ( -19.81368827760683260, -3.497637702615509880, -1.500000000000002220 ) ) ;
#60541 = AXIS2_PLACEMENT_3D ( 'NONE', #55744, #25268, #71964 ) ;
#60542 = CARTESIAN_POINT ( 'NONE',  ( 8.294003578737715543, -19.35633765900385939, 11.49999999999999645 ) ) ;
#60543 = CARTESIAN_POINT ( 'NONE',  ( -89.81226385320384509, -25.31959802671284265, 5.296208655838286816 ) ) ;
#60544 = CARTESIAN_POINT ( 'NONE',  ( 7.643743511751816655, -20.74876368896106271, 11.49999999999998934 ) ) ;
#60545 = B_SPLINE_CURVE_WITH_KNOTS ( 'NONE', 3,
 ( #99094, #60569, #91487, #67683 ),
 .UNSPECIFIED., .F., .F.,
 ( 4, 4 ),
 ( 0.000000000000000000, 1.000000000000000000 ),
 .UNSPECIFIED. ) ;
#60546 = B_SPLINE_CURVE_WITH_KNOTS ( 'NONE', 3,
 ( #32023, #79196, #3100, #56889, #34035, #94423, #80205, #71101 ),
 .UNSPECIFIED., .F., .F.,
 ( 4, 2, 2, 4 ),
 ( 6.391158118970771556E-06, 0.002007136338672931355, 0.003007508928949909066, 0.004007881519226886777 ),
 .UNSPECIFIED. ) ;
#60547 = CARTESIAN_POINT ( 'NONE',  ( -16.44861368136865920, 12.28130381464353782, 11.49999999999998934 ) ) ;
#60548 = DIRECTION ( 'NONE',  ( 0.000000000000000000, 0.000000000000000000, 1.000000000000000000 ) ) ;
#60549 = CARTESIAN_POINT ( 'NONE',  ( -114.6228709571500559, -24.64965695001469115, 8.947790433994176951 ) ) ;
#60550 = ORIENTED_EDGE ( 'NONE', *, *, #81422, .T. ) ;
#60551 = FACE_OUTER_BOUND ( 'NONE', #57509, .T. ) ;
#60552 = ORIENTED_EDGE ( 'NONE', *, *, #44419, .T. ) ;
#60553 = CARTESIAN_POINT ( 'NONE',  ( -83.22287095715005023, -23.47596703998600631, 11.44779298504227683 ) ) ;
#60554 = CARTESIAN_POINT ( 'NONE',  ( 10.24059822343757986, -6.376774720514426953, 22.82308057603840368 ) ) ;
#60555 = ORIENTED_EDGE ( 'NONE', *, *, #3086, .T. ) ;
#60556 = ORIENTED_EDGE ( 'NONE', *, *, #64503, .F. ) ;
#60557 = CARTESIAN_POINT ( 'NONE',  ( -118.6228709571500701, -24.50216790748100237, 0.6166512839513690336 ) ) ;
#60558 = CARTESIAN_POINT ( 'NONE',  ( -98.62287095715005592, -29.50250243563736774, 8.947779886222138046 ) ) ;
#60559 = CARTESIAN_POINT ( 'NONE',  ( -62.62287095715004881, -29.50247984919015209, -1.443849546365056913 ) ) ;
#60560 = CARTESIAN_POINT ( 'NONE',  ( -9.109090448966927767, 18.51201596650851400, -1.500000000000002220 ) ) ;
#60561 = CARTESIAN_POINT ( 'NONE',  ( -21.34238180412542718, 3.497892552127677135, 11.49999999999999645 ) ) ;
#60562 = VERTEX_POINT ( 'NONE', #15625 ) ;
#60563 = CARTESIAN_POINT ( 'NONE',  ( -46.62287095715004881, -29.50250786944525672, 11.44777988621624054 ) ) ;
#60564 = CARTESIAN_POINT ( 'NONE',  ( 31.63608488009065667, -6.376774720514426953, 27.34773273846995068 ) ) ;
#60565 = CARTESIAN_POINT ( 'NONE',  ( -0.4079105510268487000, 22.33655531192813370, -1.500000000000002220 ) ) ;
#60566 = CARTESIAN_POINT ( 'NONE',  ( -80.48900664166535535, -25.27875090823107485, 7.101635220485683853 ) ) ;
#60567 = DIRECTION ( 'NONE',  ( -3.773278334444167608E-23, 1.000000000000000000, 0.000000000000000000 ) ) ;
#60568 = EDGE_LOOP ( 'NONE', ( #47365, #16832, #99445, #36461 ) ) ;
#60569 = CARTESIAN_POINT ( 'NONE',  ( -43.55620429048339304, -23.47593901973091235, -1.443836447539011525 ) ) ;
#60570 = CARTESIAN_POINT ( 'NONE',  ( -49.57748681740810071, -24.66019654487198665, 8.947790411086131712 ) ) ;
#60571 = ADVANCED_FACE ( 'NONE', ( #46592 ), #74165, .T. ) ;
#60572 = CARTESIAN_POINT ( 'NONE',  ( 18.75483278694074940, -9.228467059531109129, 11.49999999999998934 ) ) ;
#60573 = EDGE_CURVE ( 'NONE', #53725, #13237, #86144, .T. ) ;
#60574 = ORIENTED_EDGE ( 'NONE', *, *, #17925, .F. ) ;
#60576 = ORIENTED_EDGE ( 'NONE', *, *, #27628, .F. ) ;
#60575 = CARTESIAN_POINT ( 'NONE',  ( -86.58558031640687602, -24.51314013834315375, 0.6176544820404177294 ) ) ;
#60577 = ORIENTED_EDGE ( 'NONE', *, *, #4476, .F. ) ;
#60578 = VECTOR ( 'NONE', #18667, 1000.000000000000114 ) ;
#60579 = CARTESIAN_POINT ( 'NONE',  ( -109.6292179679340251, -23.96169478059713853, 10.65365249895717703 ) ) ;
#60580 = CARTESIAN_POINT ( 'NONE',  ( 1.943494986365726485, -21.02143711168614004, -1.500000000000002220 ) ) ;
#60581 = EDGE_LOOP ( 'NONE', ( #26626, #85834, #62827, #98482 ) ) ;
#60582 = CARTESIAN_POINT ( 'NONE',  ( -117.5579596701613951, -23.48783264082477729, -1.443836473390081254 ) ) ;
#60583 = PLANE ( 'NONE',  #28811 ) ;
#60584 = CARTESIAN_POINT ( 'NONE',  ( 21.63681353182189682, 2.665401433100548889, 11.49999999999998934 ) ) ;
#60585 = CARTESIAN_POINT ( 'NONE',  ( -120.6293623597568825, -23.48786465467241769, 11.44779295918253936 ) ) ;
#60586 = CIRCLE ( 'NONE', #10155, 251.4258649670780699 ) ;
#60587 = PLANE ( 'NONE',  #45292 ) ;
#60588 = LINE ( 'NONE', #29112, #46567 ) ;
#60589 = CARTESIAN_POINT ( 'NONE',  ( 1.329761939549756855, 21.69843865049760367, -1.500000000000002220 ) ) ;
#60590 = CARTESIAN_POINT ( 'NONE',  ( -71.44479781437794941, -25.24674145135648828, 5.279211752121547363 ) ) ;
#60592 = ORIENTED_EDGE ( 'NONE', *, *, #63432, .T. ) ;
#60591 = CARTESIAN_POINT ( 'NONE',  ( -19.39139147909919458, -11.06001032434818576, 11.49999999999999645 ) ) ;
#60593 = ADVANCED_FACE ( 'NONE', ( #40479 ), #54214, .F. ) ;
#60594 = DIRECTION ( 'NONE',  ( 0.6559908753439240847, -0.4874460344622444929, 0.5762571777883070956 ) ) ;
#60595 = CARTESIAN_POINT ( 'NONE',  ( -11.64875734969026233, -5.965225279485572685, 31.02402280011862246 ) ) ;
#60596 = CARTESIAN_POINT ( 'NONE',  ( -68.58953762381672448, -24.65952944569304250, 1.056160979905694131 ) ) ;
#60597 = ORIENTED_EDGE ( 'NONE', *, *, #5582, .T. ) ;
#60598 = EDGE_LOOP ( 'NONE', ( #28458, #40178, #86807, #83725 ) ) ;
#60599 = VERTEX_POINT ( 'NONE', #32357 ) ;
#60600 = CARTESIAN_POINT ( 'NONE',  ( -85.55620429048337883, -23.48786465467241058, 11.44779295918254292 ) ) ;
#60601 = CARTESIAN_POINT ( 'NONE',  ( 19.38521227897113874, -8.589346653930519437, -1.500000000000002220 ) ) ;
#60602 = DIRECTION ( 'NONE',  ( -1.000000000000000000, 0.000000000000000000, 0.000000000000000000 ) ) ;
#60603 = DIRECTION ( 'NONE',  ( -1.000000000000000000, 0.000000000000000000, 0.000000000000000000 ) ) ;
#60604 = FACE_OUTER_BOUND ( 'NONE', #64184, .T. ) ;
#60605 = CARTESIAN_POINT ( 'NONE',  ( 5.994920710892026605, -5.876774720514429617, 21.76186867112717138 ) ) ;
#60606 = CARTESIAN_POINT ( 'NONE',  ( -18.68205546197936684, -5.105407162728520021, 11.49999999999998934 ) ) ;
#60607 = DIRECTION ( 'NONE',  ( -1.000000000000000000, 0.000000000000000000, 0.000000000000000000 ) ) ;
#60608 = EDGE_LOOP ( 'NONE', ( #6642, #40319, #59099, #85006 ) ) ;
#60609 = CARTESIAN_POINT ( 'NONE',  ( 15.33136405852079243, -11.96835230219363311, 11.49999999999999645 ) ) ;
#60610 = CARTESIAN_POINT ( 'NONE',  ( -115.5228709571500616, -24.83620972994592435, 8.398175272781369216 ) ) ;
#60611 = EDGE_LOOP ( 'NONE', ( #91977, #39945, #20279, #59312 ) ) ;
#60613 = CARTESIAN_POINT ( 'NONE',  ( -53.52287095715005449, -24.66019654487198665, 8.947790411086121054 ) ) ;
#60612 = VECTOR ( 'NONE', #27331, 999.9999999999998863 ) ;
#60614 = CARTESIAN_POINT ( 'NONE',  ( 2.747717285871495108, -6.376774720514404748, 18.94713297040818034 ) ) ;
#60615 = CARTESIAN_POINT ( 'NONE',  ( -65.22287095715006444, -23.47596703998600631, 11.44779298504227860 ) ) ;
#60616 = CARTESIAN_POINT ( 'NONE',  ( -120.9228709571500531, -23.47596703998600276, 11.44779298504227683 ) ) ;
#60617 = ADVANCED_FACE ( 'NONE', ( #61822 ), #71432, .F. ) ;
#60618 = CARTESIAN_POINT ( 'NONE',  ( 2.166912399371504705, 19.51343182558466793, -1.500000000000002220 ) ) ;
#60619 = VECTOR ( 'NONE', #69266, 1000.000000000000000 ) ;
#60620 = CARTESIAN_POINT ( 'NONE',  ( 8.071512145086499501, -1.000000000000008882, 3.746884140868834923 ) ) ;
#60621 = VERTEX_POINT ( 'NONE', #24737 ) ;
#60622 = CARTESIAN_POINT ( 'NONE',  ( 16.61904782137575154, -13.72857183568914685, 11.49999999999998934 ) ) ;
#60623 = CARTESIAN_POINT ( 'NONE',  ( -33.61929772658547222, -23.48786465467240347, 11.44779295918255535 ) ) ;
#60624 = CARTESIAN_POINT ( 'NONE',  ( -123.5562042904833788, -23.48786465467241769, 11.44779295918253403 ) ) ;
#60625 = CARTESIAN_POINT ( 'NONE',  ( -50.52287095715006160, -24.51163499207180152, 0.6490370598555512682 ) ) ;
#60626 = CARTESIAN_POINT ( 'NONE',  ( -99.99551102217851906, -25.27473239134466354, 3.374614203793048439 ) ) ;
#60627 = CARTESIAN_POINT ( 'NONE',  ( 1.550618966079767347, 22.99078241098900932, -1.500000000000002220 ) ) ;
#60628 = ADVANCED_FACE ( 'NONE', ( #55717 ), #7515, .F. ) ;
#60629 = APPROVAL_DATE_TIME ( #76807, #14687 ) ;
#60630 = CARTESIAN_POINT ( 'NONE',  ( -74.62287095715005592, -23.47596703998600631, 11.44779298504227860 ) ) ;
#60631 = CARTESIAN_POINT ( 'NONE',  ( 29.77147767949874790, -5.356774720514425603, 26.15915692125051706 ) ) ;
#60632 = CARTESIAN_POINT ( 'NONE',  ( 20.11291949428234105, -1.170665973999911902, 11.49999999999999645 ) ) ;
#60633 = CARTESIAN_POINT ( 'NONE',  ( -108.9559085688801616, -25.28814349977695386, 4.125625889878640429 ) ) ;
#60634 = CARTESIAN_POINT ( 'NONE',  ( -32.66840245258526920, -23.48786465467240347, 11.44779295918255535 ) ) ;
#60635 = CARTESIAN_POINT ( 'NONE',  ( -104.5895376238167245, -24.65952944569304606, 1.056160979905699238 ) ) ;
#60636 = DIRECTION ( 'NONE',  ( 1.000000000000000000, 0.000000000000000000, 0.000000000000000000 ) ) ;
#60637 = CARTESIAN_POINT ( 'NONE',  ( -110.3698707892751401, -25.18425582861542367, 3.294862445368111459 ) ) ;
#60638 = CARTESIAN_POINT ( 'NONE',  ( -0.2410636032128395945, 19.88167143085883737, 11.49999999999998934 ) ) ;
#60639 = CARTESIAN_POINT ( 'NONE',  ( -28.98875734969026396, -0.3587747205144265483, 10.11402280011862587 ) ) ;
#60640 = CARTESIAN_POINT ( 'NONE',  ( -1.996473883165060581, 19.68112600131995293, -1.500000000000002220 ) ) ;
#60641 = FACE_OUTER_BOUND ( 'NONE', #5595, .T. ) ;
#60642 = CARTESIAN_POINT ( 'NONE',  ( -125.6228709571500559, -24.99156045073393173, 7.747789690856161648 ) ) ;
#60643 = FACE_OUTER_BOUND ( 'NONE', #24354, .T. ) ;
#60644 = CARTESIAN_POINT ( 'NONE',  ( 16.58470376584361361, 12.37529123428901556, 11.49999999999999645 ) ) ;
#60645 = DIRECTION ( 'NONE',  ( 1.000000000000000000, 3.491481338843133355E-15, 2.352173255807796056E-16 ) ) ;
#60646 = B_SPLINE_CURVE_WITH_KNOTS ( 'NONE', 3,
 ( #32039, #39648, #54386, #46771 ),
 .UNSPECIFIED., .F., .F.,
 ( 4, 4 ),
 ( 0.000000000000000000, 9.999999999997510880E-05 ),
 .UNSPECIFIED. ) ;
#60647 = DIRECTION ( 'NONE',  ( 1.875376730785737473E-16, -1.000000000000000000, 0.000000000000000000 ) ) ;
#60648 = CC_DESIGN_DATE_AND_TIME_ASSIGNMENT ( #51626, #60247, ( #69913 ) ) ;
#60649 = CARTESIAN_POINT ( 'NONE',  ( -50.34100630499489881, -25.25138672863312550, 5.198616883439322933 ) ) ;
#60650 = CARTESIAN_POINT ( 'NONE',  ( 18.51665531608540860, 13.21585733361752801, 11.49999999999999645 ) ) ;
#60651 = ORIENTED_EDGE ( 'NONE', *, *, #72702, .F. ) ;
#60652 = CARTESIAN_POINT ( 'NONE',  ( -60.62287095715003460, -24.83602698348160231, 1.605859176311265513 ) ) ;
#60653 = CARTESIAN_POINT ( 'NONE',  ( 2.449489742783178770, 4.293056017849825601, 2.499999999999999556 ) ) ;
#60654 = CARTESIAN_POINT ( 'NONE',  ( 15.40757771627215256, 13.04930689719894765, 11.49999999999998934 ) ) ;
#60655 = CARTESIAN_POINT ( 'NONE',  ( -63.61013885863124528, -23.48783264082475952, -1.443836473390093245 ) ) ;
#60656 = CARTESIAN_POINT ( 'NONE',  ( -41.42938027069750007, -25.29269197957483328, 4.439299310465838033 ) ) ;
#60657 = EDGE_CURVE ( 'NONE', #53455, #16362, #73045, .T. ) ;
#60658 = ORIENTED_EDGE ( 'NONE', *, *, #8768, .T. ) ;
#60659 = ORIENTED_EDGE ( 'NONE', *, *, #19174, .F. ) ;
#60660 = CARTESIAN_POINT ( 'NONE',  ( 0.3670296583442628213, -6.376774720514417183, 20.26087634804755311 ) ) ;
#60661 = CARTESIAN_POINT ( 'NONE',  ( 22.59171682324826236, -3.780823453261925593, 11.49999999999998934 ) ) ;
#60662 = DIRECTION ( 'NONE',  ( 0.000000000000000000, 0.9999999999976377785, 2.173523156925979128E-06 ) ) ;
#60663 = CARTESIAN_POINT ( 'NONE',  ( -13.25059585359799108, -17.08168364658555305, -1.500000000000002220 ) ) ;
#60664 = LINE ( 'NONE', #98701, #73914 ) ;
#60665 = LINE ( 'NONE', #68761, #33904 ) ;
#60666 = CARTESIAN_POINT ( 'NONE',  ( 3.889286922045745776, 20.52237432693057073, 11.49999999999999645 ) ) ;
#60667 = ORIENTED_EDGE ( 'NONE', *, *, #63672, .T. ) ;
#60668 = CARTESIAN_POINT ( 'NONE',  ( -8.160000000000000142, -10.15233964170348457, 0.003711184059992174607 ) ) ;
#60669 = CARTESIAN_POINT ( 'NONE',  ( 17.71009474140864981, 13.04663522181963309, -1.500000000000002220 ) ) ;
#60670 = AXIS2_PLACEMENT_3D ( 'NONE', #78079, #79595, #24309 ) ;
#60671 = CARTESIAN_POINT ( 'NONE',  ( -105.5081692944722818, -24.92592662359561473, 8.075495903018000021 ) ) ;
#60672 = CARTESIAN_POINT ( 'NONE',  ( -28.57615893954310238, -25.21724918667983673, 7.256891368531773523 ) ) ;
#60673 = EDGE_LOOP ( 'NONE', ( #59421, #65350, #11687, #34475 ) ) ;
#60674 = DIRECTION ( 'NONE',  ( 0.000000000000000000, -1.000000000000000000, 0.000000000000000000 ) ) ;
#60675 = DIRECTION ( 'NONE',  ( -1.000000000000000000, -5.204170427930421283E-15, 0.000000000000000000 ) ) ;
#60676 = EDGE_LOOP ( 'NONE', ( #68301, #40649, #58904, #1819 ) ) ;
#60677 = PLANE ( 'NONE',  #1612 ) ;
#60678 = ORIENTED_EDGE ( 'NONE', *, *, #429, .T. ) ;
#60679 = ORIENTED_EDGE ( 'NONE', *, *, #55514, .F. ) ;
#60680 = ADVANCED_FACE ( 'NONE', ( #16126 ), #33497, .T. ) ;
#60681 = CARTESIAN_POINT ( 'NONE',  ( 8.063330319165388005, -10.15233964170352898, 1.310587897985993955 ) ) ;
#60682 = CARTESIAN_POINT ( 'NONE',  ( -101.5937515207030657, -25.27404774504482887, 3.495447232644239399 ) ) ;
#60683 = CARTESIAN_POINT ( 'NONE',  ( -27.25988310792305214, 5.965225279485572685, 30.32664379231667695 ) ) ;
#60684 = CARTESIAN_POINT ( 'NONE',  ( 15.88337727998148985, 12.78846505907953279, -1.500000000000002220 ) ) ;
#60685 = AXIS2_PLACEMENT_3D ( 'NONE', #57319, #34958, #33957 ) ;
#60686 = ORIENTED_EDGE ( 'NONE', *, *, #58112, .F. ) ;
#60687 = CARTESIAN_POINT ( 'NONE',  ( -0.7067007548136460260, -5.876774720514410966, 19.51517878119693350 ) ) ;
#60688 = CARTESIAN_POINT ( 'NONE',  ( -30.60515864328932878, -24.57438384523503316, 0.5319095616429411200 ) ) ;
#60689 = DIRECTION ( 'NONE',  ( -0.000000000000000000, 0.000000000000000000, -1.000000000000000000 ) ) ;
#60690 = DIRECTION ( 'NONE',  ( -1.000000000000000000, 0.000000000000000000, 0.000000000000000000 ) ) ;
#60691 = ORIENTED_EDGE ( 'NONE', *, *, #13208, .T. ) ;
#60692 = LINE ( 'NONE', #35844, #38669 ) ;
#60693 = CARTESIAN_POINT ( 'NONE',  ( -29.31102972132424966, -24.63645865963270865, 7.337444170384009645 ) ) ;
#60694 = EDGE_CURVE ( 'NONE', #82898, #32935, #8860, .T. ) ;
#60695 = CARTESIAN_POINT ( 'NONE',  ( 20.70993026999094511, 1.908435391604796028, -1.500000000000002220 ) ) ;
#60696 = EDGE_CURVE ( 'NONE', #55815, #2790, #96726, .T. ) ;
#60697 = ORIENTED_EDGE ( 'NONE', *, *, #70209, .T. ) ;
#60699 = VERTEX_POINT ( 'NONE', #26749 ) ;
#60698 = CARTESIAN_POINT ( 'NONE',  ( -42.52287095715006160, -23.96177878511308279, 10.65340807706331283 ) ) ;
#60700 = DIRECTION ( 'NONE',  ( -0.000000000000000000, 1.000000000000000000, -0.000000000000000000 ) ) ;
#60701 = VERTEX_POINT ( 'NONE', #49104 ) ;
#60702 = ORIENTED_EDGE ( 'NONE', *, *, #98073, .F. ) ;
#60703 = FACE_OUTER_BOUND ( 'NONE', #54925, .T. ) ;
#60704 = CARTESIAN_POINT ( 'NONE',  ( -92.62287095715008434, -24.51387760970724017, 9.387446482453416507 ) ) ;
#60705 = CARTESIAN_POINT ( 'NONE',  ( -116.6623382465025145, -25.28334050553294787, 4.245309122437062932 ) ) ;
#60706 = CARTESIAN_POINT ( 'NONE',  ( -100.4979344782931037, -25.03152448927857066, 7.562057945188089825 ) ) ;
#60707 = B_SPLINE_CURVE_WITH_KNOTS ( 'NONE', 3,
 ( #51078, #74891, #27241, #28735 ),
 .UNSPECIFIED., .F., .F.,
 ( 4, 4 ),
 ( 0.000000000000000000, 1.000000000000000000 ),
 .UNSPECIFIED. ) ;
#60708 = CARTESIAN_POINT ( 'NONE',  ( -108.9572543305703363, -25.28095782085471299, 4.080816019651302362 ) ) ;
#60709 = DIRECTION ( 'NONE',  ( -2.246662546894773332E-15, 7.121496375062676691E-15, -1.000000000000000000 ) ) ;
#60711 = ORIENTED_EDGE ( 'NONE', *, *, #6706, .F. ) ;
#60710 = CARTESIAN_POINT ( 'NONE',  ( -13.28819421967561532, -17.68372732473523001, 11.49999999999999645 ) ) ;
#60712 = EDGE_CURVE ( 'NONE', #6687, #56269, #98351, .T. ) ;
#60713 = CARTESIAN_POINT ( 'NONE',  ( -105.5895376238167387, -23.47596703998600631, 11.44779298504227683 ) ) ;
#60714 = CARTESIAN_POINT ( 'NONE',  ( -22.62345309801473547, -0.4825844212548152656, -1.500000000000002220 ) ) ;
#60715 = SHAPE_REPRESENTATION ( 'Hook_Varsay\X2\0131\X0\lan', ( #37391 ), #35871 ) ;
#60717 = ORIENTED_EDGE ( 'NONE', *, *, #36693, .F. ) ;
#60716 = CARTESIAN_POINT ( 'NONE',  ( -77.52287095715006160, -24.66019654487200086, 8.947790411086113949 ) ) ;
#60718 = ORIENTED_EDGE ( 'NONE', *, *, #98973, .F. ) ;
#60719 = AXIS2_PLACEMENT_3D ( 'NONE', #691, #54485, #93029 ) ;
#60720 = CARTESIAN_POINT ( 'NONE',  ( -10.54059822343757702, -6.376774720514426953, 17.17691942396159988 ) ) ;
#60721 = CARTESIAN_POINT ( 'NONE',  ( -19.48533387766964964, -5.011242947278518045, 11.49999999999998934 ) ) ;
#60722 = B_SPLINE_SURFACE_WITH_KNOTS ( 'NONE', 3, 3, ( 
 ( #37995, #32890, #33884, #17154 ),
 ( #48120, #63863, #79554, #1946 ),
 ( #25264, #94776, #80055, #88178 ),
 ( #72455, #79050, #63358, #18156 ),
 ( #48628, #96284, #33375, #55740 ),
 ( #18646, #64363, #16649, #34387 ),
 ( #56243, #87168, #56743, #87674 ) ),
 .UNSPECIFIED., .F., .F., .F.,
 ( 4, 3, 4 ),
 ( 4, 4 ),
 ( 0.0004766839783845008469, 0.1029713700210910104, 0.2054660560637975308 ),
 ( 0.1595345801196773328, 0.1606209136378454749 ),
 .UNSPECIFIED. ) ;
#60723 = PLANE ( 'NONE',  #5242 ) ;
#60724 = VERTEX_POINT ( 'NONE', #35370 ) ;
#60725 = FACE_OUTER_BOUND ( 'NONE', #49688, .T. ) ;
#60726 = CARTESIAN_POINT ( 'NONE',  ( -1.228339276683141579, -22.28195500894762660, -1.500000000000002220 ) ) ;
#60727 = ORIENTED_EDGE ( 'NONE', *, *, #78327, .F. ) ;
#60728 = ORIENTED_EDGE ( 'NONE', *, *, #80950, .T. ) ;
#60729 = CARTESIAN_POINT ( 'NONE',  ( -101.3540785649959304, -25.25341200507040540, 6.680569176468658554 ) ) ;
#60730 = CARTESIAN_POINT ( 'NONE',  ( -81.78154518342495294, -25.18542598755805884, 6.709299554139687594 ) ) ;
#60731 = SPHERICAL_SURFACE ( 'NONE', #84670, 6.600000000000001421 ) ;
#60732 = CARTESIAN_POINT ( 'NONE',  ( -47.55620429048338593, -24.64898659630528499, 1.056161002820819261 ) ) ;
#60733 = FACE_BOUND ( 'NONE', #38954, .T. ) ;
#60734 = CARTESIAN_POINT ( 'NONE',  ( 18.95637782189878706, 4.751392969308117387, 11.49999999999998934 ) ) ;
#60735 = CARTESIAN_POINT ( 'NONE',  ( -65.62287095715005592, -24.99156045073393173, 7.747789690856161648 ) ) ;
#60736 = CARTESIAN_POINT ( 'NONE',  ( -13.16228656746626591, 16.97819584282690286, -1.500000000000002220 ) ) ;
#60737 = CARTESIAN_POINT ( 'NONE',  ( -2.762050907158362989, -5.876774720514413630, 19.89644244529369033 ) ) ;
#60738 = CARTESIAN_POINT ( 'NONE',  ( -117.5228709571500758, -29.50248528299804818, 1.056150453629045360 ) ) ;
#60739 = CARTESIAN_POINT ( 'NONE',  ( 26.25551457520355214, -500000.0000000000582, -10.59759736550658360 ) ) ;
#60741 = CIRCLE ( 'NONE', #4025, 0.3000000000000016542 ) ;
#60740 = CARTESIAN_POINT ( 'NONE',  ( 22.28265747778879202, 5.072132558558076099, -1.500000000000002220 ) ) ;
#60742 = ADVANCED_FACE ( 'NONE', ( #80532 ), #72933, .F. ) ;
#60743 = APPROVAL_DATE_TIME ( #44004, #56303 ) ;
#60744 = CARTESIAN_POINT ( 'NONE',  ( -106.5198638994752542, -23.73791477778912551, 11.05961554403169700 ) ) ;
#60745 = FACE_OUTER_BOUND ( 'NONE', #57919, .T. ) ;
#60746 = CARTESIAN_POINT ( 'NONE',  ( -17.52048005523606022, -9.576713672051738513, 11.49999999999999645 ) ) ;
#60747 = FACE_OUTER_BOUND ( 'NONE', #13014, .T. ) ;
#60748 = CARTESIAN_POINT ( 'NONE',  ( -123.6228709571500559, -24.64898659630368627, 1.056161002820833028 ) ) ;
#60749 = CARTESIAN_POINT ( 'NONE',  ( -43.92287095715007439, -23.47593901973090524, -1.443836447538998424 ) ) ;
#60750 = ORIENTED_EDGE ( 'NONE', *, *, #47260, .T. ) ;
#60751 = CARTESIAN_POINT ( 'NONE',  ( -27.51805182407180794, -24.60240642400831135, 1.634233119128260636 ) ) ;
#60752 = DIRECTION ( 'NONE',  ( -0.6451914333552656311, 0.000000000000000000, -0.7640209514960816239 ) ) ;
#60753 = AXIS2_PLACEMENT_3D ( 'NONE', #44086, #19238, #11624 ) ;
#60754 = CARTESIAN_POINT ( 'NONE',  ( -19.25911440464646063, 10.06369110047026538, -1.500000000000002220 ) ) ;
#60755 = CARTESIAN_POINT ( 'NONE',  ( -55.62287095715004170, -29.50249982740957577, 7.747779886224967605 ) ) ;
#60756 = CARTESIAN_POINT ( 'NONE',  ( -15.04504930077994196, -12.58455232801425794, -1.500000000000002220 ) ) ;
#60757 = DIRECTION ( 'NONE',  ( 0.000000000000000000, 2.173523156925980399E-06, -0.9999999999976378895 ) ) ;
#60758 = ORIENTED_EDGE ( 'NONE', *, *, #11130, .T. ) ;
#60759 = COORDINATED_UNIVERSAL_TIME_OFFSET ( 0, 0, .AHEAD. ) ;
#60760 = CARTESIAN_POINT ( 'NONE',  ( 9.843544857143434967, -5.965225279485572685, -27.49819965379373343 ) ) ;
#60761 = CARTESIAN_POINT ( 'NONE',  ( 2.933277810221831761, -6.376774720514424288, 21.39432064584807947 ) ) ;
#60762 = CARTESIAN_POINT ( 'NONE',  ( -18.81443736134900035, 8.205417114561466718, 11.49999999999999645 ) ) ;
#60763 = CARTESIAN_POINT ( 'NONE',  ( -28.98875734969026396, 5.965225279485572685, -0.08597719988137648983 ) ) ;
#60764 = LINE ( 'NONE', #6465, #98307 ) ;
#60765 = EDGE_CURVE ( 'NONE', #26090, #86743, #20890, .T. ) ;
#60766 = ORIENTED_EDGE ( 'NONE', *, *, #10044, .T. ) ;
#60767 = CARTESIAN_POINT ( 'NONE',  ( -110.0171095414734737, -25.30123833581429338, 5.384701099344828101 ) ) ;
#60768 = CARTESIAN_POINT ( 'NONE',  ( -40.42371425561744047, -25.18430871546082628, 3.294940290805283389 ) ) ;
#60769 = CARTESIAN_POINT ( 'NONE',  ( 3.750000000000001332, 25.69999999999999574, 2.100000000000000089 ) ) ;
#60770 = EDGE_CURVE ( 'NONE', #79708, #69943, #89151, .T. ) ;
#60771 = B_SPLINE_CURVE_WITH_KNOTS ( 'NONE', 3,
 ( #13375, #91499, #38213, #45348, #45840, #44354 ),
 .UNSPECIFIED., .F., .F.,
 ( 4, 2, 4 ),
 ( 0.000000000000000000, 0.001380901958385395700, 0.002761803916770791401 ),
 .UNSPECIFIED. ) ;
#60772 = DIRECTION ( 'NONE',  ( 0.000000000000000000, -2.173523156925980399E-06, 0.9999999999976378895 ) ) ;
#60773 = CARTESIAN_POINT ( 'NONE',  ( -99.52287095715006160, -23.48786465467241769, 11.44779295918254114 ) ) ;
#60774 = ADVANCED_FACE ( 'NONE', ( #18625 ), #79532, .F. ) ;
#60775 = B_SPLINE_CURVE_WITH_KNOTS ( 'NONE', 3,
 ( #22157, #78447, #55140, #24168 ),
 .UNSPECIFIED., .F., .F.,
 ( 4, 4 ),
 ( 8.673617379884035472E-19, 0.0002632372126714214219 ),
 .UNSPECIFIED. ) ;
#60776 = EDGE_CURVE ( 'NONE', #50270, #23352, #58698, .T. ) ;
#60777 = CARTESIAN_POINT ( 'NONE',  ( 5.194767643164344584, 22.50260600399833422, 11.49999999999999645 ) ) ;
#60778 = CARTESIAN_POINT ( 'NONE',  ( 22.20583189720066741, -5.198064566299082756, -1.500000000000002220 ) ) ;
#60779 = CARTESIAN_POINT ( 'NONE',  ( -110.5150696451292021, -24.40133493613049609, 9.663955038902800609 ) ) ;
#60780 = CARTESIAN_POINT ( 'NONE',  ( -75.52287095715013265, -24.82576562948882071, 8.398263436605672538 ) ) ;
#60781 = CARTESIAN_POINT ( 'NONE',  ( -123.5228709571500190, -24.51283580621364777, 0.6167428607019826980 ) ) ;
#60782 = ADVANCED_FACE ( 'NONE', ( #42985 ), #34366, .T. ) ;
#60783 = B_SPLINE_CURVE_WITH_KNOTS ( 'NONE', 3,
 ( #50249, #96415, #26901, #66981 ),
 .UNSPECIFIED., .F., .F.,
 ( 4, 4 ),
 ( 0.000000000000000000, 0.0001000000000000028644 ),
 .UNSPECIFIED. ) ;
#60784 = CIRCLE ( 'NONE', #33245, 1.836000000000000743 ) ;
#60785 = CARTESIAN_POINT ( 'NONE',  ( -62.52287095715006160, -29.50248528299804818, 1.056150453629034924 ) ) ;
#60786 = CARTESIAN_POINT ( 'NONE',  ( -110.5193718685209774, -23.85016227208580020, -0.8807180028928306426 ) ) ;
#60787 = CARTESIAN_POINT ( 'NONE',  ( -19.33260374144687077, -10.33727041909969380, -1.500000000000002220 ) ) ;
#60788 = CARTESIAN_POINT ( 'NONE',  ( -69.52210420424350446, -23.48786465467240347, 11.44779295918255002 ) ) ;
#60789 = DIRECTION ( 'NONE',  ( -3.773278334453079030E-23, 0.9999999999976377785, 2.173523156925979128E-06 ) ) ;
#60790 = CYLINDRICAL_SURFACE ( 'NONE', #97298, 1.050000000000000488 ) ;
#60791 = CARTESIAN_POINT ( 'NONE',  ( -78.50466238525980600, -24.34968618360933945, 0.1864209137778830849 ) ) ;
#60792 = CARTESIAN_POINT ( 'NONE',  ( -112.5228709571500616, -24.66019654487200441, 8.947790411086108620 ) ) ;
#60793 = CARTESIAN_POINT ( 'NONE',  ( -76.52287095715011844, -23.48783264082477373, -1.443836473390087694 ) ) ;
#60794 = ORIENTED_EDGE ( 'NONE', *, *, #51393, .T. ) ;
#60795 = CARTESIAN_POINT ( 'NONE',  ( 7.241121213506172438, 19.11196469071355963, -1.500000000000002220 ) ) ;
#60796 = ORIENTED_EDGE ( 'NONE', *, *, #52088, .F. ) ;
#60797 = EDGE_LOOP ( 'NONE', ( #29324, #29901, #70901, #30350 ) ) ;
#60798 = ORIENTED_EDGE ( 'NONE', *, *, #31008, .F. ) ;
#60799 = ORIENTED_EDGE ( 'NONE', *, *, #78276, .F. ) ;
#60800 = EDGE_CURVE ( 'NONE', #46021, #17843, #86322, .T. ) ;
#60801 = CARTESIAN_POINT ( 'NONE',  ( 19.44587849558928738, -12.39355811350142922, 11.49999999999998934 ) ) ;
#60802 = LINE ( 'NONE', #99820, #40584 ) ;
#60803 = CARTESIAN_POINT ( 'NONE',  ( 10.87751022112437482, 17.06716278085755079, -1.500000000000002220 ) ) ;
#60804 = EDGE_LOOP ( 'NONE', ( #48936, #86069, #56182, #68039, #71953, #27516 ) ) ;
#60805 = CARTESIAN_POINT ( 'NONE',  ( -48.52287095715006160, -24.64965694238574656, 8.947790433994203596 ) ) ;
#60806 = DIRECTION ( 'NONE',  ( -0.000000000000000000, 0.000000000000000000, -1.000000000000000000 ) ) ;
#60807 = CARTESIAN_POINT ( 'NONE',  ( -28.52287095715007226, -24.17764966940397287, 9.819270424401523201 ) ) ;
#60808 = CARTESIAN_POINT ( 'NONE',  ( -99.56068028760604705, -23.48786465467241413, 11.44779295918254469 ) ) ;
#60810 = ORIENTED_EDGE ( 'NONE', *, *, #77825, .F. ) ;
#60809 = CARTESIAN_POINT ( 'NONE',  ( 21.36505145794347982, 1.902718533054148509, 11.49999999999999645 ) ) ;
#60811 = CARTESIAN_POINT ( 'NONE',  ( -128.6228709571500133, -23.72747288104441665, -1.053458166803660001 ) ) ;
#60812 = CARTESIAN_POINT ( 'NONE',  ( 14.56569730433581533, 3.366897624368340391, -28.38594530802162197 ) ) ;
#60813 = VERTEX_POINT ( 'NONE', #96264 ) ;
#60814 = CARTESIAN_POINT ( 'NONE',  ( -14.56105648253378781, -14.73650127990469016, -1.500000000000002220 ) ) ;
#60815 = AXIS2_PLACEMENT_3D ( 'NONE', #17556, #65266, #27176 ) ;
#60816 = EDGE_CURVE ( 'NONE', #81403, #88020, #7601, .T. ) ;
#60818 = ORIENTED_EDGE ( 'NONE', *, *, #32985, .F. ) ;
#60817 = CARTESIAN_POINT ( 'NONE',  ( -80.52287095715007581, -23.48783264082477018, -1.443836473390091246 ) ) ;
#60819 = B_SPLINE_CURVE_WITH_KNOTS ( 'NONE', 3,
 ( #21115, #14505, #20622, #98239, #44475, #37363, #90145, #74419, #76395, #5899, #6897, #51090, #52580, #67822, #60705, #61209, #74902, #36858 ),
 .UNSPECIFIED., .F., .F.,
 ( 4, 2, 2, 2, 2, 2, 2, 2, 4 ),
 ( 0.000000000000000000, 0.0005889166363242080444, 0.001177833272648416089, 0.001766749908972623266, 0.002355666545296830443, 0.002944583181621037403, 0.003533499817945244363, 0.004122416454269450456, 0.004711333090593654814 ),
 .UNSPECIFIED. ) ;
#60820 = EDGE_CURVE ( 'NONE', #74863, #13066, #27255, .T. ) ;
#60821 = CARTESIAN_POINT ( 'NONE',  ( -28.62375884954849425, -24.50672967435375682, 1.056161677404372501 ) ) ;
#60822 = ORIENTED_EDGE ( 'NONE', *, *, #30630, .T. ) ;
#60823 = CARTESIAN_POINT ( 'NONE',  ( 4.912344403463128728, -5.876774720514406525, 19.26008510998990886 ) ) ;
#60824 = VERTEX_POINT ( 'NONE', #88156 ) ;
#60825 = CARTESIAN_POINT ( 'NONE',  ( -16.59477544326466969, -14.39948450415919723, 11.49999999999999645 ) ) ;
#60826 = EDGE_CURVE ( 'NONE', #46180, #81702, #48784, .T. ) ;
#60827 = AXIS2_PLACEMENT_3D ( 'NONE', #65833, #89150, #81542 ) ;
#60828 = CARTESIAN_POINT ( 'NONE',  ( -37.56099278926783569, -23.73791477778911130, 11.05961554403171299 ) ) ;
#60829 = CARTESIAN_POINT ( 'NONE',  ( 6.936750662203477802, 21.44973376661030429, 11.49999999999998934 ) ) ;
#60830 = AXIS2_PLACEMENT_3D ( 'NONE', #15468, #69773, #250 ) ;
#60831 = CARTESIAN_POINT ( 'NONE',  ( 10.18035917307295435, 18.35650967997132099, -1.500000000000002220 ) ) ;
#60832 = EDGE_CURVE ( 'NONE', #27382, #75557, #81543, .T. ) ;
#60833 = CARTESIAN_POINT ( 'NONE',  ( -108.9605944373618343, -25.29717339419269706, 4.328833245316407563 ) ) ;
#60834 = DIRECTION ( 'NONE',  ( 0.000000000000000000, 0.000000000000000000, -1.000000000000000000 ) ) ;
#60835 = ORIENTED_EDGE ( 'NONE', *, *, #76328, .F. ) ;
#60836 = EDGE_CURVE ( 'NONE', #84257, #19500, #29348, .T. ) ;
#60837 = VERTEX_POINT ( 'NONE', #21609 ) ;
#60838 = VERTEX_POINT ( 'NONE', #30227 ) ;
#60839 = CARTESIAN_POINT ( 'NONE',  ( -66.54011281632980968, -24.51314013834316441, 0.6176544820404136216 ) ) ;
#60840 = CARTESIAN_POINT ( 'NONE',  ( 16.61460563260716583, 13.71664681387569118, -1.500000000000002220 ) ) ;
#60841 = LINE ( 'NONE', #91759, #89422 ) ;
#60842 = ORIENTED_EDGE ( 'NONE', *, *, #53502, .T. ) ;
#60843 = CARTESIAN_POINT ( 'NONE',  ( 6.686094007546604878, -20.02240253118446844, -1.500000000000002220 ) ) ;
#60844 = LINE ( 'NONE', #92266, #31971 ) ;
#60845 = CARTESIAN_POINT ( 'NONE',  ( 22.02124265030973760, -4.543225279485573864, 18.45402280011862217 ) ) ;
#60846 = CARTESIAN_POINT ( 'NONE',  ( -64.52287095715006160, -23.48783264082476308, -1.443836473390094355 ) ) ;
#60847 = PLANE ( 'NONE',  #96065 ) ;
#60848 = CARTESIAN_POINT ( 'NONE',  ( -5.891025641025637860, -6.376774720514427841, 21.75000000000000711 ) ) ;
#60849 = CARTESIAN_POINT ( 'NONE',  ( -14.73459587841175633, -16.56598928932902837, -1.500000000000002220 ) ) ;
#60850 = CARTESIAN_POINT ( 'NONE',  ( -71.49518700469006660, -24.65952944569304961, 1.056160979905700570 ) ) ;
#60851 = EDGE_LOOP ( 'NONE', ( #56213, #71129 ) ) ;
#60852 = CARTESIAN_POINT ( 'NONE',  ( -51.92928322226379123, -25.24860240139651424, 6.080069520644998171 ) ) ;
#60853 = CARTESIAN_POINT ( 'NONE',  ( -108.5228709571501042, -24.66019654487200441, 8.947790411086113949 ) ) ;
#60854 = CARTESIAN_POINT ( 'NONE',  ( 30.53060340732036337, 5.329285123471892760, 3.289350009555732868 ) ) ;
#60855 = CARTESIAN_POINT ( 'NONE',  ( -100.6305679976983356, -24.40034930558990567, 0.3402023900116026844 ) ) ;
#60856 = CARTESIAN_POINT ( 'NONE',  ( -17.86923650574433609, -7.721772263035739492, -1.500000000000002220 ) ) ;
#60857 = VECTOR ( 'NONE', #1990, 1000.000000000000000 ) ;
#60858 = CARTESIAN_POINT ( 'NONE',  ( -19.99122433398336440, 7.574256484821010105, -1.500000000000002220 ) ) ;
#60859 = CARTESIAN_POINT ( 'NONE',  ( 1.305682803664691249, -0.3587747205144265483, 29.57950906855421991 ) ) ;
#60860 = CARTESIAN_POINT ( 'NONE',  ( -89.80413383862705246, -25.26877915520014639, 5.947789088310639904 ) ) ;
#60861 = CARTESIAN_POINT ( 'NONE',  ( 10.46399479596398052, 3.316774720514422903, -27.03001098546561209 ) ) ;
#60862 = CARTESIAN_POINT ( 'NONE',  ( -36.62287095715006302, -23.96177878511307568, 10.65340807706330928 ) ) ;
#60863 = CARTESIAN_POINT ( 'NONE',  ( -18.74212433040710479, 12.77821124017617649, -1.500000000000002220 ) ) ;
#60864 = ORIENTED_EDGE ( 'NONE', *, *, #75467, .T. ) ;
#60865 = CARTESIAN_POINT ( 'NONE',  ( -87.52287095715004739, -24.51387760970724727, 9.387446482453409402 ) ) ;
#60866 = CARTESIAN_POINT ( 'NONE',  ( -41.22287095715006444, -23.47596703998600631, 11.44779298504227683 ) ) ;
#60867 = CARTESIAN_POINT ( 'NONE',  ( -12.28770250403618114, -15.54288071925545722, 11.49999999999999645 ) ) ;
#60868 = FACE_OUTER_BOUND ( 'NONE', #63036, .T. ) ;
#60869 = ORIENTED_EDGE ( 'NONE', *, *, #85319, .T. ) ;
#60870 = CARTESIAN_POINT ( 'NONE',  ( -68.58953762381671027, -24.66019654487199375, 8.947790411086124607 ) ) ;
#60871 = CARTESIAN_POINT ( 'NONE',  ( 0.5999240985075874333, 1.411520799013914917, 8.999999999999987566 ) ) ;
#60872 = CARTESIAN_POINT ( 'NONE',  ( -12.93760099376155104, 17.33828479246177423, 11.49999999999998934 ) ) ;
#60873 = CARTESIAN_POINT ( 'NONE',  ( -99.62287095715005592, -23.48783264082478794, -1.443836473390061936 ) ) ;
#60874 = CARTESIAN_POINT ( 'NONE',  ( -19.30698013599780083, -2.078282243779251637, -1.500000000000002220 ) ) ;
#60875 = CARTESIAN_POINT ( 'NONE',  ( -114.5562042904833504, -24.64965694238575011, 8.947790433994187609 ) ) ;
#60876 = FACE_OUTER_BOUND ( 'NONE', #79265, .T. ) ;
#60877 = CARTESIAN_POINT ( 'NONE',  ( 9.171884637996585710, -17.55225146786146695, -1.500000000000002220 ) ) ;
#60878 = ORIENTED_EDGE ( 'NONE', *, *, #27890, .F. ) ;
#60879 = CARTESIAN_POINT ( 'NONE',  ( 18.28078834835902455, 8.925752885971231620, 11.49999999999999645 ) ) ;
#60880 = CARTESIAN_POINT ( 'NONE',  ( -106.6228709571500559, -29.50250243563736774, 8.947779886222136270 ) ) ;
#60881 = AXIS2_PLACEMENT_3D ( 'NONE', #86481, #16967, #47930 ) ;
#60882 = CARTESIAN_POINT ( 'NONE',  ( 33.41263754283357912, -3.496799131921995762, -12.47286811689047070 ) ) ;
#60883 = ADVANCED_FACE ( 'NONE', ( #83517 ), #53092, .T. ) ;
#60884 = VERTEX_POINT ( 'NONE', #37850 ) ;
#60885 = CARTESIAN_POINT ( 'NONE',  ( -102.5888613629790882, -24.35071581493543391, 9.817618358456027039 ) ) ;
#60886 = CARTESIAN_POINT ( 'NONE',  ( -95.52287095715010423, -24.14406661686761524, 10.28769366194074841 ) ) ;
#60887 = CARTESIAN_POINT ( 'NONE',  ( -96.62287095715005592, -23.47596703998600631, 11.44779298504227860 ) ) ;
#60888 = EDGE_CURVE ( 'NONE', #57568, #9886, #93490, .T. ) ;
#60889 = CARTESIAN_POINT ( 'NONE',  ( -40.48992741903451531, -24.40133493613049609, 9.663955038902802386 ) ) ;
#60890 = VECTOR ( 'NONE', #30496, 1000.000000000000000 ) ;
#60891 = CARTESIAN_POINT ( 'NONE',  ( -1.030996059302438761, -5.876774720514415407, 20.06599527532949878 ) ) ;
#60892 = CARTESIAN_POINT ( 'NONE',  ( -6.237196068801617699, -19.06703463882530158, -1.500000000000002220 ) ) ;
#60893 = B_SPLINE_CURVE_WITH_KNOTS ( 'NONE', 3,
 ( #32325, #94216, #56688, #879 ),
 .UNSPECIFIED., .F., .F.,
 ( 4, 4 ),
 ( 0.000000000000000000, 0.0001000000000000028644 ),
 .UNSPECIFIED. ) ;
#60894 = CIRCLE ( 'NONE', #21955, 6.000000000000000888 ) ;
#60895 = CARTESIAN_POINT ( 'NONE',  ( -29.49875734969025842, 0.3587747205144265483, 17.86602280011862476 ) ) ;
#60896 = ORIENTED_EDGE ( 'NONE', *, *, #26053, .T. ) ;
#60897 = DIRECTION ( 'NONE',  ( 0.5630016722799281448, -5.365801633547219206E-16, -0.8264557562326033668 ) ) ;
#60898 = EDGE_CURVE ( 'NONE', #52727, #76836, #12456, .T. ) ;
#60899 = EDGE_CURVE ( 'NONE', #63331, #60884, #60819, .T. ) ;
#60900 = CARTESIAN_POINT ( 'NONE',  ( 18.88093902437788785, 12.95799798663108682, 11.49999999999999645 ) ) ;
#60901 = CARTESIAN_POINT ( 'NONE',  ( -22.72798930328562150, -0.2126449523330483371, 11.49999999999998934 ) ) ;
#60902 = CARTESIAN_POINT ( 'NONE',  ( -105.6228709571500559, -23.47593901973091235, -1.443836447538999312 ) ) ;
#60903 = CARTESIAN_POINT ( 'NONE',  ( -97.62287095715005592, -23.47593901973091235, -1.443836447539001089 ) ) ;
#60904 = CARTESIAN_POINT ( 'NONE',  ( -35.52287095715006870, -29.50248528299804818, 1.056150453629031594 ) ) ;
#60905 = ADVANCED_FACE ( 'NONE', ( #68305 ), #98745, .T. ) ;
#60906 = CARTESIAN_POINT ( 'NONE',  ( 30.55775998287478856, -1.765878758506237434, 24.49934028559106736 ) ) ;
#60907 = CARTESIAN_POINT ( 'NONE',  ( -31.62287095715005236, -23.47593901973091235, -1.443836447539013301 ) ) ;
#60908 = DIRECTION ( 'NONE',  ( -0.000000000000000000, 1.000000000000000000, -0.000000000000000000 ) ) ;
#60909 = ORIENTED_EDGE ( 'NONE', *, *, #58382, .T. ) ;
#60910 = CARTESIAN_POINT ( 'NONE',  ( -20.29798418530817017, 1.744846428065259136, 11.49999999999998934 ) ) ;
#60911 = VERTEX_POINT ( 'NONE', #60206 ) ;
#60912 = EDGE_CURVE ( 'NONE', #16787, #4203, #30297, .T. ) ;
#60913 = CARTESIAN_POINT ( 'NONE',  ( 13.56796309060646166, -18.52494293750034871, 11.49999999999998934 ) ) ;
#60914 = DIRECTION ( 'NONE',  ( 0.000000000000000000, 0.000000000000000000, -1.000000000000000000 ) ) ;
#60915 = ORIENTED_EDGE ( 'NONE', *, *, #82881, .T. ) ;
#60916 = CARTESIAN_POINT ( 'NONE',  ( -108.5864047394081950, -24.66019654487200441, 8.947790411086108620 ) ) ;
#60917 = CARTESIAN_POINT ( 'NONE',  ( -77.50092983151746751, -24.51419770103158768, 9.386484678747166299 ) ) ;
#60918 = EDGE_CURVE ( 'NONE', #31713, #16621, #59424, .T. ) ;
#60919 = DIRECTION ( 'NONE',  ( 0.000000000000000000, 0.000000000000000000, -1.000000000000000000 ) ) ;
#60921 = EDGE_LOOP ( 'NONE', ( #96639, #22595, #66122, #28261 ) ) ;
#60920 = CARTESIAN_POINT ( 'NONE',  ( -3.120219904758775975, 21.05623772282662998, 11.49999999999999645 ) ) ;
#60922 = VERTEX_POINT ( 'NONE', #91626 ) ;
#60923 = CARTESIAN_POINT ( 'NONE',  ( 5.796264663052079769, -21.44337444023769379, -1.500000000000002220 ) ) ;
#60924 = CARTESIAN_POINT ( 'NONE',  ( -0.003042231299257275486, -20.61035990087709635, 11.49999999999998934 ) ) ;
#60925 = EDGE_CURVE ( 'NONE', #100062, #1418, #88670, .T. ) ;
#60926 = B_SPLINE_CURVE_WITH_KNOTS ( 'NONE', 3,
 ( #95368, #39581, #55825, #86257 ),
 .UNSPECIFIED., .F., .F.,
 ( 4, 4 ),
 ( 0.8103645859926805750, 0.8193710172647959977 ),
 .UNSPECIFIED. ) ;
#60927 = ORIENTED_EDGE ( 'NONE', *, *, #8404, .T. ) ;
#60928 = ORIENTED_EDGE ( 'NONE', *, *, #51844, .T. ) ;
#60929 = CARTESIAN_POINT ( 'NONE',  ( -4.537657931416015700, -5.876774720514410077, 19.25713806424188235 ) ) ;
#60930 = CARTESIAN_POINT ( 'NONE',  ( 3.474198977381013798, -5.876774720514426065, 21.79108561604954986 ) ) ;
#60931 = EDGE_LOOP ( 'NONE', ( #9782, #84647, #33838, #29056 ) ) ;
#60932 = ORIENTED_EDGE ( 'NONE', *, *, #22244, .F. ) ;
#60933 = CARTESIAN_POINT ( 'NONE',  ( -124.7735416517568723, -25.27125674707836822, 4.078964885054434220 ) ) ;
#60934 = DIRECTION ( 'NONE',  ( 0.000000000000000000, 2.173523156925980399E-06, -0.9999999999976378895 ) ) ;
#60935 = CARTESIAN_POINT ( 'NONE',  ( 20.25184064777635484, 4.944226511633750043, -1.500000000000002220 ) ) ;
#60936 = CARTESIAN_POINT ( 'NONE',  ( -11.04117723084791614, -18.81814233335528286, 11.49999999999999645 ) ) ;
#60937 = DIRECTION ( 'NONE',  ( 8.334928612639484546E-17, 1.000000000000000000, 7.321843366904296032E-17 ) ) ;
#60938 = CARTESIAN_POINT ( 'NONE',  ( -78.62655469335055614, -24.51419770103157347, 9.386484678747175181 ) ) ;
#60939 = CARTESIAN_POINT ( 'NONE',  ( 19.77452139984142221, -10.64395493966388706, 11.49999999999998934 ) ) ;
#60940 = VECTOR ( 'NONE', #43903, 1000.000000000000000 ) ;
#60941 = EDGE_CURVE ( 'NONE', #94742, #82156, #28243, .T. ) ;
#60942 = DIRECTION ( 'NONE',  ( 0.000000000000000000, 0.000000000000000000, 1.000000000000000000 ) ) ;
#60943 = VERTEX_POINT ( 'NONE', #90638 ) ;
#60944 = DIRECTION ( 'NONE',  ( 0.000000000000000000, 0.000000000000000000, -1.000000000000000000 ) ) ;
#60945 = PLANE ( 'NONE',  #16699 ) ;
#60946 = ORIENTED_EDGE ( 'NONE', *, *, #17143, .T. ) ;
#60947 = ORIENTED_EDGE ( 'NONE', *, *, #38419, .F. ) ;
#60948 = EDGE_CURVE ( 'NONE', #35163, #23209, #62199, .T. ) ;
#60949 = DIRECTION ( 'NONE',  ( 1.000000000000000000, 3.773278334444166432E-23, 8.201307841325785021E-29 ) ) ;
#60950 = VERTEX_POINT ( 'NONE', #47968 ) ;
#60951 = VECTOR ( 'NONE', #80992, 1000.000000000000227 ) ;
#60952 = CARTESIAN_POINT ( 'NONE',  ( 5.124585555570928541, 20.71496159572455653, -1.500000000000002220 ) ) ;
#60953 = ORIENTED_EDGE ( 'NONE', *, *, #92946, .T. ) ;
#60954 = AXIS2_PLACEMENT_3D ( 'NONE', #78128, #46711, #61439 ) ;
#60955 = CARTESIAN_POINT ( 'NONE',  ( -9.798014431990228701, 18.61115389415964572, -1.500000000000002220 ) ) ;
#60956 = FACE_OUTER_BOUND ( 'NONE', #81127, .T. ) ;
#60957 = CARTESIAN_POINT ( 'NONE',  ( -111.1735661057252145, -25.24499744434313442, 3.690036886848450770 ) ) ;
#60958 = AXIS2_PLACEMENT_3D ( 'NONE', #33035, #7809, #49777 ) ;
#60959 = CARTESIAN_POINT ( 'NONE',  ( 6.881670032588234953, -3.316774720514422903, -27.26384557944684062 ) ) ;
#60960 = CARTESIAN_POINT ( 'NONE',  ( -3.625624329714521643, -21.66436044012089468, -1.500000000000002220 ) ) ;
#60961 = CARTESIAN_POINT ( 'NONE',  ( -87.55456245514183422, -23.96119346886881729, -0.6495511937831870419 ) ) ;
#60962 = ORIENTED_EDGE ( 'NONE', *, *, #49163, .F. ) ;
#60963 = LINE ( 'NONE', #23874, #85906 ) ;
#60964 = B_SPLINE_CURVE_WITH_KNOTS ( 'NONE', 3,
 ( #25820, #26322, #11092, #56292 ),
 .UNSPECIFIED., .F., .F.,
 ( 4, 4 ),
 ( 0.000000000000000000, 9.999999999998897304E-05 ),
 .UNSPECIFIED. ) ;
#60965 = AXIS2_PLACEMENT_3D ( 'NONE', #98905, #45142, #68965 ) ;
#60966 = AXIS2_PLACEMENT_3D ( 'NONE', #729, #63657, #9339 ) ;
#60967 = CARTESIAN_POINT ( 'NONE',  ( -84.50374581864701895, -24.51419770103157347, 9.386484678747175181 ) ) ;
#60968 = DIRECTION ( 'NONE',  ( -3.773278334453079618E-23, 0.9999999999976377785, 2.173523156925979975E-06 ) ) ;
#60969 = CARTESIAN_POINT ( 'NONE',  ( -20.42746634971195974, -23.78597006378213408, 9.174899246800713115 ) ) ;
#60970 = CARTESIAN_POINT ( 'NONE',  ( 7.794017451908327843, -19.83292067980804774, -1.500000000000002220 ) ) ;
#60971 = CARTESIAN_POINT ( 'NONE',  ( -98.51384325196762859, -24.15620529776628445, 10.23563542870660292 ) ) ;
#60972 = CARTESIAN_POINT ( 'NONE',  ( 31.99559323149412648, -3.570691370340881576, -11.82294999027247862 ) ) ;
#60973 = PLANE ( 'NONE',  #56826 ) ;
#60974 = CARTESIAN_POINT ( 'NONE',  ( -33.52200586597940912, -23.48783264082477729, -1.443836473390078146 ) ) ;
#60975 = CARTESIAN_POINT ( 'NONE',  ( -22.07377061809603092, 4.253497373390751513, -1.500000000000002220 ) ) ;
#60976 = CARTESIAN_POINT ( 'NONE',  ( -108.8772486938376289, -25.21970293610405633, 6.713732480141158199 ) ) ;
#60977 = VERTEX_POINT ( 'NONE', #30735 ) ;
#60978 = DIRECTION ( 'NONE',  ( 0.000000000000000000, 0.000000000000000000, 1.000000000000000000 ) ) ;
#60979 = CARTESIAN_POINT ( 'NONE',  ( -19.37001648656083574, -3.113731218521536004, 11.49999999999999645 ) ) ;
#60980 = CARTESIAN_POINT ( 'NONE',  ( -68.62287095715001328, -24.33832256526968862, 0.1851278514119885088 ) ) ;
#60981 = FACE_OUTER_BOUND ( 'NONE', #82120, .T. ) ;
#60982 = EDGE_LOOP ( 'NONE', ( #17593, #71541, #35254, #93644 ) ) ;
#60983 = DIRECTION ( 'NONE',  ( -3.773278334453079618E-23, 0.9999999999976377785, 2.173523156925979975E-06 ) ) ;
#60984 = CARTESIAN_POINT ( 'NONE',  ( -84.52287095715006160, -23.47593901973090524, -1.443836447538996648 ) ) ;
#60985 = CARTESIAN_POINT ( 'NONE',  ( -124.5194944430484014, -24.66019654487200441, 8.947790411086108620 ) ) ;
#60986 = AXIS2_PLACEMENT_3D ( 'NONE', #46966, #30226, #8393 ) ;
#60987 = CARTESIAN_POINT ( 'NONE',  ( 16.26279755680690542, 1.684774720514426560, -27.67997040356620531 ) ) ;
#60988 = CARTESIAN_POINT ( 'NONE',  ( -19.65353550717971487, 1.628721094194526486, 11.49999999999998934 ) ) ;
#60989 = ORIENTED_EDGE ( 'NONE', *, *, #12416, .T. ) ;
#60990 = CARTESIAN_POINT ( 'NONE',  ( 9.196673285530609476, 6.376774720514424288, -25.00509208784493964 ) ) ;
#60991 = FACE_OUTER_BOUND ( 'NONE', #77773, .T. ) ;
#60992 = APPROVAL_STATUS ( 'not_yet_approved' ) ;
#60993 = EDGE_LOOP ( 'NONE', ( #46406, #55938, #11990, #95111 ) ) ;
#60994 = CARTESIAN_POINT ( 'NONE',  ( -47.62287095715004170, -24.65952944569304250, 1.056160979905693686 ) ) ;
#60995 = CARTESIAN_POINT ( 'NONE',  ( -69.62287095715005592, -24.66019654487199020, 8.947790411086131712 ) ) ;
#60996 = CARTESIAN_POINT ( 'NONE',  ( -13.57581083383197296, -6.376774720514426953, 19.78786796564403616 ) ) ;
#60997 = CARTESIAN_POINT ( 'NONE',  ( -66.52287095715007581, -23.47593901973090524, -1.443836447538997092 ) ) ;
#60998 = PLANE ( 'NONE',  #87389 ) ;
#60999 = ADVANCED_FACE ( 'NONE', ( #93122 ), #96481, .F. ) ;
#61000 = B_SPLINE_CURVE_WITH_KNOTS ( 'NONE', 3,
 ( #18550, #40891, #49522, #80454 ),
 .UNSPECIFIED., .F., .F.,
 ( 4, 4 ),
 ( 0.000000000000000000, 9.999999999998897304E-05 ),
 .UNSPECIFIED. ) ;
#61001 = CARTESIAN_POINT ( 'NONE',  ( -95.52287095715006160, -23.47596703998600631, 11.44779298504228215 ) ) ;
#61002 = EDGE_CURVE ( 'NONE', #68689, #79343, #61105, .T. ) ;
#61003 = CARTESIAN_POINT ( 'NONE',  ( -107.5594696158587595, -23.48783264082479505, -1.443836473390060826 ) ) ;
#61004 = CARTESIAN_POINT ( 'NONE',  ( -17.55682386033230102, 9.526633247210019917, -1.500000000000002220 ) ) ;
#61005 = EDGE_CURVE ( 'NONE', #89308, #8902, #77889, .T. ) ;
#61006 = CARTESIAN_POINT ( 'NONE',  ( -125.6228709571500843, -25.00182538069146432, 7.747789668545100206 ) ) ;
#61007 = CARTESIAN_POINT ( 'NONE',  ( -45.49983799985675148, -24.15602025860896163, 10.28564288303535434 ) ) ;
#61008 = ORIENTED_EDGE ( 'NONE', *, *, #81264, .T. ) ;
#61009 = ADVANCED_FACE ( 'NONE', ( #31736 ), #7387, .T. ) ;
#61010 = AXIS2_PLACEMENT_3D ( 'NONE', #25150, #95175, #1333 ) ;
#61011 = CARTESIAN_POINT ( 'NONE',  ( 6.672787727097600374, -5.349622116134226779, -25.44584804566076031 ) ) ;
#61012 = CARTESIAN_POINT ( 'NONE',  ( 18.72495633783376334, -0.5000000000000000000, -1.691563534834430227 ) ) ;
#61013 = DIRECTION ( 'NONE',  ( 0.000000000000000000, 0.000000000000000000, -1.000000000000000000 ) ) ;
#61014 = CARTESIAN_POINT ( 'NONE',  ( -39.49146858854847864, -24.34968618360933235, 0.1864209137778788106 ) ) ;
#61015 = CARTESIAN_POINT ( 'NONE',  ( 25.61870917940689552, -5.965225279485572685, 28.79814474876421926 ) ) ;
#61016 = CARTESIAN_POINT ( 'NONE',  ( -51.09576285965076181, -25.31574456684156615, 4.912418940310026017 ) ) ;
#61017 = CARTESIAN_POINT ( 'NONE',  ( -64.62287095715002749, -23.73907113216990084, -1.053371485793233475 ) ) ;
#61018 = EDGE_CURVE ( 'NONE', #71823, #54115, #39843, .T. ) ;
#61020 = VECTOR ( 'NONE', #62305, 1000.000000000000000 ) ;
#61019 = DIRECTION ( 'NONE',  ( -3.773278334453079618E-23, 0.9999999999976377785, 2.173523156925979975E-06 ) ) ;
#61021 = ORIENTED_EDGE ( 'NONE', *, *, #39827, .T. ) ;
#61022 = VECTOR ( 'NONE', #87377, 1000.000000000000000 ) ;
#61023 = CARTESIAN_POINT ( 'NONE',  ( -12.21837793623082113, -16.16665877782589433, 11.49999999999998934 ) ) ;
#61024 = CARTESIAN_POINT ( 'NONE',  ( -122.6234929783657890, -24.65952944569305316, 1.056160979905708786 ) ) ;
#61025 = CARTESIAN_POINT ( 'NONE',  ( 21.48823513768370574, 4.361976414099077992, -16.63192637262848450 ) ) ;
#61026 = AXIS2_PLACEMENT_3D ( 'NONE', #75842, #60647, #28683 ) ;
#61027 = CARTESIAN_POINT ( 'NONE',  ( -90.52287095715009002, -24.62226745350443480, 0.9660975649729555137 ) ) ;
#61028 = ORIENTED_EDGE ( 'NONE', *, *, #69043, .T. ) ;
#61029 = DIRECTION ( 'NONE',  ( -3.773278334444167608E-23, 1.000000000000000000, 0.000000000000000000 ) ) ;
#61030 = LINE ( 'NONE', #17731, #34064 ) ;
#61031 = CARTESIAN_POINT ( 'NONE',  ( 18.22116949570664701, -8.484823103377051368, -1.500000000000002220 ) ) ;
#61032 = CARTESIAN_POINT ( 'NONE',  ( -13.06023916655064276, -16.53025015627232719, 11.49999999999999645 ) ) ;
#61033 = B_SPLINE_CURVE_WITH_KNOTS ( 'NONE', 3,
 ( #80005, #80507, #18112, #85742, #79506, #9994 ),
 .UNSPECIFIED., .F., .F.,
 ( 4, 2, 4 ),
 ( 1.570755371633954459E-05, 0.001396183895866086669, 0.002776660238015833844 ),
 .UNSPECIFIED. ) ;
#61034 = CARTESIAN_POINT ( 'NONE',  ( -99.58953762381672448, -24.64965694238407323, 8.947790433994651238 ) ) ;
#61035 = CARTESIAN_POINT ( 'NONE',  ( -2.366842300981895519, -21.98859952056468714, 11.49999999999998934 ) ) ;
#61036 = CARTESIAN_POINT ( 'NONE',  ( 16.23509277041898358, 12.58620111108425377, 11.49999999999998934 ) ) ;
#61037 = DIRECTION ( 'NONE',  ( -0.000000000000000000, 1.000000000000000000, -0.000000000000000000 ) ) ;
#61038 = VERTEX_POINT ( 'NONE', #17002 ) ;
#61039 = CARTESIAN_POINT ( 'NONE',  ( 3.750000000000001332, 25.69999999999999574, 0.000000000000000000 ) ) ;
#61040 = ORIENTED_EDGE ( 'NONE', *, *, #16430, .F. ) ;
#61041 = CARTESIAN_POINT ( 'NONE',  ( -82.92287095715005307, -23.47596703998600631, 11.44779298504227860 ) ) ;
#61042 = B_SPLINE_CURVE_WITH_KNOTS ( 'NONE', 3,
 ( #76038, #6039, #91764, #45119, #82663, #83156, #36991, #45612 ),
 .UNSPECIFIED., .F., .F.,
 ( 4, 2, 2, 4 ),
 ( 6.384118678612463891E-06, 0.002007151183507257554, 0.003007534715921580341, 0.004007918248335903127 ),
 .UNSPECIFIED. ) ;
#61043 = FACE_OUTER_BOUND ( 'NONE', #24710, .T. ) ;
#61044 = EDGE_LOOP ( 'NONE', ( #26646, #740, #56940, #24947 ) ) ;
#61045 = ORIENTED_EDGE ( 'NONE', *, *, #6760, .T. ) ;
#61046 = ORIENTED_EDGE ( 'NONE', *, *, #46217, .F. ) ;
#61047 = PLANE ( 'NONE',  #38888 ) ;
#61048 = CARTESIAN_POINT ( 'NONE',  ( -71.62287095715005592, -23.47596703998600631, 11.44779298504227683 ) ) ;
#61049 = CARTESIAN_POINT ( 'NONE',  ( -28.52287095715005805, -29.50250786944459946, 11.44777958301664356 ) ) ;
#61050 = CARTESIAN_POINT ( 'NONE',  ( -20.60669311552257810, 0.8253496925510150906, -1.500000000000002220 ) ) ;
#61051 = CARTESIAN_POINT ( 'NONE',  ( 15.46703529437019853, -15.08741104398349187, 11.49999999999999645 ) ) ;
#61052 = VERTEX_POINT ( 'NONE', #1791 ) ;
#61053 = CARTESIAN_POINT ( 'NONE',  ( -46.52287095715006160, -24.64965694238406613, 8.947790433994203596 ) ) ;
#61054 = EDGE_CURVE ( 'NONE', #58570, #72031, #78937, .T. ) ;
#61055 = VECTOR ( 'NONE', #36715, 1000.000000000000114 ) ;
#61056 = LINE ( 'NONE', #22951, #18855 ) ;
#61057 = CARTESIAN_POINT ( 'NONE',  ( -22.26391555059773353, 2.265117081278330780, -1.500000000000002220 ) ) ;
#61058 = CARTESIAN_POINT ( 'NONE',  ( -34.52287095715006160, -24.35013146730202749, 9.818937971375103047 ) ) ;
#61059 = CARTESIAN_POINT ( 'NONE',  ( -84.52214531569265432, -23.48783264082476308, -1.443836473390094799 ) ) ;
#61060 = VERTEX_POINT ( 'NONE', #53594 ) ;
#61061 = B_SPLINE_CURVE_WITH_KNOTS ( 'NONE', 3,
 ( #90276, #29870, #67951, #12645 ),
 .UNSPECIFIED., .F., .F.,
 ( 4, 4 ),
 ( 4.163336342344337027E-17, 9.999999999997512235E-05 ),
 .UNSPECIFIED. ) ;
#61062 = CARTESIAN_POINT ( 'NONE',  ( -100.0601433209239133, -25.31017654890569801, 4.635600862196024963 ) ) ;
#61063 = CARTESIAN_POINT ( 'NONE',  ( -35.62380681592568266, -25.00182538069146787, 7.747789668545037145 ) ) ;
#61064 = CIRCLE ( 'NONE', #52950, 1.699999999999999289 ) ;
#61065 = CARTESIAN_POINT ( 'NONE',  ( -3.950822543831816080, -20.53616823614468956, 11.49999999999998934 ) ) ;
#61066 = ORIENTED_EDGE ( 'NONE', *, *, #32875, .F. ) ;
#61067 = ADVANCED_FACE ( 'NONE', ( #9892 ), #87529, .F. ) ;
#61069 = ORIENTED_EDGE ( 'NONE', *, *, #25140, .T. ) ;
#61068 = CARTESIAN_POINT ( 'NONE',  ( -67.64622146058944452, -23.73791477778911840, 11.05961554403170766 ) ) ;
#61070 = ORIENTED_EDGE ( 'NONE', *, *, #44163, .F. ) ;
#61071 = CARTESIAN_POINT ( 'NONE',  ( -50.62287095715007723, -24.91570333823099759, 8.075032458375556388 ) ) ;
#61072 = CARTESIAN_POINT ( 'NONE',  ( 19.29917393477590437, 8.764703196630867055, -1.500000000000002220 ) ) ;
#61073 = ORIENTED_EDGE ( 'NONE', *, *, #51492, .F. ) ;
#61074 = LINE ( 'NONE', #52959, #31681 ) ;
#61075 = CARTESIAN_POINT ( 'NONE',  ( 0.000000000000000000, 0.3849999999999945688, 1.530000000000001359 ) ) ;
#61076 = CARTESIAN_POINT ( 'NONE',  ( 21.67628855941699939, -2.339797445609365756, 11.49999999999998934 ) ) ;
#61077 = DIRECTION ( 'NONE',  ( 0.000000000000000000, -2.173523156925980399E-06, 0.9999999999976378895 ) ) ;
#61078 = CARTESIAN_POINT ( 'NONE',  ( -36.62287095715004881, -24.33832256527048088, 0.1851278514138546272 ) ) ;
#61079 = CARTESIAN_POINT ( 'NONE',  ( 7.477175500793984853, -5.876774720514417183, 20.66439772633092176 ) ) ;
#61080 = CARTESIAN_POINT ( 'NONE',  ( 19.96715809174937561, -8.635335823514383335, -1.500000000000002220 ) ) ;
#61081 = CARTESIAN_POINT ( 'NONE',  ( -0.9257915630711897048, -6.376774720514408301, 19.25892998154168012 ) ) ;
#61083 = ORIENTED_EDGE ( 'NONE', *, *, #89415, .F. ) ;
#61082 = CARTESIAN_POINT ( 'NONE',  ( 8.793911523065595759, -20.50603677605392150, 11.49999999999999645 ) ) ;
#61084 = CARTESIAN_POINT ( 'NONE',  ( -33.52287095715004739, -24.34917612407030063, 0.1852690917476907950 ) ) ;
#61085 = DIRECTION ( 'NONE',  ( 0.000000000000000000, -0.000000000000000000, -1.000000000000000000 ) ) ;
#61086 = CARTESIAN_POINT ( 'NONE',  ( -56.62287095715005592, -29.50250243563736774, 8.947779886222145151 ) ) ;
#61087 = VERTEX_POINT ( 'NONE', #10394 ) ;
#61088 = AXIS2_PLACEMENT_3D ( 'NONE', #56865, #18769, #49751 ) ;
#61089 = ORIENTED_EDGE ( 'NONE', *, *, #97827, .T. ) ;
#61090 = ORIENTED_EDGE ( 'NONE', *, *, #41062, .F. ) ;
#61091 = LINE ( 'NONE', #45857, #85376 ) ;
#61092 = CARTESIAN_POINT ( 'NONE',  ( 15.88363568188429653, -14.04911357082368006, -1.500000000000002220 ) ) ;
#61093 = DIRECTION ( 'NONE',  ( 0.7071067811865476838, 0.000000000000000000, -0.7071067811865474617 ) ) ;
#61094 = CARTESIAN_POINT ( 'NONE',  ( -80.47485683444980964, -25.27791972877900406, 7.562833136764695929 ) ) ;
#61095 = CARTESIAN_POINT ( 'NONE',  ( 22.33191539159863481, -4.132774720514426292, -16.26852658953813346 ) ) ;
#61096 = CIRCLE ( 'NONE', #1113, 1.325999999999943446 ) ;
#61097 = DIRECTION ( 'NONE',  ( -3.773278334453080206E-23, 0.9999999999976377785, 2.173523156925979975E-06 ) ) ;
#61098 = B_SPLINE_CURVE_WITH_KNOTS ( 'NONE', 3,
 ( #36210, #21952, #43331, #4761, #52937, #67174 ),
 .UNSPECIFIED., .F., .F.,
 ( 4, 2, 4 ),
 ( 1.570755371633797249E-05, 0.001396183895866087536, 0.002776660238015836880 ),
 .UNSPECIFIED. ) ;
#61099 = CARTESIAN_POINT ( 'NONE',  ( -5.798782886354239885, 18.49141925852020663, 11.49999999999998934 ) ) ;
#61100 = CARTESIAN_POINT ( 'NONE',  ( -45.61118087450132919, -23.85016227208580375, -0.8807180028928391913 ) ) ;
#61101 = VERTEX_POINT ( 'NONE', #40843 ) ;
#61102 = VECTOR ( 'NONE', #91629, 1000.000000000000000 ) ;
#61103 = CARTESIAN_POINT ( 'NONE',  ( -5.694372300836820777, 18.57635362771370424, 11.49999999999999645 ) ) ;
#61104 = DIRECTION ( 'NONE',  ( -0.000000000000000000, -1.000000000000000000, -0.000000000000000000 ) ) ;
#61105 = CIRCLE ( 'NONE', #54578, 1.699999999999999289 ) ;
#61106 = ORIENTED_EDGE ( 'NONE', *, *, #29511, .T. ) ;
#61107 = CARTESIAN_POINT ( 'NONE',  ( -78.55620429048340725, -23.47596703998600276, 11.44779298504227683 ) ) ;
#61108 = CARTESIAN_POINT ( 'NONE',  ( 32.53135143123563466, 5.965225279485572685, 6.926385399448451885 ) ) ;
#61109 = CARTESIAN_POINT ( 'NONE',  ( -121.5228709571500616, -23.47596703998600631, 11.44779298504227860 ) ) ;
#61110 = EDGE_CURVE ( 'NONE', #58493, #72155, #80027, .T. ) ;
#61111 = CARTESIAN_POINT ( 'NONE',  ( -19.61951575358169819, -0.1233725505697131491, -1.500000000000002220 ) ) ;
#61112 = FACE_OUTER_BOUND ( 'NONE', #95477, .T. ) ;
#61113 = ORIENTED_EDGE ( 'NONE', *, *, #29999, .F. ) ;
#61114 = CARTESIAN_POINT ( 'NONE',  ( 21.48638754631891246, 1.654510534108022179, 11.49999999999998934 ) ) ;
#61115 = CARTESIAN_POINT ( 'NONE',  ( -33.54540960989195497, -24.15620529776627379, 10.23563542870661536 ) ) ;
#61116 = CARTESIAN_POINT ( 'NONE',  ( 32.98733314340959311, 0.3587747205144265483, 2.074222136288530027 ) ) ;
#61117 = LINE ( 'NONE', #43890, #56958 ) ;
#61118 = CARTESIAN_POINT ( 'NONE',  ( 11.92049557817732364, -19.74369927386287671, -1.500000000000002220 ) ) ;
#61119 = B_SPLINE_CURVE_WITH_KNOTS ( 'NONE', 3,
 ( #64353, #73443, #79543, #10033, #18144, #3937 ),
 .UNSPECIFIED., .F., .F.,
 ( 4, 2, 4 ),
 ( 6.391158118967745954E-06, 0.001387004593080787230, 0.002767618028042606766 ),
 .UNSPECIFIED. ) ;
#61120 = B_SPLINE_CURVE_WITH_KNOTS ( 'NONE', 3,
 ( #60805, #15604, #52182, #75998, #46568, #91232 ),
 .UNSPECIFIED., .F., .F.,
 ( 4, 2, 4 ),
 ( 0.000000000000000000, 0.001380901958385391580, 0.002761803916770783161 ),
 .UNSPECIFIED. ) ;
#61121 = PERSON_AND_ORGANIZATION_ROLE ( 'classification_officer' ) ;
#61122 = DIRECTION ( 'NONE',  ( -0.000000000000000000, -1.000000000000000000, -0.000000000000000000 ) ) ;
#61123 = CARTESIAN_POINT ( 'NONE',  ( -50.70339841325804997, -25.29249258120279009, 4.255736650380444352 ) ) ;
#61124 = CARTESIAN_POINT ( 'NONE',  ( 14.71488472389458124, -13.84269218943631508, 11.49999999999999645 ) ) ;
#61125 = CARTESIAN_POINT ( 'NONE',  ( -121.6245712669088732, -24.35071581493543391, 9.817618358456025263 ) ) ;
#61126 = CARTESIAN_POINT ( 'NONE',  ( -91.52287095715006160, -24.51283580621365488, 0.6167428607019749265 ) ) ;
#61127 = EDGE_CURVE ( 'NONE', #18110, #85110, #57590, .T. ) ;
#61128 = CARTESIAN_POINT ( 'NONE',  ( -111.7788625685672486, -25.10921688335350055, 4.278827964032922537 ) ) ;
#61129 = DIRECTION ( 'NONE',  ( -2.439088438507244272E-15, -0.000000000000000000, -1.000000000000000000 ) ) ;
#61130 = B_SPLINE_CURVE_WITH_KNOTS ( 'NONE', 3,
 ( #4184, #43250, #42269, #66107, #65604, #27017 ),
 .UNSPECIFIED., .F., .F.,
 ( 4, 2, 4 ),
 ( 1.437692738331097786, 1.447547036373233009, 1.457401334415368233 ),
 .UNSPECIFIED. ) ;
#61131 = CARTESIAN_POINT ( 'NONE',  ( -110.9011049686103263, -25.29779188398908829, 3.445933212628501163 ) ) ;
#61132 = CARTESIAN_POINT ( 'NONE',  ( 17.57725459251073019, -9.329341740261039462, 11.49999999999998934 ) ) ;
#61133 = ADVANCED_FACE ( 'NONE', ( #18009 ), #72808, .T. ) ;
#61134 = CARTESIAN_POINT ( 'NONE',  ( -79.11611000704998276, -25.16711686381824720, 3.101159594853582835 ) ) ;
#61135 = CARTESIAN_POINT ( 'NONE',  ( 0.5484783294719396407, -19.75002165935583776, -1.500000000000002220 ) ) ;
#61136 = CIRCLE ( 'NONE', #51415, 0.8160000000000000586 ) ;
#61137 = CARTESIAN_POINT ( 'NONE',  ( -56.65737350661340344, -23.48783264082477018, -1.443836473390095909 ) ) ;
#61138 = ADVANCED_FACE ( 'NONE', ( #33739 ), #56594, .T. ) ;
#61139 = ADVANCED_FACE ( 'NONE', ( #17509 ), #63713, .F. ) ;
#61140 = PLANE ( 'NONE',  #64652 ) ;
#61141 = LINE ( 'NONE', #59644, #88063 ) ;
#61142 = CARTESIAN_POINT ( 'NONE',  ( 17.27521350410721368, -11.31798593588896829, 11.49999999999999645 ) ) ;
#61143 = VECTOR ( 'NONE', #71837, 1000.000000000000114 ) ;
#61144 = LINE ( 'NONE', #38278, #95358 ) ;
#61145 = ADVANCED_FACE ( 'NONE', ( #88527 ), #42565, .T. ) ;
#61146 = B_SPLINE_CURVE_WITH_KNOTS ( 'NONE', 3,
 ( #25184, #40424, #59518, #63785, #79976, #71381 ),
 .UNSPECIFIED., .F., .F.,
 ( 4, 2, 4 ),
 ( 0.000000000000000000, 0.001380901958385385509, 0.002761803916770771018 ),
 .UNSPECIFIED. ) ;
#61147 = CARTESIAN_POINT ( 'NONE',  ( -119.6228709571500559, -29.50250243563736774, 8.947779886222134493 ) ) ;
#61148 = CARTESIAN_POINT ( 'NONE',  ( 9.008567143757492346, 20.83016157428379955, 11.49999999999999645 ) ) ;
#61149 = ORIENTED_EDGE ( 'NONE', *, *, #32860, .F. ) ;
#61150 = B_SPLINE_SURFACE_WITH_KNOTS ( 'NONE', 3, 1, ( 
 ( #84927, #93530 ),
 ( #70213, #84429 ),
 ( #93032, #62609 ),
 ( #24026, #76798 ),
 ( #30645, #45882 ),
 ( #68718, #23510 ),
 ( #78308, #99634 ),
 ( #54995, #92536 ),
 ( #85935, #30138 ),
 ( #39750, #53506 ),
 ( #70710, #7298 ),
 ( #38250, #23009 ),
 ( #28469, #36092 ),
 ( #69035, #43708 ),
 ( #37588, #5635 ),
 ( #75145, #91368 ),
 ( #36581, #21843 ),
 ( #68539, #51320 ),
 ( #59434, #14233 ) ),
 .UNSPECIFIED., .F., .F., .F.,
 ( 4, 1, 1, 1, 1, 1, 1, 1, 1, 1, 1, 1, 1, 1, 1, 1, 4 ),
 ( 2, 2 ),
 ( 0.000000000000000000, 0.05953958549708775888, 0.1174229600021179099, 0.1744404410469199418, 0.2317338905564219620, 0.2897219772859587206, 0.3492003964486030121, 0.4105155317344490462, 0.4750802789743625576, 0.5400944754761672906, 0.6044440959297832094, 0.6686966743402348312, 0.7321102011010777177, 0.7967393467417489550, 0.8629057297096498491, 0.9304616390764175460, 0.9999999999999998890 ),
 ( 0.000000000000000000, 1.000000000000000000 ),
 .UNSPECIFIED. ) ;
#61151 = DIRECTION ( 'NONE',  ( 3.773278334444167608E-23, -1.000000000000000000, 0.000000000000000000 ) ) ;
#61152 = CARTESIAN_POINT ( 'NONE',  ( -33.62287095715005592, -24.66019654487199020, 8.947790411086138818 ) ) ;
#61153 = CARTESIAN_POINT ( 'NONE',  ( 8.007726535620864894, 18.53121347637897287, -1.500000000000002220 ) ) ;
#61154 = EDGE_CURVE ( 'NONE', #59202, #14898, #67199, .T. ) ;
#61155 = CARTESIAN_POINT ( 'NONE',  ( -111.7814946224345789, -25.29712067403330877, 4.332404411321261861 ) ) ;
#61156 = B_SPLINE_CURVE_WITH_KNOTS ( 'NONE', 3,
 ( #53928, #23956, #7737, #54923, #84859, #38683 ),
 .UNSPECIFIED., .F., .F.,
 ( 4, 2, 4 ),
 ( 0.000000000000000000, 0.001380764517854763014, 0.002761529035709526028 ),
 .UNSPECIFIED. ) ;
#61157 = CARTESIAN_POINT ( 'NONE',  ( 9.278253834636469577, -5.876774720514426953, 18.51871304725684553 ) ) ;
#61158 = ORIENTED_EDGE ( 'NONE', *, *, #54752, .T. ) ;
#61159 = CIRCLE ( 'NONE', #20570, 2.999999999999999112 ) ;
#61160 = B_SPLINE_CURVE_WITH_KNOTS ( 'NONE', 3,
 ( #95657, #73326, #80930, #81926, #72325, #57608 ),
 .UNSPECIFIED., .F., .F.,
 ( 4, 2, 4 ),
 ( 1.570755371634150632E-05, 0.001396183895866087319, 0.002776660238015833410 ),
 .UNSPECIFIED. ) ;
#61161 = ORIENTED_EDGE ( 'NONE', *, *, #26653, .T. ) ;
#61162 = CARTESIAN_POINT ( 'NONE',  ( 0.3670296583442628213, -5.876774720514417183, 20.26087634804755311 ) ) ;
#61163 = CARTESIAN_POINT ( 'NONE',  ( 21.13568926591755925, -8.834425160694816981, 11.49999999999998934 ) ) ;
#61164 = CARTESIAN_POINT ( 'NONE',  ( -8.160000000000000142, -10.65233964170348635, 1.628518864987183790 ) ) ;
#61165 = CARTESIAN_POINT ( 'NONE',  ( 19.51036611237648088, 9.378288983258578071, -1.500000000000002220 ) ) ;
#61166 = DIRECTION ( 'NONE',  ( -3.773278334444167608E-23, 1.000000000000000000, 0.000000000000000000 ) ) ;
#61167 = DIRECTION ( 'NONE',  ( 0.000000000000000000, -2.173523156925980399E-06, 0.9999999999976378895 ) ) ;
#61168 = CARTESIAN_POINT ( 'NONE',  ( -16.13976855045889636, 13.32451261336467496, 11.49999999999999645 ) ) ;
#61169 = ORIENTED_EDGE ( 'NONE', *, *, #42014, .T. ) ;
#61170 = CARTESIAN_POINT ( 'NONE',  ( -124.5904483378009218, -23.96119346886880308, -0.6495511937832024740 ) ) ;
#61171 = CARTESIAN_POINT ( 'NONE',  ( -15.57331531552114612, -15.56871402003811333, 11.49999999999998934 ) ) ;
#61172 = CIRCLE ( 'NONE', #12551, 251.4258649670780699 ) ;
#61173 = CARTESIAN_POINT ( 'NONE',  ( -105.5884166583201988, -24.63419186844610920, 9.035850630976920428 ) ) ;
#61174 = CARTESIAN_POINT ( 'NONE',  ( -28.66268959117890347, -25.21724901141872976, 7.176256802127888967 ) ) ;
#61175 = ORIENTED_EDGE ( 'NONE', *, *, #26536, .T. ) ;
#61176 = PLANE ( 'NONE',  #28010 ) ;
#61177 = CARTESIAN_POINT ( 'NONE',  ( -90.60546021415382256, -23.48786465467241058, 11.44779295918254824 ) ) ;
#61178 = EDGE_LOOP ( 'NONE', ( #84234, #76070, #63226, #15366 ) ) ;
#61179 = CARTESIAN_POINT ( 'NONE',  ( -72.51646068626162389, -23.73791477778911840, 11.05961554403170943 ) ) ;
#61180 = ORIENTED_EDGE ( 'NONE', *, *, #79430, .F. ) ;
#61181 = VECTOR ( 'NONE', #32375, 1000.000000000000114 ) ;
#61182 = VERTEX_POINT ( 'NONE', #20003 ) ;
#61183 = CARTESIAN_POINT ( 'NONE',  ( -102.6228709571500559, -29.50247984919015209, -1.443849546365050029 ) ) ;
#61184 = CARTESIAN_POINT ( 'NONE',  ( -117.5228709571500758, -24.64965694238408034, 8.947790433994191162 ) ) ;
#61185 = CARTESIAN_POINT ( 'NONE',  ( -100.5228709571500616, -24.82576562948881005, 8.398263436605667209 ) ) ;
#61186 = CARTESIAN_POINT ( 'NONE',  ( 20.39306652673287701, -2.074774109220689500, -1.500000000000002220 ) ) ;
#61187 = EDGE_CURVE ( 'NONE', #29990, #19469, #35170, .T. ) ;
#61188 = VERTEX_POINT ( 'NONE', #13377 ) ;
#61189 = CARTESIAN_POINT ( 'NONE',  ( -3.108974358974359475, -5.876774720514416295, 20.36458333333334281 ) ) ;
#61190 = CARTESIAN_POINT ( 'NONE',  ( -30.61048516611183956, -24.43626637953623160, 0.1835287498755953095 ) ) ;
#61191 = DIRECTION ( 'NONE',  ( -1.895872651340772790E-16, 0.000000000000000000, -1.000000000000000000 ) ) ;
#61192 = CARTESIAN_POINT ( 'NONE',  ( 22.20168578472828358, 1.497490109320031682, 11.49999999999998934 ) ) ;
#61193 = EDGE_CURVE ( 'NONE', #81664, #55675, #5278, .T. ) ;
#61194 = CARTESIAN_POINT ( 'NONE',  ( -98.52287095715006160, -24.65952944569304606, 1.056160979905702346 ) ) ;
#61195 = CARTESIAN_POINT ( 'NONE',  ( -7.686499194032762716, 10.69006800129435497, -0.9352597624345265759 ) ) ;
#61196 = ORIENTED_EDGE ( 'NONE', *, *, #77187, .F. ) ;
#61197 = FACE_OUTER_BOUND ( 'NONE', #51197, .T. ) ;
#61198 = CARTESIAN_POINT ( 'NONE',  ( -28.41099462919338237, -24.63646035822953451, 8.118938870972160160 ) ) ;
#61199 = CARTESIAN_POINT ( 'NONE',  ( 9.628234360240019996, 18.42577530400075858, 11.49999999999998934 ) ) ;
#61200 = EDGE_LOOP ( 'NONE', ( #73171, #72377, #65413, #55487 ) ) ;
#61202 = ORIENTED_EDGE ( 'NONE', *, *, #81532, .T. ) ;
#61201 = CARTESIAN_POINT ( 'NONE',  ( 4.518205171808153509, -6.376774720514406525, 19.05004583296150500 ) ) ;
#61203 = CARTESIAN_POINT ( 'NONE',  ( -31.55620429048339304, -24.65952944569304606, 1.056160979905691688 ) ) ;
#61205 = ORIENTED_EDGE ( 'NONE', *, *, #44755, .T. ) ;
#61204 = EDGE_CURVE ( 'NONE', #56477, #44828, #18382, .T. ) ;
#61206 = ORIENTED_EDGE ( 'NONE', *, *, #91533, .T. ) ;
#61207 = CARTESIAN_POINT ( 'NONE',  ( 7.961587039082260731, 10.40935432823260776, -0.9107004983449004110 ) ) ;
#61208 = DIRECTION ( 'NONE',  ( 0.000000000000000000, 0.9961946980917452121, -0.08715574274766166307 ) ) ;
#61209 = CARTESIAN_POINT ( 'NONE',  ( -116.5120815788254021, -25.30053193007086065, 4.607778174927533499 ) ) ;
#61210 = CARTESIAN_POINT ( 'NONE',  ( -40.62287095715006302, -24.15516710230294350, 10.28746687063726029 ) ) ;
#61211 = CARTESIAN_POINT ( 'NONE',  ( -109.4104630438534542, -25.17367207030539689, 3.148482298596714024 ) ) ;
#61212 = LINE ( 'NONE', #92132, #27052 ) ;
#61214 = EDGE_LOOP ( 'NONE', ( #88792, #97439, #63681, #61695 ) ) ;
#61213 = CARTESIAN_POINT ( 'NONE',  ( 1.014068502963303864, -22.09113584270698993, 11.49999999999999645 ) ) ;
#61215 = EDGE_CURVE ( 'NONE', #41031, #58438, #7402, .T. ) ;
#61216 = CARTESIAN_POINT ( 'NONE',  ( 31.79364159983995464, 6.475225279485573360, -11.59305536555894278 ) ) ;
#61217 = CARTESIAN_POINT ( 'NONE',  ( -15.40814491850785650, 16.58152744545821022, 11.49999999999998934 ) ) ;
#61218 = AXIS2_PLACEMENT_3D ( 'NONE', #94124, #2801, #64719 ) ;
#61220 = VERTEX_POINT ( 'NONE', #21981 ) ;
#61219 = CARTESIAN_POINT ( 'NONE',  ( -29.16552315785632743, -25.14802933280332198, 6.095404567958068398 ) ) ;
#61221 = ORIENTED_EDGE ( 'NONE', *, *, #28732, .F. ) ;
#61222 = CARTESIAN_POINT ( 'NONE',  ( 31.14267748017797288, 4.481735162546534923, -3.047060235321841226 ) ) ;
#61223 = CC_DESIGN_PERSON_AND_ORGANIZATION_ASSIGNMENT ( #54496, #7306, ( #78135 ) ) ;
#61224 = CARTESIAN_POINT ( 'NONE',  ( -2.706554608146168217, 19.95013100808389339, 11.49999999999998934 ) ) ;
#61225 = CARTESIAN_POINT ( 'NONE',  ( -7.160000000000000142, -6.927494035009244411E-16, 6.788828319098143105 ) ) ;
#61226 = VERTEX_POINT ( 'NONE', #21482 ) ;
#61227 = PLANE ( 'NONE',  #9847 ) ;
#61228 = CARTESIAN_POINT ( 'NONE',  ( 16.41691039316204481, 15.16158741987741365, -1.500000000000002220 ) ) ;
#61229 = ORIENTED_EDGE ( 'NONE', *, *, #27996, .F. ) ;
#61230 = ORIENTED_EDGE ( 'NONE', *, *, #41936, .T. ) ;
#61231 = CARTESIAN_POINT ( 'NONE',  ( -34.92287095715007439, -23.47593901973090524, -1.443836447538998646 ) ) ;
#61232 = DIRECTION ( 'NONE',  ( -3.773278334444166432E-23, 1.000000000000000000, 0.000000000000000000 ) ) ;
#61233 = FACE_OUTER_BOUND ( 'NONE', #97414, .T. ) ;
#61234 = DIRECTION ( 'NONE',  ( 0.000000000000000000, -1.000000000000000000, 0.000000000000000000 ) ) ;
#61235 = VECTOR ( 'NONE', #74573, 1000.000000000000000 ) ;
#61236 = CARTESIAN_POINT ( 'NONE',  ( 0.000000000000000000, -1.530000000000000027, 0.3849999999999990652 ) ) ;
#61237 = CARTESIAN_POINT ( 'NONE',  ( 18.00893756148942870, 7.586210683597776949, -1.500000000000002220 ) ) ;
#61238 = CARTESIAN_POINT ( 'NONE',  ( -102.5228709571501042, -23.48783264083375144, -1.443836473376139740 ) ) ;
#61239 = CARTESIAN_POINT ( 'NONE',  ( 1.049947104896167049, -21.43676768134831434, -1.500000000000002220 ) ) ;
#61240 = CARTESIAN_POINT ( 'NONE',  ( -2.283364382221138467, -5.876774720514410077, 19.46427715384223944 ) ) ;
#61241 = CARTESIAN_POINT ( 'NONE',  ( 8.160000000000000142, -10.15233964170348457, 0.003711184059992174607 ) ) ;
#61242 = FACE_OUTER_BOUND ( 'NONE', #9141, .T. ) ;
#61243 = CARTESIAN_POINT ( 'NONE',  ( -17.51315278866654879, 14.73147661606379621, -1.500000000000002220 ) ) ;
#61244 = AXIS2_PLACEMENT_3D ( 'NONE', #31585, #85879, #23967 ) ;
#61245 = COORDINATED_UNIVERSAL_TIME_OFFSET ( 0, 0, .AHEAD. ) ;
#61246 = FACE_OUTER_BOUND ( 'NONE', #48312, .T. ) ;
#61247 = DIRECTION ( 'NONE',  ( -0.000000000000000000, 1.000000000000000000, -0.000000000000000000 ) ) ;
#61248 = CARTESIAN_POINT ( 'NONE',  ( 19.98059151383774434, -0.7942727526097331792, 11.49999999999999645 ) ) ;
#61249 = CARTESIAN_POINT ( 'NONE',  ( -31.62287095715005236, -23.48783264082477729, -1.443836473390074149 ) ) ;
#61250 = AXIS2_PLACEMENT_3D ( 'NONE', #70570, #8173, #77165 ) ;
#61251 = CARTESIAN_POINT ( 'NONE',  ( 4.966983519792414370, -5.876774720514415407, 19.83633487160803099 ) ) ;
#61252 = CARTESIAN_POINT ( 'NONE',  ( 30.73873608389078527, 2.297196155479665158, 24.67598410064776715 ) ) ;
#61253 = ADVANCED_FACE ( 'NONE', ( #20493 ), #66713, .F. ) ;
#61254 = ORIENTED_EDGE ( 'NONE', *, *, #77490, .F. ) ;
#61255 = LINE ( 'NONE', #92177, #31564 ) ;
#61256 = CARTESIAN_POINT ( 'NONE',  ( -70.52287095715007581, -23.48786465467241769, 11.44779295918254647 ) ) ;
#61257 = CARTESIAN_POINT ( 'NONE',  ( -20.56741719582323213, 7.008553436993695485, 11.49999999999998934 ) ) ;
#61258 = CARTESIAN_POINT ( 'NONE',  ( -117.5228709571500758, -23.48783264082477729, -1.443836473390083697 ) ) ;
#61259 = CARTESIAN_POINT ( 'NONE',  ( -2.459534284235005863, 19.42625828800391119, -1.500000000000002220 ) ) ;
#61260 = DIRECTION ( 'NONE',  ( -3.773278334453079618E-23, 0.9999999999976377785, 2.173523156925979975E-06 ) ) ;
#61261 = CARTESIAN_POINT ( 'NONE',  ( -109.6940667814372006, -25.31698119913111000, 5.011372319774925366 ) ) ;
#61262 = COORDINATED_UNIVERSAL_TIME_OFFSET ( 0, 0, .AHEAD. ) ;
#61263 = EDGE_CURVE ( 'NONE', #39813, #24849, #2577, .T. ) ;
#61264 = CARTESIAN_POINT ( 'NONE',  ( -8.160000000000000142, -10.15233964170348457, 0.003711184059992174607 ) ) ;
#61265 = CARTESIAN_POINT ( 'NONE',  ( 3.474198977381013798, -5.876774720514426065, 21.79108561604954986 ) ) ;
#61266 = CARTESIAN_POINT ( 'NONE',  ( -15.16157141410761966, -13.82251119679066953, 11.49999999999999645 ) ) ;
#61267 = CARTESIAN_POINT ( 'NONE',  ( -34.62287095715005592, -29.50247984919015209, -1.443849546365062242 ) ) ;
#61268 = EDGE_CURVE ( 'NONE', #54721, #99816, #76410, .T. ) ;
#61269 = LINE ( 'NONE', #60271, #41635 ) ;
#61270 = ORIENTED_EDGE ( 'NONE', *, *, #3964, .T. ) ;
#61271 =( LENGTH_UNIT ( ) NAMED_UNIT ( * ) SI_UNIT ( .MILLI., .METRE. ) );
#61272 = DIRECTION ( 'NONE',  ( -3.773278334453079030E-23, 0.9999999999976377785, 2.173523156925979128E-06 ) ) ;
#61273 = CARTESIAN_POINT ( 'NONE',  ( 14.76093561896379214, -5.965225279485572685, -26.55548769130089681 ) ) ;
#61274 = CARTESIAN_POINT ( 'NONE',  ( -125.6264018559343754, -23.48786465467241413, 11.44779295918253581 ) ) ;
#61275 = CARTESIAN_POINT ( 'NONE',  ( -85.62287095715001328, -23.85196035786900737, -0.8779234886474913679 ) ) ;
#61276 = EDGE_CURVE ( 'NONE', #56269, #31248, #83894, .T. ) ;
#61277 = CARTESIAN_POINT ( 'NONE',  ( -85.52287095715004739, -24.63287334234178161, 0.9662140553045371894 ) ) ;
#61278 = FACE_OUTER_BOUND ( 'NONE', #22732, .T. ) ;
#61279 = CARTESIAN_POINT ( 'NONE',  ( -23.05830607064937965, -0.9945063503333604338, 11.49999999999999645 ) ) ;
#61280 = CARTESIAN_POINT ( 'NONE',  ( -0.9063223138645676302, -22.79912562917415997, 11.49999999999998934 ) ) ;
#61281 = CARTESIAN_POINT ( 'NONE',  ( -74.56445243665983469, -23.48783264082477018, -1.443836473390096353 ) ) ;
#61282 = B_SPLINE_SURFACE_WITH_KNOTS ( 'NONE', 3, 3, ( 
 ( #9931, #71845, #94666, #31264 ),
 ( #15533, #318, #40885, #46498 ),
 ( #85549, #32767, #77424, #25148 ),
 ( #70840, #55626, #2335, #56128 ),
 ( #62234, #86556, #16032, #46998 ),
 ( #8432, #11433, #95674, #18046 ),
 ( #87559, #42412, #34778, #10938 ) ),
 .UNSPECIFIED., .F., .F., .F.,
 ( 4, 3, 4 ),
 ( 4, 4 ),
 ( 0.0004766839783849497066, 0.1029713700210913990, 0.2054660560637978362 ),
 ( 0.01949895744967442002, 0.02052067878884997545 ),
 .UNSPECIFIED. ) ;
#61283 = CARTESIAN_POINT ( 'NONE',  ( -75.52287095715013265, -24.51254535375842636, 9.355368624242251130 ) ) ;
#61284 = CARTESIAN_POINT ( 'NONE',  ( -5.837039262820512775, -6.376774720514413630, 19.76512419871795245 ) ) ;
#61285 = CARTESIAN_POINT ( 'NONE',  ( -21.98280116189361877, -4.439423430357301470, 11.49999999999999645 ) ) ;
#61286 = CARTESIAN_POINT ( 'NONE',  ( -115.5228709571499905, -24.15431212366390312, -0.2830839119429361395 ) ) ;
#61287 = CARTESIAN_POINT ( 'NONE',  ( -110.5109861788922103, -24.92564183028978775, 1.928384488918252204 ) ) ;
#61288 = CARTESIAN_POINT ( 'NONE',  ( -19.93956527825925917, 9.129326121205059152, 11.49999999999998934 ) ) ;
#61289 = CARTESIAN_POINT ( 'NONE',  ( 32.45853543194704116, -5.965225279485572685, 9.169203677920338080 ) ) ;
#61290 = DIRECTION ( 'NONE',  ( 0.000000000000000000, 0.000000000000000000, 1.000000000000000000 ) ) ;
#61291 = CARTESIAN_POINT ( 'NONE',  ( -40.41683116089613748, -25.31532428806244539, 5.082404371757057504 ) ) ;
#61292 = CARTESIAN_POINT ( 'NONE',  ( -49.11047489538273680, -25.15112582127123275, 6.935676789746522353 ) ) ;
#61293 = DIRECTION ( 'NONE',  ( 0.000000000000000000, -1.000000000000000000, 0.000000000000000000 ) ) ;
#61294 = ORIENTED_EDGE ( 'NONE', *, *, #83892, .T. ) ;
#61295 = CARTESIAN_POINT ( 'NONE',  ( 19.60162835767302880, 5.811842276320244416, -1.500000000000002220 ) ) ;
#61296 = ORIENTED_EDGE ( 'NONE', *, *, #47485, .F. ) ;
#61297 = ORIENTED_EDGE ( 'NONE', *, *, #24930, .F. ) ;
#61298 = VERTEX_POINT ( 'NONE', #74780 ) ;
#61299 = ORIENTED_EDGE ( 'NONE', *, *, #29248, .T. ) ;
#61300 = CARTESIAN_POINT ( 'NONE',  ( -23.06710473063640165, 0.7821689226722955413, 11.49999999999998934 ) ) ;
#61301 = CARTESIAN_POINT ( 'NONE',  ( -40.11925438608624717, -25.18341647909762315, 3.283321612209681994 ) ) ;
#61302 = CARTESIAN_POINT ( 'NONE',  ( -19.72078065558051208, -4.686549088087978099, -1.500000000000002220 ) ) ;
#61303 = VERTEX_POINT ( 'NONE', #97131 ) ;
#61304 = CARTESIAN_POINT ( 'NONE',  ( -122.5228709571500616, -24.64898659630368272, 1.056161002820833028 ) ) ;
#61305 = VECTOR ( 'NONE', #55756, 1000.000000000000000 ) ;
#61306 = LINE ( 'NONE', #67417, #85475 ) ;
#61307 = EDGE_CURVE ( 'NONE', #64861, #6511, #91502, .T. ) ;
#61308 = CARTESIAN_POINT ( 'NONE',  ( 27.53860345374808105, -1.477225279485574028, -6.982392034746242260 ) ) ;
#61309 = CARTESIAN_POINT ( 'NONE',  ( -99.51916323793128072, -23.73791477778911840, 11.05961554403170588 ) ) ;
#61311 = VERTEX_POINT ( 'NONE', #44356 ) ;
#61310 = CARTESIAN_POINT ( 'NONE',  ( 7.480126432006339421, -20.11416664461015458, 11.49999999999999645 ) ) ;
#61312 = FACE_OUTER_BOUND ( 'NONE', #73909, .T. ) ;
#61313 = CARTESIAN_POINT ( 'NONE',  ( -61.65509961064937272, -23.48786465467240703, 11.44779295918255180 ) ) ;
#61314 = ORIENTED_EDGE ( 'NONE', *, *, #77301, .F. ) ;
#61315 = CARTESIAN_POINT ( 'NONE',  ( -4.968023186724614959, -20.10795263665959709, -1.500000000000002220 ) ) ;
#61316 = ADVANCED_FACE ( 'NONE', ( #14375 ), #6274, .T. ) ;
#61317 = EDGE_LOOP ( 'NONE', ( #42252, #65927, #6289, #1039 ) ) ;
#61319 = ORIENTED_EDGE ( 'NONE', *, *, #9351, .F. ) ;
#61318 = CARTESIAN_POINT ( 'NONE',  ( -123.6228709571500559, -24.51283580621365132, 0.6167428607019813658 ) ) ;
#61320 = EDGE_CURVE ( 'NONE', #11793, #60035, #6406, .T. ) ;
#61321 = DIRECTION ( 'NONE',  ( -3.773278334453080206E-23, 0.9999999999976377785, 2.173523156925979975E-06 ) ) ;
#61322 = ORIENTED_EDGE ( 'NONE', *, *, #3045, .T. ) ;
#61323 = ORIENTED_EDGE ( 'NONE', *, *, #46005, .F. ) ;
#61324 = CARTESIAN_POINT ( 'NONE',  ( 3.797776442307698286, -5.876774720514399419, 18.16025641025640525 ) ) ;
#61325 = VECTOR ( 'NONE', #25433, 1000.000000000000227 ) ;
#61326 = CARTESIAN_POINT ( 'NONE',  ( -65.62370077586832906, -25.00158670708910691, 2.256160236439222366 ) ) ;
#61327 = CARTESIAN_POINT ( 'NONE',  ( 9.922928194174257754, 19.57116106031148561, 11.49999999999999645 ) ) ;
#61328 = CARTESIAN_POINT ( 'NONE',  ( -5.891025641025637860, -6.376774720514427841, 21.75000000000000711 ) ) ;
#61329 = CARTESIAN_POINT ( 'NONE',  ( 19.01167203989450982, 12.12494712425435850, 11.49999999999998934 ) ) ;
#61330 = CARTESIAN_POINT ( 'NONE',  ( -8.441512789788195192, 19.21024974253229800, 11.49999999999998934 ) ) ;
#61331 = DIRECTION ( 'NONE',  ( 6.267148949376394486E-16, -1.000000000000000000, -5.583826031377232793E-16 ) ) ;
#61332 = DIRECTION ( 'NONE',  ( -0.000000000000000000, 1.000000000000000000, -0.000000000000000000 ) ) ;
#61333 = ORIENTED_EDGE ( 'NONE', *, *, #43858, .T. ) ;
#61334 = ORIENTED_EDGE ( 'NONE', *, *, #17923, .T. ) ;
#61335 = ORIENTED_EDGE ( 'NONE', *, *, #27502, .F. ) ;
#61336 = PLANE ( 'NONE',  #15826 ) ;
#61337 = EDGE_CURVE ( 'NONE', #17515, #29214, #12252, .T. ) ;
#61338 = EDGE_CURVE ( 'NONE', #71272, #32855, #54701, .T. ) ;
#61339 = CARTESIAN_POINT ( 'NONE',  ( 2.436486579176012413, 21.40072447632485364, -1.500000000000002220 ) ) ;
#61340 = LINE ( 'NONE', #92759, #32775 ) ;
#61341 = EDGE_LOOP ( 'NONE', ( #18346, #89536, #11485, #39957 ) ) ;
#61342 = CARTESIAN_POINT ( 'NONE',  ( -20.44436638909326120, 5.324712401148210539, -1.500000000000002220 ) ) ;
#61343 = DIRECTION ( 'NONE',  ( -0.000000000000000000, -1.000000000000000000, -0.000000000000000000 ) ) ;
#61344 = CARTESIAN_POINT ( 'NONE',  ( -64.62739518140152484, -24.51314013834315730, 0.6176544820404094027 ) ) ;
#61345 = CARTESIAN_POINT ( 'NONE',  ( -44.52287095715007581, -24.66019654487199730, 8.947790411086117501 ) ) ;
#61346 = CARTESIAN_POINT ( 'NONE',  ( -5.366453405989236813, 0.000000000000000000, 0.000000000000000000 ) ) ;
#61347 = CARTESIAN_POINT ( 'NONE',  ( 31.60706529141452137, -4.540774720514427543, 26.12024523944105070 ) ) ;
#61348 = CARTESIAN_POINT ( 'NONE',  ( 8.970247382295582383, 20.24485829007567617, -1.500000000000002220 ) ) ;
#61349 = CARTESIAN_POINT ( 'NONE',  ( -71.54956710204380954, -24.15543982623907127, -0.2315651400026636497 ) ) ;
#61350 = ORIENTED_EDGE ( 'NONE', *, *, #38707, .T. ) ;
#61351 = CARTESIAN_POINT ( 'NONE',  ( 4.621320343559619737, 12.50000000000004974, 0.000000000000000000 ) ) ;
#61352 = LINE ( 'NONE', #92773, #16776 ) ;
#61353 = DIRECTION ( 'NONE',  ( 0.000000000000000000, -2.173523156925980399E-06, 0.9999999999976378895 ) ) ;
#61354 = ADVANCED_FACE ( 'NONE', ( #1168 ), #31102, .T. ) ;
#61355 = EDGE_CURVE ( 'NONE', #80660, #98207, #18928, .T. ) ;
#61356 = CARTESIAN_POINT ( 'NONE',  ( -100.5869819392765123, -24.73486907724917572, 1.287355809206965240 ) ) ;
#61357 = B_SPLINE_CURVE_WITH_KNOTS ( 'NONE', 3,
 ( #14163, #28902, #45140, #61865 ),
 .UNSPECIFIED., .F., .F.,
 ( 4, 4 ),
 ( 0.000000000000000000, 9.999999999998897304E-05 ),
 .UNSPECIFIED. ) ;
#61358 = CARTESIAN_POINT ( 'NONE',  ( -17.22176335520693158, -9.073154711715998744, 11.49999999999998934 ) ) ;
#61359 = CARTESIAN_POINT ( 'NONE',  ( -7.638042729800005759, 19.97414216180626667, 11.49999999999998934 ) ) ;
#61360 = CARTESIAN_POINT ( 'NONE',  ( -119.4728709571500360, -25.30558663486607429, 5.000950657679038791 ) ) ;
#61361 = CARTESIAN_POINT ( 'NONE',  ( -105.5228709571500758, -25.00182538069145366, 7.747789668545101094 ) ) ;
#61362 = CARTESIAN_POINT ( 'NONE',  ( -106.5562042904834072, -24.65952944569305316, 1.056160979905704789 ) ) ;
#61363 = CARTESIAN_POINT ( 'NONE',  ( -38.62287095715005592, -24.65952944569303895, 1.056160979905692798 ) ) ;
#61364 = CARTESIAN_POINT ( 'NONE',  ( -16.57510365746454184, 15.48777146884464884, -1.500000000000002220 ) ) ;
#61365 = B_SPLINE_SURFACE_WITH_KNOTS ( 'NONE', 3, 3, ( 
 ( #96033, #57493, #66114, #64619 ),
 ( #18408, #81308, #12779, #11791 ),
 ( #49377, #97523, #88928, #27529 ),
 ( #34642, #10799, #41764, #19894 ),
 ( #2696, #74199, #50371, #42761 ),
 ( #88427, #73696, #58979, #72708 ),
 ( #33639, #26017, #80812, #50867 ) ),
 .UNSPECIFIED., .F., .F., .F.,
 ( 4, 3, 4 ),
 ( 4, 4 ),
 ( 0.0004766839783816396374, 0.1029713700210894006, 0.2054660560637971700 ),
 ( 0.6196516260353998051, 0.6209502567131185424 ),
 .UNSPECIFIED. ) ;
#61366 = CARTESIAN_POINT ( 'NONE',  ( 10.34999999999998010, 22.00000000000000000, 2.100000000000000089 ) ) ;
#61367 = CARTESIAN_POINT ( 'NONE',  ( 32.73857899460458754, 5.965225279485572685, -13.20677013500358399 ) ) ;
#61368 = CARTESIAN_POINT ( 'NONE',  ( -7.013475202606065828, -18.52788797337992222, 11.49999999999999645 ) ) ;
#61369 = LINE ( 'NONE', #38015, #20441 ) ;
#61370 = EDGE_CURVE ( 'NONE', #48067, #60922, #40133, .T. ) ;
#61371 = ORIENTED_EDGE ( 'NONE', *, *, #30452, .T. ) ;
#61372 = CARTESIAN_POINT ( 'NONE',  ( 15.22086173316507285, -2.682774720514426559, -27.22822144916453624 ) ) ;
#61373 = CARTESIAN_POINT ( 'NONE',  ( -61.64687923781919920, -25.16711686381824364, 3.101159594853581503 ) ) ;
#61374 = CARTESIAN_POINT ( 'NONE',  ( 9.069627533930374241, 19.64968329815391712, -1.500000000000002220 ) ) ;
#61375 = CARTESIAN_POINT ( 'NONE',  ( -63.62287095715004881, -29.50248528299804818, 1.056150453629034924 ) ) ;
#61376 = VECTOR ( 'NONE', #3720, 1000.000000000000000 ) ;
#61377 = CARTESIAN_POINT ( 'NONE',  ( 19.29218144733592055, -2.436590042558338443, -1.500000000000002220 ) ) ;
#61378 = CARTESIAN_POINT ( 'NONE',  ( -4.686006777320708139, -5.965225279485572685, 29.60911411231905888 ) ) ;
#61379 = FACE_OUTER_BOUND ( 'NONE', #11509, .T. ) ;
#61380 = CARTESIAN_POINT ( 'NONE',  ( -4.105667982141768313, -19.37954422259287668, -1.500000000000002220 ) ) ;
#61381 = ORIENTED_EDGE ( 'NONE', *, *, #7100, .F. ) ;
#61382 = CARTESIAN_POINT ( 'NONE',  ( 8.409737122318338365, 18.51778827956368190, 11.49999999999999645 ) ) ;
#61383 = DIRECTION ( 'NONE',  ( -3.773278334453079618E-23, 0.9999999999976377785, 2.173523156925979975E-06 ) ) ;
#61384 = ADVANCED_FACE ( 'NONE', ( #63077 ), #77267, .T. ) ;
#61385 = CARTESIAN_POINT ( 'NONE',  ( -46.62287095715004881, -24.66019654487198665, 8.947790411086135265 ) ) ;
#61386 = ADVANCED_FACE ( 'NONE', ( #46336 ), #92996, .F. ) ;
#61387 = B_SPLINE_CURVE_WITH_KNOTS ( 'NONE', 3,
 ( #82677, #64994, #3577, #34519 ),
 .UNSPECIFIED., .F., .F.,
 ( 4, 4 ),
 ( 0.000000000000000000, 9.999999999999592548E-05 ),
 .UNSPECIFIED. ) ;
#61388 = ORIENTED_EDGE ( 'NONE', *, *, #20116, .F. ) ;
#61389 = CARTESIAN_POINT ( 'NONE',  ( -0.04929185891187171792, -22.41187815084102652, 8.907023374642855984 ) ) ;
#61390 = PLANE ( 'NONE',  #39576 ) ;
#61391 = CARTESIAN_POINT ( 'NONE',  ( -49.08163135806235289, -25.25214541495745380, 5.465038328920414301 ) ) ;
#61392 = AXIS2_PLACEMENT_3D ( 'NONE', #52648, #28309, #68869 ) ;
#61393 = CARTESIAN_POINT ( 'NONE',  ( -127.6228709571500559, -24.65952944569305316, 1.056160979905707897 ) ) ;
#61394 = CARTESIAN_POINT ( 'NONE',  ( -82.22287095715005023, -23.47596703998600276, 11.44779298504227683 ) ) ;
#61395 = CARTESIAN_POINT ( 'NONE',  ( -16.95507112718987486, -10.73317591066004084, -1.500000000000002220 ) ) ;
#61396 = EDGE_CURVE ( 'NONE', #88472, #80402, #87390, .T. ) ;
#61397 = CARTESIAN_POINT ( 'NONE',  ( -120.5228709571500900, -25.00182538069145366, 7.747789668545101982 ) ) ;
#61398 = ORIENTED_EDGE ( 'NONE', *, *, #11213, .T. ) ;
#61399 = DIRECTION ( 'NONE',  ( 0.000000000000000000, 0.000000000000000000, -1.000000000000000000 ) ) ;
#61400 = EDGE_CURVE ( 'NONE', #77615, #3631, #70172, .T. ) ;
#61401 = CARTESIAN_POINT ( 'NONE',  ( 7.980177114813061579, 21.45908683785374649, 11.49999999999999645 ) ) ;
#61402 = CARTESIAN_POINT ( 'NONE',  ( -19.63924127562733446, 11.44998032699685631, 11.49999999999998934 ) ) ;
#61403 = CARTESIAN_POINT ( 'NONE',  ( -49.68676680831369197, -25.26258819900877484, 4.434853480562869876 ) ) ;
#61404 = CARTESIAN_POINT ( 'NONE',  ( -126.5228709571500900, -24.51387760970726504, 9.387446482453400520 ) ) ;
#61405 = CARTESIAN_POINT ( 'NONE',  ( -38.59384448668303946, -24.15620529776627379, 10.23563542870660825 ) ) ;
#61406 = PLANE ( 'NONE',  #20584 ) ;
#61407 = CARTESIAN_POINT ( 'NONE',  ( -128.5215767096398451, -24.35071581493544102, 9.817618358456019934 ) ) ;
#61408 = AXIS2_PLACEMENT_3D ( 'NONE', #82940, #75329, #14426 ) ;
#61409 = DIRECTION ( 'NONE',  ( -0.000000000000000000, -1.000000000000000000, -0.000000000000000000 ) ) ;
#61410 = ORIENTED_EDGE ( 'NONE', *, *, #40565, .T. ) ;
#61411 = CARTESIAN_POINT ( 'NONE',  ( 6.737473828552405841, -19.20966278261563076, 11.49999999999998934 ) ) ;
#61412 = ORIENTED_EDGE ( 'NONE', *, *, #19293, .F. ) ;
#61413 = CARTESIAN_POINT ( 'NONE',  ( -12.06219892284564388, 19.56905390912838172, 11.49999999999998934 ) ) ;
#61414 = DIRECTION ( 'NONE',  ( -0.000000000000000000, 1.000000000000000000, -0.000000000000000000 ) ) ;
#61415 = ORIENTED_EDGE ( 'NONE', *, *, #87362, .T. ) ;
#61416 = DIRECTION ( 'NONE',  ( -3.773278334453079030E-23, 0.9999999999976377785, 2.173523156925979128E-06 ) ) ;
#61417 = CARTESIAN_POINT ( 'NONE',  ( -77.51696115879298077, -23.73791477778911840, 11.05961554403170588 ) ) ;
#61418 = EDGE_CURVE ( 'NONE', #48372, #89948, #3841, .T. ) ;
#61419 = CARTESIAN_POINT ( 'NONE',  ( -51.61380951771659653, -23.48786465467241413, 11.44779295918254824 ) ) ;
#61421 = ORIENTED_EDGE ( 'NONE', *, *, #23176, .F. ) ;
#61420 = CARTESIAN_POINT ( 'NONE',  ( -16.85803360905838488, 12.98640638483674259, 11.49999999999999645 ) ) ;
#61422 = ORIENTED_EDGE ( 'NONE', *, *, #61754, .F. ) ;
#61423 = CARTESIAN_POINT ( 'NONE',  ( -0.9571703918902072505, -22.19477237104690914, -1.500000000000002220 ) ) ;
#61424 = B_SPLINE_CURVE_WITH_KNOTS ( 'NONE', 3,
 ( #79956, #96192, #49529, #26680 ),
 .UNSPECIFIED., .F., .F.,
 ( 4, 4 ),
 ( 0.000000000000000000, 9.999999999998897304E-05 ),
 .UNSPECIFIED. ) ;
#61425 = CARTESIAN_POINT ( 'NONE',  ( 0.06016934085327452914, 20.63536315578604174, -1.500000000000002220 ) ) ;
#61426 = ORIENTED_EDGE ( 'NONE', *, *, #74682, .T. ) ;
#61427 = VERTEX_POINT ( 'NONE', #14875 ) ;
#61428 = CARTESIAN_POINT ( 'NONE',  ( -109.0556427821970260, -25.31627237126944152, 4.716568607272451530 ) ) ;
#61429 = CARTESIAN_POINT ( 'NONE',  ( -121.6228709571500843, -24.34917612406838927, 0.1852690917426690620 ) ) ;
#61430 = ORIENTED_EDGE ( 'NONE', *, *, #1607, .F. ) ;
#61431 = VECTOR ( 'NONE', #96708, 1000.000000000000000 ) ;
#61432 = DIRECTION ( 'NONE',  ( 0.000000000000000000, -1.000000000000000000, 0.000000000000000000 ) ) ;
#61433 = VECTOR ( 'NONE', #3754, 1000.000000000000114 ) ;
#61434 = ORIENTED_EDGE ( 'NONE', *, *, #65989, .F. ) ;
#61435 = CARTESIAN_POINT ( 'NONE',  ( -127.4728709571500360, -25.30558663486607429, 5.000950657679038791 ) ) ;
#61436 = CARTESIAN_POINT ( 'NONE',  ( -44.52287095715006160, -24.64898659630367916, 1.056161002820819261 ) ) ;
#61437 = CARTESIAN_POINT ( 'NONE',  ( -11.07951500695464553, -17.62175104703424466, -1.500000000000002220 ) ) ;
#61438 = CARTESIAN_POINT ( 'NONE',  ( 21.63681353182189682, 2.665401433100548889, 11.49999999999999645 ) ) ;
#61439 = DIRECTION ( 'NONE',  ( -3.773278334444167608E-23, 1.000000000000000000, 0.000000000000000000 ) ) ;
#61440 = CARTESIAN_POINT ( 'NONE',  ( -100.4498239493576648, -25.03284467579916495, 7.563174216508126158 ) ) ;
#61441 = CARTESIAN_POINT ( 'NONE',  ( 21.67916507323446496, -5.852930566066080864, 11.49999999999998934 ) ) ;
#61442 = AXIS2_PLACEMENT_3D ( 'NONE', #20608, #82508, #52570 ) ;
#61443 = CARTESIAN_POINT ( 'NONE',  ( -25.92875734969025814, -6.376774720514426953, 30.51402280011862089 ) ) ;
#61444 = EDGE_LOOP ( 'NONE', ( #467, #49069, #36556, #84861 ) ) ;
#61445 = CARTESIAN_POINT ( 'NONE',  ( -58.52287095715004739, -23.48783264082477018, -1.443836473390092801 ) ) ;
#61446 = DIRECTION ( 'NONE',  ( 1.000000000000000000, 3.773278334444166432E-23, 8.201307841325785021E-29 ) ) ;
#61447 = ORIENTED_EDGE ( 'NONE', *, *, #14033, .F. ) ;
#61448 = AXIS2_PLACEMENT_3D ( 'NONE', #31809, #38915, #8468 ) ;
#61449 = EDGE_LOOP ( 'NONE', ( #97099, #21511, #75576, #64851 ) ) ;
#61450 = ORIENTED_EDGE ( 'NONE', *, *, #28611, .F. ) ;
#61451 = EDGE_CURVE ( 'NONE', #8232, #93778, #94572, .T. ) ;
#61452 = CARTESIAN_POINT ( 'NONE',  ( -14.61619677566029729, 15.53698580111986693, -1.500000000000002220 ) ) ;
#61453 = ORIENTED_EDGE ( 'NONE', *, *, #30644, .T. ) ;
#61454 = CARTESIAN_POINT ( 'NONE',  ( 11.68726034403320746, 17.49698133428071145, 11.49999999999998934 ) ) ;
#61455 = CARTESIAN_POINT ( 'NONE',  ( -30.40788910079855256, -25.13731019820412982, 2.712646531854225440 ) ) ;
#61456 = AXIS2_PLACEMENT_3D ( 'NONE', #45563, #53177, #99326 ) ;
#61457 = CARTESIAN_POINT ( 'NONE',  ( -110.6746315611901963, -25.20166100307829993, 3.341187069408153132 ) ) ;
#61458 = CARTESIAN_POINT ( 'NONE',  ( 10.01577673925062584, -3.316774720514425567, -27.02510548822787584 ) ) ;
#61459 = CARTESIAN_POINT ( 'NONE',  ( -6.321128248299066499, 21.05883132939252533, -1.500000000000002220 ) ) ;
#61460 = CARTESIAN_POINT ( 'NONE',  ( -87.50252558622028687, -24.65952944569304606, 1.056160979905703678 ) ) ;
#61461 = ORIENTED_EDGE ( 'NONE', *, *, #75003, .T. ) ;
#61462 = CARTESIAN_POINT ( 'NONE',  ( -80.88924702628075636, -25.30869131066464561, 4.592921213095906730 ) ) ;
#61463 = ADVANCED_FACE ( 'NONE', ( #30606 ), #78265, .T. ) ;
#61464 = CARTESIAN_POINT ( 'NONE',  ( -107.5562042904834215, -23.47593901973091235, -1.443836447538999312 ) ) ;
#61465 = ADVANCED_FACE ( 'NONE', ( #2677 ), #65592, .T. ) ;
#61466 = ADVANCED_FACE ( 'NONE', ( #79278 ), #66081, .T. ) ;
#61467 = FACE_OUTER_BOUND ( 'NONE', #94878, .T. ) ;
#61468 = CARTESIAN_POINT ( 'NONE',  ( -55.52287095715005449, -29.50248789122583659, 2.256150453626215580 ) ) ;
#61469 = ADVANCED_FACE ( 'NONE', ( #80287 ), #83086, .T. ) ;
#61470 = CARTESIAN_POINT ( 'NONE',  ( -0.08805446101867206443, -21.91006580534973480, 9.960784317162939772 ) ) ;
#61471 = CARTESIAN_POINT ( 'NONE',  ( 1.764508054474889009, 21.21474994468914943, 11.49999999999998934 ) ) ;
#61472 = CARTESIAN_POINT ( 'NONE',  ( -46.58953762381672448, -23.48786465467241058, 11.44779295918255180 ) ) ;
#61473 = CARTESIAN_POINT ( 'NONE',  ( -107.5129983477871320, -24.51419770103159124, 9.386484678747168076 ) ) ;
#61474 = CARTESIAN_POINT ( 'NONE',  ( -90.62287095715009855, -24.82558206586143967, 1.605769216559451484 ) ) ;
#61475 = CARTESIAN_POINT ( 'NONE',  ( -33.47775787355578103, -24.65952944569304606, 1.056160979905695907 ) ) ;
#61476 = CARTESIAN_POINT ( 'NONE',  ( -6.671648801611133273, 21.52854475820963032, -1.500000000000002220 ) ) ;
#61477 = DIRECTION ( 'NONE',  ( 0.000000000000000000, 0.000000000000000000, -1.000000000000000000 ) ) ;
#61478 = EDGE_LOOP ( 'NONE', ( #44297, #82596, #68286, #64746 ) ) ;
#61479 = CARTESIAN_POINT ( 'NONE',  ( -99.10931216887415474, -25.17291523371832440, 6.862075660167399782 ) ) ;
#61480 = CARTESIAN_POINT ( 'NONE',  ( 18.74904333037421011, -5.873301551693434597, 11.49999999999999645 ) ) ;
#61481 = CARTESIAN_POINT ( 'NONE',  ( -26.91814428177455909, -5.965225279485572685, 29.98490496616818746 ) ) ;
#61483 = B_SPLINE_CURVE_WITH_KNOTS ( 'NONE', 3,
 ( #73865, #80100, #1491, #56787 ),
 .UNSPECIFIED., .F., .F.,
 ( 4, 4 ),
 ( 0.000000000000000000, 0.0001000000000000444977 ),
 .UNSPECIFIED. ) ;
#61482 = PLANE ( 'NONE',  #51252 ) ;
#61484 = ADVANCED_FACE ( 'NONE', ( #5653 ), #58465, .F. ) ;
#61485 = VERTEX_POINT ( 'NONE', #28490 ) ;
#61486 = CARTESIAN_POINT ( 'NONE',  ( -69.92726831997306647, -25.30507734521815522, 4.890125790641020487 ) ) ;
#61487 = CARTESIAN_POINT ( 'NONE',  ( 2.100208336950355914, 0.000000000000000000, 0.000000000000000000 ) ) ;
#61488 = CARTESIAN_POINT ( 'NONE',  ( -100.5515626640960960, -25.31439534661152280, 5.205058145584142260 ) ) ;
#61490 = EDGE_CURVE ( 'NONE', #78152, #94223, #26829, .T. ) ;
#61489 = CARTESIAN_POINT ( 'NONE',  ( -14.12090166725071327, 13.77431136191591143, -1.500000000000002220 ) ) ;
#61491 = ORIENTED_EDGE ( 'NONE', *, *, #31847, .T. ) ;
#61492 = CARTESIAN_POINT ( 'NONE',  ( -110.0886599897713012, -25.19857471502731272, 3.319100349969234642 ) ) ;
#61493 = CARTESIAN_POINT ( 'NONE',  ( -118.5228709571501184, -24.34917612406837861, 0.1852690917426619288 ) ) ;
#61494 = EDGE_CURVE ( 'NONE', #13745, #5619, #21365, .T. ) ;
#61495 = COORDINATED_UNIVERSAL_TIME_OFFSET ( 0, 0, .AHEAD. ) ;
#61496 = ORIENTED_EDGE ( 'NONE', *, *, #24095, .T. ) ;
#61497 = CARTESIAN_POINT ( 'NONE',  ( -7.160000000000000142, -9.123836073446797812, -2.666350264951732552 ) ) ;
#61498 = PLANE ( 'NONE',  #2105 ) ;
#61499 = CARTESIAN_POINT ( 'NONE',  ( 32.45853543194704116, -0.3587747205144265483, 9.169203677920338080 ) ) ;
#61500 = DIRECTION ( 'NONE',  ( -0.000000000000000000, 0.000000000000000000, -1.000000000000000000 ) ) ;
#61501 = CARTESIAN_POINT ( 'NONE',  ( -100.6814946224345846, -29.50249428492551829, 5.197779886230994073 ) ) ;
#61502 = CIRCLE ( 'NONE', #59912, 251.4258649670780699 ) ;
#61503 = LINE ( 'NONE', #54891, #31118 ) ;
#61504 = CARTESIAN_POINT ( 'NONE',  ( 7.347880794884120722E-16, 5.356774720514425603, -6.000000000000000888 ) ) ;
#61505 = CARTESIAN_POINT ( 'NONE',  ( 4.555139465550277933, 19.45931829295258453, 11.49999999999998934 ) ) ;
#61506 = B_SPLINE_CURVE_WITH_KNOTS ( 'NONE', 3,
 ( #86428, #47373, #25022, #55488 ),
 .UNSPECIFIED., .F., .F.,
 ( 4, 4 ),
 ( 0.000000000000000000, 0.0001000000000000028644 ),
 .UNSPECIFIED. ) ;
#61507 = ADVANCED_FACE ( 'NONE', ( #90890 ), #67572, .F. ) ;
#61508 = CARTESIAN_POINT ( 'NONE',  ( -127.6228709571500559, -23.47593901973091235, -1.443836447538995760 ) ) ;
#61509 = CARTESIAN_POINT ( 'NONE',  ( -45.62627668582059215, -24.92592662359561118, 8.075495903018000021 ) ) ;
#61510 = VERTEX_POINT ( 'NONE', #52339 ) ;
#61511 = AXIS2_PLACEMENT_3D ( 'NONE', #44836, #13866, #20481 ) ;
#61512 = EDGE_CURVE ( 'NONE', #95068, #50221, #1118, .T. ) ;
#61513 = VECTOR ( 'NONE', #12488, 1000.000000000000114 ) ;
#61514 = CARTESIAN_POINT ( 'NONE',  ( -106.9228709571500673, -23.47593901973090169, -1.443836447538996426 ) ) ;
#61515 = CARTESIAN_POINT ( 'NONE',  ( -39.62287095715005592, -29.50247984919015209, -1.443849546365060466 ) ) ;
#61516 = DIRECTION ( 'NONE',  ( 0.000000000000000000, -2.173523156925979552E-06, 0.9999999999976378895 ) ) ;
#61517 = CARTESIAN_POINT ( 'NONE',  ( -100.5228709571501042, -23.85229601348996553, 10.88205029486208453 ) ) ;
#61518 = AXIS2_PLACEMENT_3D ( 'NONE', #92333, #76598, #29936 ) ;
#61519 = B_SPLINE_CURVE_WITH_KNOTS ( 'NONE', 3,
 ( #84597, #15579, #24196, #92206, #22184, #62279 ),
 .UNSPECIFIED., .F., .F.,
 ( 4, 2, 4 ),
 ( 1.958437160922047748E-11, 0.002593568795227694981, 0.005187137570871018510 ),
 .UNSPECIFIED. ) ;
#61520 = CARTESIAN_POINT ( 'NONE',  ( -1.140932434931746582E-13, -5.876774720514426953, 21.78128695274321203 ) ) ;
#61521 = CARTESIAN_POINT ( 'NONE',  ( -1.649669150391666506, -5.876774720514411854, 19.67464842890028365 ) ) ;
#61522 = B_SPLINE_CURVE_WITH_KNOTS ( 'NONE', 3,
 ( #10863, #26591, #9853, #11360, #26081, #25071 ),
 .UNSPECIFIED., .F., .F.,
 ( 4, 2, 4 ),
 ( 6.391158118966174708E-06, 0.001387004593080789615, 0.002767618028042612838 ),
 .UNSPECIFIED. ) ;
#61523 = AXIS2_PLACEMENT_3D ( 'NONE', #100218, #7893, #15999 ) ;
#61524 = FACE_OUTER_BOUND ( 'NONE', #46486, .T. ) ;
#61525 = CARTESIAN_POINT ( 'NONE',  ( -63.52287095715006160, -24.64898659630367561, 1.056161002820822592 ) ) ;
#61526 = ORIENTED_EDGE ( 'NONE', *, *, #68857, .F. ) ;
#61527 =( BOUNDED_SURFACE ( )  B_SPLINE_SURFACE ( 3, 2, ( 
 ( #64863, #98131, #66730 ),
 ( #21501, #5295, #87670 ),
 ( #33880, #44871, #51981 ),
 ( #64359, #95777, #95280 ),
 ( #82909, #90528, #82416 ),
 ( #18151, #36254, #5795 ),
 ( #97641, #29128, #28638 ),
 ( #49124, #88173, #75297 ),
 ( #28144, #20509, #52478 ),
 ( #60105, #67717, #51480 ),
 ( #2945, #13894, #91029 ),
 ( #36749, #80051, #57240 ) ),
 .UNSPECIFIED., .F., .F., .T. ) 
 B_SPLINE_SURFACE_WITH_KNOTS ( ( 4, 2, 2, 2, 2, 4 ),
 ( 3, 3 ),
 ( 5.963111948670274387E-19, 0.0004805055694112242209, 0.0007207583541168360603, 0.0009610111388224478997, 0.001441516708233671470, 0.001922022277644895149 ),
 ( 0.000000000000000000, 1.000000000000000000 ),
 .UNSPECIFIED. ) 
 GEOMETRIC_REPRESENTATION_ITEM ( )  RATIONAL_B_SPLINE_SURFACE ( (
 ( 1.000000000000000000, 0.6532382444175209857, 1.000000000000000000),
 ( 1.000000000000000000, 0.6532227097440629349, 1.000000000000000000),
 ( 1.000000000000000000, 0.6547852517831300734, 1.000000000000000000),
 ( 1.000000000000000000, 0.6591574828660964336, 1.000000000000000000),
 ( 1.000000000000000000, 0.6609310395923762016, 1.000000000000000000),
 ( 1.000000000000000000, 0.6650742797340818413, 1.000000000000000000),
 ( 1.000000000000000000, 0.6674600455423553846, 1.000000000000000000),
 ( 1.000000000000000000, 0.6751670852230186037, 1.000000000000000000),
 ( 1.000000000000000000, 0.6812390391297645786, 1.000000000000000000),
 ( 1.000000000000000000, 0.6938890553660238547, 1.000000000000000000),
 ( 1.000000000000000000, 0.7006220437376451393, 1.000000000000000000),
 ( 1.000000000000000000, 0.7071067811865475727, 1.000000000000000000) ) ) 
 REPRESENTATION_ITEM ( '' )  SURFACE ( )  );
#61528 = CARTESIAN_POINT ( 'NONE',  ( -15.58492919356500650, -12.95507736684500699, -1.500000000000002220 ) ) ;
#61529 = CARTESIAN_POINT ( 'NONE',  ( -76.62287095715009855, -24.35013146730204170, 9.818937971375111928 ) ) ;
#61530 = DIRECTION ( 'NONE',  ( 2.168404344971008868E-16, 0.000000000000000000, 1.000000000000000000 ) ) ;
#61531 = FACE_OUTER_BOUND ( 'NONE', #156, .T. ) ;
#61532 = ORIENTED_EDGE ( 'NONE', *, *, #96745, .T. ) ;
#61533 = FACE_OUTER_BOUND ( 'NONE', #48719, .T. ) ;
#61534 = B_SPLINE_CURVE_WITH_KNOTS ( 'NONE', 3,
 ( #9320, #41801, #18441, #11333, #32663, #56525 ),
 .UNSPECIFIED., .F., .F.,
 ( 4, 2, 4 ),
 ( 0.000000000000000000, 0.001380901958385394833, 0.002761803916770789666 ),
 .UNSPECIFIED. ) ;
#61535 = CARTESIAN_POINT ( 'NONE',  ( 16.24926901856429140, 11.90123039513101411, -1.500000000000002220 ) ) ;
#61536 = CARTESIAN_POINT ( 'NONE',  ( 19.72786461798894209, 7.474574171381012100, 11.49999999999999645 ) ) ;
#61537 = CARTESIAN_POINT ( 'NONE',  ( -123.6228709571500559, -29.50250243563736774, 8.947779886222134493 ) ) ;
#61538 = CARTESIAN_POINT ( 'NONE',  ( 10.71795340210964120, -19.33932934982082585, 11.49999999999998934 ) ) ;
#61539 = CARTESIAN_POINT ( 'NONE',  ( 7.506095096478735407, 19.11734572241606145, 11.49999999999998934 ) ) ;
#61540 = PLANE ( 'NONE',  #56031 ) ;
#61541 = CARTESIAN_POINT ( 'NONE',  ( -60.63371511099986577, -24.63355581998385446, 0.9682620441943891043 ) ) ;
#61542 = ORIENTED_EDGE ( 'NONE', *, *, #44720, .T. ) ;
#61543 = FACE_OUTER_BOUND ( 'NONE', #63946, .T. ) ;
#61544 = ORIENTED_EDGE ( 'NONE', *, *, #35178, .F. ) ;
#61545 = PLANE ( 'NONE',  #91580 ) ;
#61546 = B_SPLINE_SURFACE_WITH_KNOTS ( 'NONE', 3, 1, ( 
 ( #14977, #70775 ),
 ( #100190, #24586 ),
 ( #53570, #30710 ),
 ( #38815, #46939 ),
 ( #55560, #15475 ),
 ( #39817, #23075 ),
 ( #8371, #86494 ),
 ( #1272, #47943 ),
 ( #55058, #54550 ),
 ( #84495, #45950 ),
 ( #76861, #39316 ),
 ( #757, #69780 ),
 ( #85488, #54066 ),
 ( #84990, #46436 ),
 ( #77368, #31201 ),
 ( #62174, #31710 ),
 ( #62677, #18977 ),
 ( #10369, #65191 ),
 ( #88502, #33206 ) ),
 .UNSPECIFIED., .F., .F., .F.,
 ( 4, 1, 1, 1, 1, 1, 1, 1, 1, 1, 1, 1, 1, 1, 1, 1, 4 ),
 ( 2, 2 ),
 ( 0.000000000000000000, 0.06976287284686377710, 0.1345149942976650026, 0.1951193525406911267, 0.2509143402908639020, 0.3026968495153159466, 0.3502960464810119801, 0.3933858467586653918, 0.4329734110072621656, 0.5070892430766293923, 0.5787491638444322017, 0.6502280224451006951, 0.7224618180302712078, 0.7938856428547002020, 0.8631290414909040809, 0.9313229315869653302, 1.000000000000000000 ),
 ( 0.000000000000000000, 1.000000000000000000 ),
 .UNSPECIFIED. ) ;
#61547 = DIRECTION ( 'NONE',  ( -0.9685340172660600322, 0.000000000000000000, 0.2488812114211667037 ) ) ;
#61548 = VERTEX_POINT ( 'NONE', #66594 ) ;
#61549 = EDGE_LOOP ( 'NONE', ( #84134, #32076, #88461, #83654 ) ) ;
#61550 = ORIENTED_EDGE ( 'NONE', *, *, #20550, .F. ) ;
#61551 = DIRECTION ( 'NONE',  ( -4.448048651795319837E-16, 1.000000000000000000, -7.118365844322522408E-16 ) ) ;
#61552 = CARTESIAN_POINT ( 'NONE',  ( -75.62287095715004170, -24.99132157543084176, 2.256160258750667502 ) ) ;
#61553 = CARTESIAN_POINT ( 'NONE',  ( 0.3670296583442628213, -6.376774720514417183, 20.26087634804755311 ) ) ;
#61554 = CARTESIAN_POINT ( 'NONE',  ( -20.26430336558559020, 4.098603726722801710, -1.500000000000002220 ) ) ;
#61555 = CARTESIAN_POINT ( 'NONE',  ( 0.9236959384754221958, 21.56878955078795812, 11.49999999999999645 ) ) ;
#61556 = VERTEX_POINT ( 'NONE', #19872 ) ;
#61557 = CARTESIAN_POINT ( 'NONE',  ( -83.62287095715005592, -23.47593901973091235, -1.443836447539004642 ) ) ;
#61558 = CARTESIAN_POINT ( 'NONE',  ( 3.552794897967157528, -5.876774720514401196, 18.18650940196788568 ) ) ;
#61559 = CARTESIAN_POINT ( 'NONE',  ( -13.11617634606977489, 18.14055439154125438, 11.49999999999998934 ) ) ;
#61560 = B_SPLINE_CURVE_WITH_KNOTS ( 'NONE', 3,
 ( #66624, #58995, #52370, #98024, #74694, #28522 ),
 .UNSPECIFIED., .F., .F.,
 ( 4, 2, 4 ),
 ( 6.384118678617502043E-06, 0.001386860460828380839, 0.002767336802978144494 ),
 .UNSPECIFIED. ) ;
#61561 = DIRECTION ( 'NONE',  ( 0.000000000000000000, 0.000000000000000000, -1.000000000000000000 ) ) ;
#61562 = DIRECTION ( 'NONE',  ( 1.000000000000000000, 0.000000000000000000, 0.000000000000000000 ) ) ;
#61563 = VERTEX_POINT ( 'NONE', #83276 ) ;
#61564 = CARTESIAN_POINT ( 'NONE',  ( -106.6228709571500559, -29.50250786944525672, 11.44777988621622988 ) ) ;
#61565 = CARTESIAN_POINT ( 'NONE',  ( -56.52287095715006870, -29.50247984919015209, -1.443849546365056913 ) ) ;
#61566 = CARTESIAN_POINT ( 'NONE',  ( -5.366453405989239478, 14.49999999999999645, 11.24599928863594300 ) ) ;
#61567 = CARTESIAN_POINT ( 'NONE',  ( -17.98194200498208062, 10.70670730041394947, 11.49999999999998934 ) ) ;
#61568 = VERTEX_POINT ( 'NONE', #13754 ) ;
#61569 = AXIS2_PLACEMENT_3D ( 'NONE', #88184, #3950, #27282 ) ;
#61570 = DIRECTION ( 'NONE',  ( -3.773278334453079030E-23, 0.9999999999976377785, 2.173523156925979128E-06 ) ) ;
#61571 = ORIENTED_EDGE ( 'NONE', *, *, #58491, .F. ) ;
#61572 = PLANE ( 'NONE',  #76231 ) ;
#61573 = CARTESIAN_POINT ( 'NONE',  ( 20.83148622972472808, -3.941400823363257366, -1.500000000000002220 ) ) ;
#61574 = EDGE_LOOP ( 'NONE', ( #8359, #26307 ) ) ;
#61575 = CARTESIAN_POINT ( 'NONE',  ( -117.5903100292338621, -24.15543982623907837, -0.2315651400026547124 ) ) ;
#61577 = EDGE_CURVE ( 'NONE', #52051, #42367, #53423, .T. ) ;
#61576 = CARTESIAN_POINT ( 'NONE',  ( 31.01539214510854237, -4.736880496761925130, -2.146553774717921304 ) ) ;
#61578 = CARTESIAN_POINT ( 'NONE',  ( -16.40380107638378604, 14.33077157581830008, 11.49999999999998934 ) ) ;
#61579 = CARTESIAN_POINT ( 'NONE',  ( -66.62287095715005592, -29.50250243563736774, 8.947779886222143375 ) ) ;
#61580 = AXIS2_PLACEMENT_3D ( 'NONE', #46309, #15846, #14346 ) ;
#61581 = ADVANCED_FACE ( 'NONE', ( #4670 ), #12258, .T. ) ;
#61582 = CARTESIAN_POINT ( 'NONE',  ( -76.60093289846236075, -23.73791477778911840, 11.05961554403170766 ) ) ;
#61583 = DIRECTION ( 'NONE',  ( -3.773278334453080206E-23, 0.9999999999976377785, 2.173523156925979975E-06 ) ) ;
#61584 = CARTESIAN_POINT ( 'NONE',  ( -18.37375256118794553, 11.78967355450649457, -1.500000000000002220 ) ) ;
#61585 = CARTESIAN_POINT ( 'NONE',  ( -1.064504969004270052, -6.376774720514408301, 19.35667676486395905 ) ) ;
#61586 = ORIENTED_EDGE ( 'NONE', *, *, #44079, .T. ) ;
#61587 = CARTESIAN_POINT ( 'NONE',  ( 25.73006673792228938, 5.175315920840755091, -7.739742029708382987 ) ) ;
#61588 = CARTESIAN_POINT ( 'NONE',  ( -123.6228709571500559, -24.65952944569304961, 1.056160979905703234 ) ) ;
#61589 = CARTESIAN_POINT ( 'NONE',  ( 15.63605935613269438, 6.475225279485573360, -27.55169773172585934 ) ) ;
#61590 = ORIENTED_EDGE ( 'NONE', *, *, #68134, .F. ) ;
#61591 = EDGE_CURVE ( 'NONE', #55431, #78619, #82776, .T. ) ;
#61592 = VECTOR ( 'NONE', #60092, 1000.000000000000114 ) ;
#61593 = EDGE_CURVE ( 'NONE', #65225, #48372, #95840, .T. ) ;
#61594 = VERTEX_POINT ( 'NONE', #29481 ) ;
#61595 = ADVANCED_FACE ( 'NONE', ( #91384 ), #50347, .F. ) ;
#61596 = AXIS2_PLACEMENT_3D ( 'NONE', #82248, #41715, #95981 ) ;
#61597 = ORIENTED_EDGE ( 'NONE', *, *, #4850, .T. ) ;
#61598 = AXIS2_PLACEMENT_3D ( 'NONE', #91698, #35928, #53165 ) ;
#61599 = FACE_OUTER_BOUND ( 'NONE', #87192, .T. ) ;
#61600 = CARTESIAN_POINT ( 'NONE',  ( -13.45780860896912934, -16.40347334334247265, -1.500000000000002220 ) ) ;
#61601 = LINE ( 'NONE', #94022, #77363 ) ;
#61602 = CARTESIAN_POINT ( 'NONE',  ( -79.79245360944284471, -25.27791940355850286, 7.413204867740626369 ) ) ;
#61603 = DIRECTION ( 'NONE',  ( 0.000000000000000000, -0.9999999999976377785, -2.173523156925979128E-06 ) ) ;
#61604 = VECTOR ( 'NONE', #86415, 999.9999999999998863 ) ;
#61605 = CARTESIAN_POINT ( 'NONE',  ( -9.899997732206244905, -16.63842163800745766, -1.500000000000002220 ) ) ;
#61606 = CARTESIAN_POINT ( 'NONE',  ( -69.86753664201866343, -25.30877541009007459, 5.411526165084938889 ) ) ;
#61607 = EDGE_LOOP ( 'NONE', ( #3472, #44446, #55214, #26517 ) ) ;
#61608 = CARTESIAN_POINT ( 'NONE',  ( -19.06185424839875964, 3.971334347869299286, 11.49999999999999645 ) ) ;
#61609 = CARTESIAN_POINT ( 'NONE',  ( -34.52287095715006160, -23.48783264083359867, -1.443836473376372442 ) ) ;
#61610 = CARTESIAN_POINT ( 'NONE',  ( -49.62287095715005592, -24.64965695001467694, 8.947790433994185832 ) ) ;
#61611 = EDGE_CURVE ( 'NONE', #31632, #76406, #81786, .T. ) ;
#61612 = ORIENTED_EDGE ( 'NONE', *, *, #91451, .T. ) ;
#61613 = DIRECTION ( 'NONE',  ( 1.000000000000000000, 3.773278334444167608E-23, 8.201307833595939069E-29 ) ) ;
#61614 = PLANE ( 'NONE',  #38458 ) ;
#61615 = CARTESIAN_POINT ( 'NONE',  ( -45.62287095715004881, -25.00158670708908915, 2.256160236439166855 ) ) ;
#61616 = CARTESIAN_POINT ( 'NONE',  ( 22.81105451610979173, -1.477225279485574028, -18.46691820600746681 ) ) ;
#61618 = EDGE_CURVE ( 'NONE', #60030, #26877, #98156, .T. ) ;
#61617 = CARTESIAN_POINT ( 'NONE',  ( -17.63651738508609412, 8.604534254076446231, -1.500000000000002220 ) ) ;
#61619 = DIRECTION ( 'NONE',  ( 0.000000000000000000, -2.173523156925979552E-06, 0.9999999999976378895 ) ) ;
#61620 = ORIENTED_EDGE ( 'NONE', *, *, #81316, .F. ) ;
#61621 = CARTESIAN_POINT ( 'NONE',  ( 14.45009471711328786, 16.04676183837579373, -1.500000000000002220 ) ) ;
#61622 = CARTESIAN_POINT ( 'NONE',  ( -95.52287095715006160, -23.48786465467241769, 11.44779295918254114 ) ) ;
#61623 = CARTESIAN_POINT ( 'NONE',  ( -78.94303308397306296, -29.50249597972496929, 5.977527482382998691 ) ) ;
#61624 = FACE_OUTER_BOUND ( 'NONE', #30598, .T. ) ;
#61625 = CARTESIAN_POINT ( 'NONE',  ( -11.53412672884717871, -19.92380006517282709, -1.500000000000002220 ) ) ;
#61626 = DATE_TIME_ROLE ( 'classification_date' ) ;
#61627 = CARTESIAN_POINT ( 'NONE',  ( -75.62287095715005592, -23.47593901973091235, -1.443836447539004642 ) ) ;
#61628 = CARTESIAN_POINT ( 'NONE',  ( 4.647438682898014761, -6.376774720514417183, 20.26932200457894950 ) ) ;
#61629 = CARTESIAN_POINT ( 'NONE',  ( -121.5192058621623090, -24.35071581493543746, 9.817618358456025263 ) ) ;
#61630 = CARTESIAN_POINT ( 'NONE',  ( -101.5351826556731254, -25.12726549548206023, 7.135831474093189186 ) ) ;
#61631 = CARTESIAN_POINT ( 'NONE',  ( -109.3900273060415316, -25.26106641928794971, 3.961258450193692493 ) ) ;
#61632 = CARTESIAN_POINT ( 'NONE',  ( -129.5219158117283769, -24.34968618360934300, 0.1864209137778921610 ) ) ;
#61633 = CARTESIAN_POINT ( 'NONE',  ( -99.60745734687597519, -25.26400877198413042, 4.898549832726014408 ) ) ;
#61634 = CARTESIAN_POINT ( 'NONE',  ( 19.12242951303546334, 5.485007674754557527, -1.500000000000002220 ) ) ;
#61635 = CARTESIAN_POINT ( 'NONE',  ( 1.754398552524170762, 17.92127466780477718, 9.000000000000000000 ) ) ;
#61636 = CARTESIAN_POINT ( 'NONE',  ( 19.75791096855702733, 1.210928449428283038, -1.500000000000002220 ) ) ;
#61637 = CARTESIAN_POINT ( 'NONE',  ( -56.62367352497894757, -24.65952944569304250, 1.056160979905696795 ) ) ;
#61638 = ADVANCED_FACE ( 'NONE', ( #66093 ), #51842, .T. ) ;
#61639 = CARTESIAN_POINT ( 'NONE',  ( -39.14342005660770241, -25.29116703577911807, 3.683763317769410683 ) ) ;
#61640 = DIRECTION ( 'NONE',  ( -3.773278334453079618E-23, 0.9999999999976377785, 2.173523156925979975E-06 ) ) ;
#61641 = CARTESIAN_POINT ( 'NONE',  ( 17.59156710592704442, 10.99281682905060897, 11.49999999999999645 ) ) ;
#61642 = PLANE ( 'NONE',  #12700 ) ;
#61644 = ADVANCED_FACE ( 'NONE', ( #97990 ), #75163, .F. ) ;
#61643 = AXIS2_PLACEMENT_3D ( 'NONE', #14478, #55057, #69274 ) ;
#61645 = DIRECTION ( 'NONE',  ( 0.000000000000000000, 0.000000000000000000, 1.000000000000000000 ) ) ;
#61646 = CARTESIAN_POINT ( 'NONE',  ( -22.07869367785253090, -5.390224856484156390, 11.49999999999999645 ) ) ;
#61647 = ORIENTED_EDGE ( 'NONE', *, *, #22981, .T. ) ;
#61648 = LINE ( 'NONE', #83965, #33308 ) ;
#61649 = CARTESIAN_POINT ( 'NONE',  ( -28.52287095715005805, -24.49893655963190042, 1.056161680022248195 ) ) ;
#61650 = CARTESIAN_POINT ( 'NONE',  ( 19.91930514195032487, 3.327535025408205893, -1.500000000000002220 ) ) ;
#61651 = CARTESIAN_POINT ( 'NONE',  ( 9.058420110819382032, -0.8999999999999999112, -3.692441080025381961 ) ) ;
#61652 = CARTESIAN_POINT ( 'NONE',  ( -45.62287095715005592, -23.48786465467240703, 11.44779295918255002 ) ) ;
#61653 = ORIENTED_EDGE ( 'NONE', *, *, #60918, .T. ) ;
#61654 = VERTEX_POINT ( 'NONE', #77651 ) ;
#61655 = CARTESIAN_POINT ( 'NONE',  ( -0.1037292527911751056, -5.876774720514413630, 19.53657742262743824 ) ) ;
#61656 = CARTESIAN_POINT ( 'NONE',  ( 15.01570752033863165, -17.30494853738164096, -1.500000000000002220 ) ) ;
#61657 = CARTESIAN_POINT ( 'NONE',  ( -41.31104052750491462, -25.16585682362166310, 3.095323067379869730 ) ) ;
#61658 = VECTOR ( 'NONE', #91766, 1000.000000000000000 ) ;
#61659 = CARTESIAN_POINT ( 'NONE',  ( 7.158504886898216846, -20.39052948596947346, -1.500000000000002220 ) ) ;
#61660 = CARTESIAN_POINT ( 'NONE',  ( -123.5222519537087464, -23.48783264082477373, -1.443836473390086361 ) ) ;
#61661 = CARTESIAN_POINT ( 'NONE',  ( -34.60964202172039705, -23.73766607897670866, -1.055555164236443133 ) ) ;
#61662 = B_SPLINE_CURVE_WITH_KNOTS ( 'NONE', 3,
 ( #37310, #68257, #99185, #60656, #91578, #78344, #56040, #10347, #15946, #39291, #41301, #87472, #25062, #1247 ),
 .UNSPECIFIED., .F., .F.,
 ( 4, 2, 2, 2, 2, 2, 4 ),
 ( 0.000000000000000000, 0.0001905927013275506747, 0.0003811854026551013495, 0.0007623708053102105052, 0.001143556207965319444, 0.001334148909292864373, 0.001524741610620409084 ),
 .UNSPECIFIED. ) ;
#61663 = CARTESIAN_POINT ( 'NONE',  ( 20.89859092893058801, 0.06103081833375877813, 11.49999999999999645 ) ) ;
#61664 = ORIENTED_EDGE ( 'NONE', *, *, #73734, .F. ) ;
#61665 = AXIS2_PLACEMENT_3D ( 'NONE', #50539, #79983, #88607 ) ;
#61666 = CARTESIAN_POINT ( 'NONE',  ( -124.5909689015293367, -23.73766607897671577, -1.055555164236449572 ) ) ;
#61667 = CARTESIAN_POINT ( 'NONE',  ( 2.959355296939036872, -21.81356824310248399, 11.49999999999998934 ) ) ;
#61669 = CARTESIAN_POINT ( 'NONE',  ( -105.5186459176268983, -23.85049219812686871, 10.88485053497526955 ) ) ;
#61668 = CIRCLE ( 'NONE', #68106, 19.00000000000000000 ) ;
#61670 = DIRECTION ( 'NONE',  ( -3.773278334444167608E-23, 1.000000000000000000, 0.000000000000000000 ) ) ;
#61671 = ORIENTED_EDGE ( 'NONE', *, *, #57077, .T. ) ;
#61672 = CARTESIAN_POINT ( 'NONE',  ( 4.967948717948723392, -6.376774720514415407, 20.00140224358974095 ) ) ;
#61673 = FACE_OUTER_BOUND ( 'NONE', #10866, .T. ) ;
#61674 = ORIENTED_EDGE ( 'NONE', *, *, #4776, .F. ) ;
#61675 = CARTESIAN_POINT ( 'NONE',  ( -72.58096329547595360, -24.66019654487199730, 8.947790411086121054 ) ) ;
#61676 = ORIENTED_EDGE ( 'NONE', *, *, #22168, .F. ) ;
#61677 = VERTEX_POINT ( 'NONE', #41 ) ;
#61678 = CYLINDRICAL_SURFACE ( 'NONE', #20991, 1.000000000000000444 ) ;
#61679 = CARTESIAN_POINT ( 'NONE',  ( -95.62287095715007013, -23.48786465467241769, 11.44779295918254114 ) ) ;
#61680 = CARTESIAN_POINT ( 'NONE',  ( -36.50467997377245410, -23.96119346886880308, -0.6495511937832127991 ) ) ;
#61681 = CARTESIAN_POINT ( 'NONE',  ( 19.60162835767302880, 5.811842276320244416, -1.500000000000002220 ) ) ;
#61682 = ORIENTED_EDGE ( 'NONE', *, *, #94146, .F. ) ;
#61683 = CARTESIAN_POINT ( 'NONE',  ( -2.872281323269014752, -1.473225279485573358, 1.999999999999999556 ) ) ;
#61684 = CARTESIAN_POINT ( 'NONE',  ( 9.150000000000007461, -6.376774720514426953, 11.88602120139451834 ) ) ;
#61685 = CARTESIAN_POINT ( 'NONE',  ( 14.43441819135929194, 3.316774720514426456, -28.36222020317710957 ) ) ;
#61686 = CARTESIAN_POINT ( 'NONE',  ( 17.40631026334068565, 13.93540124644318645, -1.500000000000002220 ) ) ;
#61687 = LINE ( 'NONE', #37834, #35130 ) ;
#61688 = CARTESIAN_POINT ( 'NONE',  ( -51.58953762381672448, -24.64965694238407323, 8.947790433994656567 ) ) ;
#61689 = ORIENTED_EDGE ( 'NONE', *, *, #72996, .F. ) ;
#61690 = CARTESIAN_POINT ( 'NONE',  ( -27.79962520430046524, -24.61258123373733753, 1.630330808770078743 ) ) ;
#61691 = CARTESIAN_POINT ( 'NONE',  ( -28.41099462919338237, -25.26248047940597985, 8.118937510302929539 ) ) ;
#61692 = CARTESIAN_POINT ( 'NONE',  ( 15.94631523246878579, 13.42178585792578360, -1.500000000000002220 ) ) ;
#61693 = ORIENTED_EDGE ( 'NONE', *, *, #88458, .T. ) ;
#61695 = ORIENTED_EDGE ( 'NONE', *, *, #93777, .F. ) ;
#61694 = CARTESIAN_POINT ( 'NONE',  ( -42.52287095715005449, -23.73934037231755667, 11.05740245334330041 ) ) ;
#61696 = PLANE ( 'NONE',  #81111 ) ;
#61697 = ORIENTED_EDGE ( 'NONE', *, *, #8924, .T. ) ;
#61698 = ORIENTED_EDGE ( 'NONE', *, *, #77577, .T. ) ;
#61699 = DIRECTION ( 'NONE',  ( 1.000000000000000000, 3.773278334444167608E-23, 8.201307833595939069E-29 ) ) ;
#61701 = ADVANCED_FACE ( 'NONE', ( #60956 ), #22854, .T. ) ;
#61700 = CARTESIAN_POINT ( 'NONE',  ( 10.34999999999999254, 3.499999999999995115, 0.000000000000000000 ) ) ;
#61702 = LINE ( 'NONE', #77890, #84177 ) ;
#61703 = CARTESIAN_POINT ( 'NONE',  ( -108.9952638098694990, -25.25813793666175755, 3.818317156516219502 ) ) ;
#61704 = CARTESIAN_POINT ( 'NONE',  ( -53.62287095715004881, -23.48783264082478084, -1.443836473390070596 ) ) ;
#61706 = ORIENTED_EDGE ( 'NONE', *, *, #91269, .F. ) ;
#61705 = CARTESIAN_POINT ( 'NONE',  ( 22.20243239366838850, -0.07139729354238147363, 11.49999999999999645 ) ) ;
#61707 = CARTESIAN_POINT ( 'NONE',  ( -5.366453405989236813, 0.000000000000000000, 24.00000000000000000 ) ) ;
#61708 = ORIENTED_EDGE ( 'NONE', *, *, #60363, .T. ) ;
#61709 = EDGE_CURVE ( 'NONE', #74792, #55598, #39096, .T. ) ;
#61710 = CARTESIAN_POINT ( 'NONE',  ( 0.4201012023153268271, 22.63755686032812164, -1.500000000000002220 ) ) ;
#61711 = EDGE_CURVE ( 'NONE', #63420, #87407, #23865, .T. ) ;
#61713 = ORIENTED_EDGE ( 'NONE', *, *, #61849, .F. ) ;
#61712 = CARTESIAN_POINT ( 'NONE',  ( -115.5935066442949619, -23.85049219812686871, 10.88485053497526778 ) ) ;
#61714 = ADVANCED_FACE ( 'NONE', ( #62961 ), #13413, .T. ) ;
#61715 = VERTEX_POINT ( 'NONE', #72567 ) ;
#61716 = EDGE_CURVE ( 'NONE', #34088, #14044, #13518, .T. ) ;
#61717 = FACE_OUTER_BOUND ( 'NONE', #78444, .T. ) ;
#61718 = B_SPLINE_CURVE_WITH_KNOTS ( 'NONE', 3,
 ( #30672, #90084, #51528, #12942 ),
 .UNSPECIFIED., .F., .F.,
 ( 4, 4 ),
 ( 0.000000000000000000, 9.999999999997510880E-05 ),
 .UNSPECIFIED. ) ;
#61719 = AXIS2_PLACEMENT_3D ( 'NONE', #38210, #85891, #54448 ) ;
#61720 = CARTESIAN_POINT ( 'NONE',  ( -15.79248070760165490, 12.47733877207048181, -1.500000000000002220 ) ) ;
#61721 = DIRECTION ( 'NONE',  ( 0.000000000000000000, -1.000000000000000000, -1.020425574104004246E-16 ) ) ;
#61722 = EDGE_LOOP ( 'NONE', ( #75287, #83127, #95992, #84183 ) ) ;
#61723 = DIRECTION ( 'NONE',  ( 0.000000000000000000, -0.9999999999976377785, -2.173523156925979128E-06 ) ) ;
#61724 = CARTESIAN_POINT ( 'NONE',  ( 2.183928509170398602, -22.20744181112294413, -1.500000000000002220 ) ) ;
#61725 = EDGE_CURVE ( 'NONE', #24459, #41863, #10903, .T. ) ;
#61726 = ORIENTED_EDGE ( 'NONE', *, *, #24452, .F. ) ;
#61727 = EDGE_LOOP ( 'NONE', ( #82917, #65744, #31806, #83585 ) ) ;
#61728 = CARTESIAN_POINT ( 'NONE',  ( -101.1944152955115044, -25.25341239125477344, 6.858245852482038885 ) ) ;
#61729 = CARTESIAN_POINT ( 'NONE',  ( -119.6228709571500701, -24.50321055353803246, 9.387540953477515160 ) ) ;
#61730 = CARTESIAN_POINT ( 'NONE',  ( -58.52287095715006160, -29.50250243563736774, 8.947779886222145151 ) ) ;
#61731 = CARTESIAN_POINT ( 'NONE',  ( 31.84105487026623393, 5.152774720514427642, -11.95870468328481806 ) ) ;
#61732 = EDGE_CURVE ( 'NONE', #55816, #96695, #88290, .T. ) ;
#61733 = CARTESIAN_POINT ( 'NONE',  ( 14.76093561896379214, -3.316774720514426456, -26.55548769130089681 ) ) ;
#61734 = AXIS2_PLACEMENT_3D ( 'NONE', #82422, #90536, #21018 ) ;
#61735 = CARTESIAN_POINT ( 'NONE',  ( 19.09806219120973125, -4.162641619376711510, -1.500000000000002220 ) ) ;
#61736 = CARTESIAN_POINT ( 'NONE',  ( -5.205649524681222218, -5.876774720514407413, 19.16400979764067714 ) ) ;
#61737 = AXIS2_PLACEMENT_3D ( 'NONE', #86755, #1024, #40597 ) ;
#61738 = CARTESIAN_POINT ( 'NONE',  ( -21.47443924280258187, -0.1944818460393343829, -1.500000000000002220 ) ) ;
#61739 = CARTESIAN_POINT ( 'NONE',  ( -2.599001758237162285, -5.876774720514411854, 19.60308799987317485 ) ) ;
#61740 = CARTESIAN_POINT ( 'NONE',  ( 15.58962545129234556, 1.684774720514426560, -26.91365498785467736 ) ) ;
#61741 = CARTESIAN_POINT ( 'NONE',  ( -15.54901181048698255, -6.376774720514426953, -55.62515100798455592 ) ) ;
#61742 = CARTESIAN_POINT ( 'NONE',  ( -68.62287095715011276, -23.95044443724992789, 10.65354141964649415 ) ) ;
#61743 = CARTESIAN_POINT ( 'NONE',  ( 16.68310095749102118, 15.68496000196893370, -1.500000000000002220 ) ) ;
#61744 = PERSON_AND_ORGANIZATION ( #70597, #27821 ) ;
#61745 = CARTESIAN_POINT ( 'NONE',  ( -91.15361000704997707, -29.50249591506787894, 5.947779886229223045 ) ) ;
#61746 = DIRECTION ( 'NONE',  ( 0.1254312216594016816, 0.000000000000000000, 0.9921023176230514551 ) ) ;
#61747 = CARTESIAN_POINT ( 'NONE',  ( 11.63622169266987783, 16.31392799894670631, 11.49999999999999645 ) ) ;
#61748 = CARTESIAN_POINT ( 'NONE',  ( -78.94416233434603214, -25.26612682183856862, 5.924886500966431768 ) ) ;
#61749 = CARTESIAN_POINT ( 'NONE',  ( -113.5228709571500616, -24.64965694238408034, 8.947790433994192938 ) ) ;
#61750 = CARTESIAN_POINT ( 'NONE',  ( 4.588387839717440464, -5.876774720514402084, 18.52756237589653665 ) ) ;
#61751 = CARTESIAN_POINT ( 'NONE',  ( -24.57525087998974200, -0.3587747205143967943, -15.45548830044932664 ) ) ;
#61752 = ORIENTED_EDGE ( 'NONE', *, *, #11539, .T. ) ;
#61753 = FACE_OUTER_BOUND ( 'NONE', #93634, .T. ) ;
#61754 = EDGE_CURVE ( 'NONE', #45760, #40197, #96801, .T. ) ;
#61755 = CARTESIAN_POINT ( 'NONE',  ( -109.0885707575500447, -25.22089525921357733, 3.567658405505949482 ) ) ;
#61756 = CARTESIAN_POINT ( 'NONE',  ( -21.25272785503416273, -4.502612752106283978, -1.500000000000002220 ) ) ;
#61757 = DIRECTION ( 'NONE',  ( 1.000000000000000000, 0.000000000000000000, 0.000000000000000000 ) ) ;
#61758 = CARTESIAN_POINT ( 'NONE',  ( -18.14765110722914798, -7.448729197826248871, -1.500000000000002220 ) ) ;
#61759 = CARTESIAN_POINT ( 'NONE',  ( -128.5895376238167103, -24.64898659630529565, 1.056161002820832806 ) ) ;
#61760 = CARTESIAN_POINT ( 'NONE',  ( -109.3602963299949806, -25.27925676388351306, 4.255031605239652848 ) ) ;
#61761 = CARTESIAN_POINT ( 'NONE',  ( -91.62825878037952521, -24.35071581493543391, 9.817618358456023486 ) ) ;
#61762 = CARTESIAN_POINT ( 'NONE',  ( -47.52287095715007581, -23.72773821059537269, 11.05748984161097326 ) ) ;
#61763 = CARTESIAN_POINT ( 'NONE',  ( 2.947869850540926429, 20.32360706268488215, 11.49999999999999645 ) ) ;
#61764 = DIRECTION ( 'NONE',  ( 0.9951627101165076983, 0.000000000000000000, 0.09824042138329622254 ) ) ;
#61765 = CARTESIAN_POINT ( 'NONE',  ( -120.6235064633471268, -25.00158670708911046, 2.256160236439219258 ) ) ;
#61766 = VERTEX_POINT ( 'NONE', #89284 ) ;
#61767 = EDGE_CURVE ( 'NONE', #16991, #39655, #27388, .T. ) ;
#61768 = CARTESIAN_POINT ( 'NONE',  ( -46.62287095715004170, -23.48783264082478439, -1.443836473390070818 ) ) ;
#61769 = LINE ( 'NONE', #77459, #39640 ) ;
#61770 = CARTESIAN_POINT ( 'NONE',  ( -125.5545351961102369, -24.73531770709095312, 8.716586749053508498 ) ) ;
#61771 = CARTESIAN_POINT ( 'NONE',  ( 0.000000000000000000, 1.682774720514426114, 0.000000000000000000 ) ) ;
#61772 = EDGE_CURVE ( 'NONE', #51486, #92435, #59841, .T. ) ;
#61773 = CARTESIAN_POINT ( 'NONE',  ( -25.59878527050454622, -24.93063146600816538, 6.005086248586695596 ) ) ;
#61774 = CARTESIAN_POINT ( 'NONE',  ( 32.76524810979199742, 3.299944812882172229, -3.892744026461423701 ) ) ;
#61775 = CARTESIAN_POINT ( 'NONE',  ( 19.24196208499951055, 12.69117723712289703, 11.49999999999999645 ) ) ;
#61776 = CARTESIAN_POINT ( 'NONE',  ( 2.581029390964978187, -22.66945732913600509, 11.49999999999998934 ) ) ;
#61777 = CARTESIAN_POINT ( 'NONE',  ( -74.63881430719601440, -23.96119346886880308, -0.6495511937832119109 ) ) ;
#61778 = CARTESIAN_POINT ( 'NONE',  ( -5.293508136514246232, -6.376774720514408301, 19.18727597066021318 ) ) ;
#61779 = CARTESIAN_POINT ( 'NONE',  ( -104.6228709571500559, -24.66019654487200086, 8.947790411086124607 ) ) ;
#61780 = CARTESIAN_POINT ( 'NONE',  ( 20.53814608839396527, -8.957171556794316203, 11.49999999999999645 ) ) ;
#61781 = ORIENTED_EDGE ( 'NONE', *, *, #8875, .F. ) ;
#61782 = CARTESIAN_POINT ( 'NONE',  ( -29.52287095715006870, -23.40099448348795264, -1.443836171194820883 ) ) ;
#61783 = CARTESIAN_POINT ( 'NONE',  ( -43.60777470970129599, -23.73766607897671221, -1.055555164236442689 ) ) ;
#61784 = VECTOR ( 'NONE', #50880, 1000.000000000000000 ) ;
#61785 = CARTESIAN_POINT ( 'NONE',  ( 17.58553779993395594, 13.13030503331179411, -1.500000000000002220 ) ) ;
#61786 = APPROVAL ( #93182, 'UNKNOWN' ) ;
#61787 = CARTESIAN_POINT ( 'NONE',  ( -5.457842845122470976, -5.876774720514410077, 19.25892998154168367 ) ) ;
#61788 = CARTESIAN_POINT ( 'NONE',  ( -15.82668884360736961, 5.965225279485572685, 42.07822029717483758 ) ) ;
#61789 = CARTESIAN_POINT ( 'NONE',  ( -104.5858024219328399, -24.65952944569305316, 1.056160979905702346 ) ) ;
#61790 = CARTESIAN_POINT ( 'NONE',  ( -78.52212890984405647, -23.48783264082477018, -1.443836473390096797 ) ) ;
#61791 = CARTESIAN_POINT ( 'NONE',  ( -91.52287095715006160, -29.50248528299804818, 1.056150453629040253 ) ) ;
#61792 = ORIENTED_EDGE ( 'NONE', *, *, #16817, .F. ) ;
#61793 = CARTESIAN_POINT ( 'NONE',  ( -20.16212974941129588, 3.559051167911782887, -1.500000000000002220 ) ) ;
#61794 = ORIENTED_EDGE ( 'NONE', *, *, #88594, .T. ) ;
#61795 = ORIENTED_EDGE ( 'NONE', *, *, #61964, .T. ) ;
#61796 = ORIENTED_EDGE ( 'NONE', *, *, #8785, .F. ) ;
#61797 = EDGE_LOOP ( 'NONE', ( #79289, #97314, #63301, #100126, #17477, #41716, #69202, #86766, #15472, #42964, #96327, #78883, #59295, #50884, #43369, #16318, #21820, #22549, #58337, #45586, #70552, #68250, #68695, #56790, #83745 ) ) ;
#61798 = CARTESIAN_POINT ( 'NONE',  ( 7.103900956763240515, -21.94381868531750968, 11.49999999999998934 ) ) ;
#61799 = CARTESIAN_POINT ( 'NONE',  ( -82.52287095715006160, -23.72747288104470087, -1.053458166803226126 ) ) ;
#61800 = CARTESIAN_POINT ( 'NONE',  ( 19.35245777310151993, -6.127589836641541332, -1.500000000000002220 ) ) ;
#61801 = VERTEX_POINT ( 'NONE', #43115 ) ;
#61802 = CARTESIAN_POINT ( 'NONE',  ( -79.11611000704996854, -25.14083923594767001, 2.947789366383933185 ) ) ;
#61803 = CARTESIAN_POINT ( 'NONE',  ( -92.55803704003275811, -23.73766607897670866, -1.055555164236430032 ) ) ;
#61805 = CARTESIAN_POINT ( 'NONE',  ( -8.160000000000000142, -2.191226316053958875E-18, 2.701633758479787833E-17 ) ) ;
#61804 = VECTOR ( 'NONE', #67475, 1000.000000000000000 ) ;
#61806 = CARTESIAN_POINT ( 'NONE',  ( -70.58423775607164430, -24.73486907724917572, 1.287355809206963908 ) ) ;
#61808 = ORIENTED_EDGE ( 'NONE', *, *, #13626, .F. ) ;
#61807 = CARTESIAN_POINT ( 'NONE',  ( 13.13055478438326773, -17.03443908202477886, 11.49999999999999645 ) ) ;
#61809 = DIRECTION ( 'NONE',  ( 0.000000000000000000, -2.173523156925979552E-06, 0.9999999999976378895 ) ) ;
#61810 = CARTESIAN_POINT ( 'NONE',  ( -61.49888431235496000, -24.35071581493542681, 9.817618358456030592 ) ) ;
#61811 =( GEOMETRIC_REPRESENTATION_CONTEXT ( 3 ) GLOBAL_UNCERTAINTY_ASSIGNED_CONTEXT ( ( #98675 ) ) GLOBAL_UNIT_ASSIGNED_CONTEXT ( ( #84581, #46039, #76960 ) ) REPRESENTATION_CONTEXT ( 'NONE', 'WORKASPACE' ) );
#61812 = VERTEX_POINT ( 'NONE', #13139 ) ;
#61813 = CARTESIAN_POINT ( 'NONE',  ( 20.56943099487245519, -2.726235779781958968, 11.49999999999998934 ) ) ;
#61814 = B_SPLINE_CURVE_WITH_KNOTS ( 'NONE', 3,
 ( #30401, #61373, #45145, #7069 ),
 .UNSPECIFIED., .F., .F.,
 ( 4, 4 ),
 ( 2.818811872883924926E-06, 0.0004696340498052392208 ),
 .UNSPECIFIED. ) ;
#61815 = ORIENTED_EDGE ( 'NONE', *, *, #21035, .F. ) ;
#61817 = VERTEX_POINT ( 'NONE', #73563 ) ;
#61816 = CARTESIAN_POINT ( 'NONE',  ( -73.62287095715005592, -23.48783264082478084, -1.443836473390067487 ) ) ;
#61818 = DIRECTION ( 'NONE',  ( 1.000000000000000000, 0.000000000000000000, 0.000000000000000000 ) ) ;
#61819 = ORIENTED_EDGE ( 'NONE', *, *, #82634, .T. ) ;
#61820 = VERTEX_POINT ( 'NONE', #90779 ) ;
#61821 = CARTESIAN_POINT ( 'NONE',  ( 4.967948717948723392, -6.376774720514415407, 20.00140224358974095 ) ) ;
#61822 = FACE_OUTER_BOUND ( 'NONE', #82241, .T. ) ;
#61823 = CARTESIAN_POINT ( 'NONE',  ( -124.5228709571501327, -23.96177878511309345, 10.65340807706329507 ) ) ;
#61824 = CARTESIAN_POINT ( 'NONE',  ( -3.149188516569510377, 21.71089317892358395, 11.49999999999999645 ) ) ;
#61825 = CARTESIAN_POINT ( 'NONE',  ( -90.62287095715002749, -25.00182538069145366, 7.747789668545099317 ) ) ;
#61826 = CARTESIAN_POINT ( 'NONE',  ( 19.88857169258762170, 10.62688394266798930, 11.49999999999998934 ) ) ;
#61827 = CARTESIAN_POINT ( 'NONE',  ( -2.499008156623981236, -20.81284420272260860, 11.49999999999998934 ) ) ;
#61828 = CARTESIAN_POINT ( 'NONE',  ( -109.6485548560138312, -25.30376161434310234, 5.552256222609500469 ) ) ;
#61829 = CARTESIAN_POINT ( 'NONE',  ( 30.09341516180546350, 1.682774720514426114, -11.39311774897855756 ) ) ;
#61830 = ORIENTED_EDGE ( 'NONE', *, *, #92509, .F. ) ;
#61831 = EDGE_CURVE ( 'NONE', #79185, #17321, #74128, .T. ) ;
#61832 = ORIENTED_EDGE ( 'NONE', *, *, #21230, .F. ) ;
#61833 = ORIENTED_EDGE ( 'NONE', *, *, #29742, .F. ) ;
#61834 = EDGE_CURVE ( 'NONE', #71524, #47693, #13638, .T. ) ;
#61835 = PLANE ( 'NONE',  #53100 ) ;
#61836 = CARTESIAN_POINT ( 'NONE',  ( 20.53733210929814845, -6.371126427052321795, -1.500000000000002220 ) ) ;
#61837 = VECTOR ( 'NONE', #30741, 1000.000000000000114 ) ;
#61838 = CARTESIAN_POINT ( 'NONE',  ( -0.02075734969026423599, 6.376774720514426953, -0.08597719988137648983 ) ) ;
#61839 = VERTEX_POINT ( 'NONE', #82661 ) ;
#61840 = CARTESIAN_POINT ( 'NONE',  ( 17.61891135320703938, 11.69080507458975227, -1.500000000000002220 ) ) ;
#61841 = DIRECTION ( 'NONE',  ( -3.773278334453079030E-23, 0.9999999999976377785, 2.173523156925979128E-06 ) ) ;
#61842 = CARTESIAN_POINT ( 'NONE',  ( -60.72894938232060724, -25.20144863547804803, 6.835696751361012957 ) ) ;
#61843 = CARTESIAN_POINT ( 'NONE',  ( -83.59947989562338933, -23.73791477778912196, 11.05961554403170588 ) ) ;
#61844 = FACE_OUTER_BOUND ( 'NONE', #79193, .T. ) ;
#61845 = CARTESIAN_POINT ( 'NONE',  ( -47.62287095715004881, -24.50321055353803956, 9.387540953477536476 ) ) ;
#61846 = CARTESIAN_POINT ( 'NONE',  ( -7.471142097702432316, -20.87072022463130239, -1.500000000000002220 ) ) ;
#61847 = CARTESIAN_POINT ( 'NONE',  ( -71.54510427940205375, -24.34968618360933945, 0.1864209137778822800 ) ) ;
#61848 = B_SPLINE_CURVE_WITH_KNOTS ( 'NONE', 3,
 ( #40001, #39506, #93275, #54242 ),
 .UNSPECIFIED., .F., .F.,
 ( 4, 4 ),
 ( 0.4501073351080630003, 0.4591137663801785895 ),
 .UNSPECIFIED. ) ;
#61849 = EDGE_CURVE ( 'NONE', #81082, #97756, #92245, .T. ) ;
#61850 = ORIENTED_EDGE ( 'NONE', *, *, #95473, .T. ) ;
#61851 = CARTESIAN_POINT ( 'NONE',  ( -51.35838135674943317, -25.31633125061866352, 5.126937609008879626 ) ) ;
#61852 = CARTESIAN_POINT ( 'NONE',  ( -8.160000000000000142, -8.603846352786376883, -0.6978360589526751978 ) ) ;
#61853 = CARTESIAN_POINT ( 'NONE',  ( -126.5552529902581256, -24.34968618360934300, 0.1864209137778884418 ) ) ;
#61854 = B_SPLINE_CURVE_WITH_KNOTS ( 'NONE', 3,
 ( #62503, #37157, #29537, #76696, #92931, #53890, #7197, #68612, #77198, #7705, #38652, #45279 ),
 .UNSPECIFIED., .F., .F.,
 ( 4, 2, 2, 2, 2, 4 ),
 ( 0.000000000000000000, 0.0001514886653422532943, 0.0003029773306845065886, 0.0006059546613690202244, 0.0009089319920535340229, 0.001211909322738047821 ),
 .UNSPECIFIED. ) ;
#61855 = DIRECTION ( 'NONE',  ( -0.000000000000000000, 1.000000000000000000, -0.000000000000000000 ) ) ;
#61856 = CARTESIAN_POINT ( 'NONE',  ( 18.80106323769845389, 4.952424739525837616, 11.49999999999998934 ) ) ;
#61857 = CARTESIAN_POINT ( 'NONE',  ( -17.20161093224466953, -12.68000408521323408, -1.500000000000002220 ) ) ;
#61858 = CARTESIAN_POINT ( 'NONE',  ( -38.52287095715006870, -23.48786465467241058, 11.44779295918255180 ) ) ;
#61859 = CARTESIAN_POINT ( 'NONE',  ( -89.80332600318982372, -25.31973986624387862, 5.294390042787146200 ) ) ;
#61860 = VECTOR ( 'NONE', #89076, 1000.000000000000227 ) ;
#61861 = CARTESIAN_POINT ( 'NONE',  ( -46.62287095715004170, -23.48783264082478439, -1.443836473390070818 ) ) ;
#61862 = DIRECTION ( 'NONE',  ( -0.06486421869277853025, 0.000000000000000000, 0.9978940991575085961 ) ) ;
#61863 = CARTESIAN_POINT ( 'NONE',  ( -19.30582015231555104, -11.89196067722419237, -1.500000000000002220 ) ) ;
#61864 = DIRECTION ( 'NONE',  ( 0.000000000000000000, -0.000000000000000000, -1.000000000000000000 ) ) ;
#61865 = CARTESIAN_POINT ( 'NONE',  ( -97.52287095715006160, -24.64898659630367916, 1.056161002820829697 ) ) ;
#61866 = CARTESIAN_POINT ( 'NONE',  ( -19.84341114293531305, -1.032944114202840824, 11.49999999999999645 ) ) ;
#61867 = CARTESIAN_POINT ( 'NONE',  ( -73.62287095715005592, -23.47593901973091235, -1.443836447539006196 ) ) ;
#61868 = ORIENTED_EDGE ( 'NONE', *, *, #16428, .F. ) ;
#61869 = FACE_OUTER_BOUND ( 'NONE', #18526, .T. ) ;
#61870 = CARTESIAN_POINT ( 'NONE',  ( -6.377963355984652694, -6.376774720514411854, 19.53740760792478426 ) ) ;
#61872 = CARTESIAN_POINT ( 'NONE',  ( -7.160000000000000142, -6.754662360505034435, 7.925641719537454222 ) ) ;
#61871 = APPROVAL_PERSON_ORGANIZATION ( #37417, #78479, #14056 ) ;
#61873 = CARTESIAN_POINT ( 'NONE',  ( 8.597998336517790108, -19.88058937513707392, -1.500000000000002220 ) ) ;
#61874 = CARTESIAN_POINT ( 'NONE',  ( 9.150000000000000355, -5.876774720514426953, -15.70000000000000284 ) ) ;
#61875 = CARTESIAN_POINT ( 'NONE',  ( 19.43689267596983683, 0.5339526363925560792, -1.500000000000002220 ) ) ;
#61876 = CARTESIAN_POINT ( 'NONE',  ( -80.52287095715007581, -24.83620972994591014, 8.398175272781370992 ) ) ;
#61877 = DIRECTION ( 'NONE',  ( -0.000000000000000000, 2.173523156925979552E-06, -0.9999999999976378895 ) ) ;
#61878 = CARTESIAN_POINT ( 'NONE',  ( -9.134819693115781902, 17.59984377705169933, -1.500000000000002220 ) ) ;
#61879 = EDGE_CURVE ( 'NONE', #1347, #19743, #72851, .T. ) ;
#61880 = VECTOR ( 'NONE', #5691, 1000.000000000000000 ) ;
#61881 = ORIENTED_EDGE ( 'NONE', *, *, #52231, .T. ) ;
#61882 = APPROVAL_PERSON_ORGANIZATION ( #19047, #82954, #34288 ) ;
#61883 = CARTESIAN_POINT ( 'NONE',  ( 16.70477854660759931, 11.60849435585976153, 11.49999999999999645 ) ) ;
#61884 = CARTESIAN_POINT ( 'NONE',  ( -80.63530711448595412, -24.40034930558991277, 0.3402023900116063482 ) ) ;
#61885 = EDGE_CURVE ( 'NONE', #18367, #94148, #12145, .T. ) ;
#61886 = LINE ( 'NONE', #85201, #2734 ) ;
#61887 = VERTEX_POINT ( 'NONE', #74062 ) ;
#61888 = CARTESIAN_POINT ( 'NONE',  ( -30.59755354180557418, -24.77158516743337913, 8.907023374642857760 ) ) ;
#61889 = CARTESIAN_POINT ( 'NONE',  ( -119.4728709594060376, -25.21147767946275664, 8.000950760261451578 ) ) ;
#61890 = CARTESIAN_POINT ( 'NONE',  ( -101.5228709571500758, -29.50248528299804818, 1.056150453629042030 ) ) ;
#61891 = CARTESIAN_POINT ( 'NONE',  ( -40.53724472056929784, -24.52399227489126687, 9.353111116836521077 ) ) ;
#61892 = DIRECTION ( 'NONE',  ( 0.000000000000000000, 0.9999999999976377785, 2.173523156925979975E-06 ) ) ;
#61893 = CARTESIAN_POINT ( 'NONE',  ( 11.77038589110637901, 16.27938679534767275, -1.500000000000002220 ) ) ;
#61894 = CARTESIAN_POINT ( 'NONE',  ( 15.58962545129234556, -1.684774720514426560, -26.91365498785467736 ) ) ;
#61895 = ORIENTED_EDGE ( 'NONE', *, *, #61002, .F. ) ;
#61896 = CARTESIAN_POINT ( 'NONE',  ( -97.26334014122947735, -23.56000036390797092, -1.497999999999530374 ) ) ;
#61897 = CARTESIAN_POINT ( 'NONE',  ( -4.526818761702180893, -22.41603498850323817, 11.49999999999999645 ) ) ;
#61898 = CARTESIAN_POINT ( 'NONE',  ( -13.93578158028743985, 17.96481793202167054, 11.49999999999998934 ) ) ;
#61899 = VERTEX_POINT ( 'NONE', #26884 ) ;
#61900 = CARTESIAN_POINT ( 'NONE',  ( -53.62287095715007013, -23.73934037231756733, 11.05740245334329153 ) ) ;
#61901 = CARTESIAN_POINT ( 'NONE',  ( -53.62287095715005592, -29.50250243563736774, 8.947779886222146928 ) ) ;
#61902 = CARTESIAN_POINT ( 'NONE',  ( -38.60882062815987581, -23.73791477778911485, 11.05961554403170766 ) ) ;
#61903 = DIRECTION ( 'NONE',  ( 0.000000000000000000, -1.000000000000000000, 0.000000000000000000 ) ) ;
#61904 = EDGE_CURVE ( 'NONE', #56351, #89504, #49857, .T. ) ;
#61905 = LINE ( 'NONE', #38050, #7324 ) ;
#61906 = FACE_OUTER_BOUND ( 'NONE', #13119, .T. ) ;
#61907 = VERTEX_POINT ( 'NONE', #57855 ) ;
#61908 = CARTESIAN_POINT ( 'NONE',  ( 18.16468007720714795, -9.286844270591712913, 11.49999999999998934 ) ) ;
#61909 = EDGE_LOOP ( 'NONE', ( #97267, #19239, #14598, #69824 ) ) ;
#61910 = CARTESIAN_POINT ( 'NONE',  ( -12.06219892284564388, 19.56905390912838172, -1.500000000000002220 ) ) ;
#61911 = DIRECTION ( 'NONE',  ( -3.773278334444166432E-23, 1.000000000000000000, 0.000000000000000000 ) ) ;
#61913 = EDGE_LOOP ( 'NONE', ( #70743, #85135, #20015, #45416, #14885, #62539, #43303, #95541 ) ) ;
#61912 = EDGE_CURVE ( 'NONE', #31190, #14381, #63143, .T. ) ;
#61914 = CARTESIAN_POINT ( 'NONE',  ( 21.57151214508649772, 0.000000000000000000, -1.500000000000000666 ) ) ;
#61915 = CARTESIAN_POINT ( 'NONE',  ( -81.18457222299012699, -25.17491913618721355, 6.847625054176566195 ) ) ;
#61916 = CARTESIAN_POINT ( 'NONE',  ( -51.51435870162961095, -23.73791477778911840, 11.05961554403170766 ) ) ;
#61918 = VERTEX_POINT ( 'NONE', #20254 ) ;
#61917 = CARTESIAN_POINT ( 'NONE',  ( 21.10678091372558640, -2.468637549841573797, 11.49999999999999645 ) ) ;
#61919 = VERTEX_POINT ( 'NONE', #82165 ) ;
#61920 = CARTESIAN_POINT ( 'NONE',  ( 13.39142644571787422, -17.71860720625715757, -1.500000000000002220 ) ) ;
#61921 = AXIS2_PLACEMENT_3D ( 'NONE', #90327, #43171, #51776 ) ;
#61922 = CARTESIAN_POINT ( 'NONE',  ( -4.704028875484805639, -20.06825252194306941, -1.500000000000002220 ) ) ;
#61923 = EDGE_LOOP ( 'NONE', ( #79378, #27213, #2628, #100319 ) ) ;
#61924 = ORIENTED_EDGE ( 'NONE', *, *, #81691, .T. ) ;
#61925 = CARTESIAN_POINT ( 'NONE',  ( -112.6228709571500701, -24.33927499327855415, 9.819080762295817166 ) ) ;
#61926 = CARTESIAN_POINT ( 'NONE',  ( -68.92252889959623019, -25.25978459231412288, 3.590539514744167437 ) ) ;
#61927 = ORIENTED_EDGE ( 'NONE', *, *, #71347, .T. ) ;
#61928 = CARTESIAN_POINT ( 'NONE',  ( -0.02075734969026423599, -5.965225279485572685, -0.08597719988137648983 ) ) ;
#61929 = VERTEX_POINT ( 'NONE', #44110 ) ;
#61930 = CARTESIAN_POINT ( 'NONE',  ( -49.52287095715005449, -24.50321055353802890, 9.387540953477525818 ) ) ;
#61931 = EDGE_CURVE ( 'NONE', #15218, #55557, #59332, .T. ) ;
#61932 = PLANE ( 'NONE',  #21147 ) ;
#61933 = CARTESIAN_POINT ( 'NONE',  ( 20.80141654084381386, -1.409215765453083469, -1.500000000000002220 ) ) ;
#61934 = EDGE_CURVE ( 'NONE', #21450, #81557, #98378, .T. ) ;
#61935 = CARTESIAN_POINT ( 'NONE',  ( 1.472770742059883897, 21.73951962378590963, 11.49999999999999645 ) ) ;
#61936 = CARTESIAN_POINT ( 'NONE',  ( 25.17305609041493142, -5.157291146176350871, -8.664675380811843297 ) ) ;
#61937 = CARTESIAN_POINT ( 'NONE',  ( 10.45000000000000462, 1.999999999999998668, 24.00000000000000000 ) ) ;
#61938 = CARTESIAN_POINT ( 'NONE',  ( -22.32441756149717094, -2.617931739244098388, 11.49999999999998934 ) ) ;
#61939 = CARTESIAN_POINT ( 'NONE',  ( -38.61775694482038546, -23.48783264082477729, -1.443836473390076369 ) ) ;
#61940 = ORIENTED_EDGE ( 'NONE', *, *, #36640, .T. ) ;
#61941 = B_SPLINE_CURVE_WITH_KNOTS ( 'NONE', 3,
 ( #13279, #75180, #73697, #11792, #27530, #19896 ),
 .UNSPECIFIED., .F., .F.,
 ( 4, 2, 4 ),
 ( 1.570887131794333942E-05, 0.001396322306279761073, 0.002776935741241578874 ),
 .UNSPECIFIED. ) ;
#61942 = LINE ( 'NONE', #7645, #89038 ) ;
#61943 = VECTOR ( 'NONE', #5925, 1000.000000000000000 ) ;
#61944 = CARTESIAN_POINT ( 'NONE',  ( 13.91401389203221406, -0.3587747205144265483, 158.0376437107427137 ) ) ;
#61945 = LOCAL_TIME ( 0, 54, 15.00000000000000000, #99644 ) ;
#61946 = ORIENTED_EDGE ( 'NONE', *, *, #44602, .T. ) ;
#61947 = ORIENTED_EDGE ( 'NONE', *, *, #89084, .T. ) ;
#61948 = EDGE_CURVE ( 'NONE', #77573, #39962, #36353, .T. ) ;
#61949 = ORIENTED_EDGE ( 'NONE', *, *, #57042, .T. ) ;
#61950 = CARTESIAN_POINT ( 'NONE',  ( 12.02608574658498597, -17.65016651952024063, -1.500000000000002220 ) ) ;
#61951 = ADVANCED_FACE ( 'NONE', ( #67954 ), #46108, .T. ) ;
#61952 = ORIENTED_EDGE ( 'NONE', *, *, #98102, .F. ) ;
#61953 = CARTESIAN_POINT ( 'NONE',  ( 12.99892964944760543, 16.54660993828877125, -1.500000000000002220 ) ) ;
#61954 = CARTESIAN_POINT ( 'NONE',  ( -30.53009561173929143, -23.47879756175468557, -1.443836490256471983 ) ) ;
#61955 = LINE ( 'NONE', #92881, #80929 ) ;
#61956 = CARTESIAN_POINT ( 'NONE',  ( -61.58953762381671737, -23.48783264082478439, -1.443836473390069042 ) ) ;
#61957 = CARTESIAN_POINT ( 'NONE',  ( 12.93620265873104991, 17.78788284566447331, -1.500000000000002220 ) ) ;
#61958 = CARTESIAN_POINT ( 'NONE',  ( 3.300000000000004263, 0.000000000000000000, 0.000000000000000000 ) ) ;
#61959 = ORIENTED_EDGE ( 'NONE', *, *, #31679, .T. ) ;
#61960 = CARTESIAN_POINT ( 'NONE',  ( -71.30457154551152144, -29.50249648326654039, 6.209198155459374924 ) ) ;
#61961 = EDGE_CURVE ( 'NONE', #35718, #34952, #83656, .T. ) ;
#61962 = CARTESIAN_POINT ( 'NONE',  ( -107.5228709571501042, -23.47593901973090524, -1.443836447538996426 ) ) ;
#61963 = CARTESIAN_POINT ( 'NONE',  ( -19.76906661924035191, -6.534152953431121347, 11.49999999999999645 ) ) ;
#61964 = EDGE_CURVE ( 'NONE', #39283, #99333, #31374, .T. ) ;
#61965 = CARTESIAN_POINT ( 'NONE',  ( 31.68084058116295409, -4.801908866063379300, 29.09855526763849198 ) ) ;
#61966 = CARTESIAN_POINT ( 'NONE',  ( -108.6228709571499991, -24.51387760970724372, 9.387446482453409402 ) ) ;
#61967 = CARTESIAN_POINT ( 'NONE',  ( -30.58710530088973911, -25.14111132627482093, 7.291654623549845837 ) ) ;
#61968 = CARTESIAN_POINT ( 'NONE',  ( 4.979423480801214552, 20.69870207611912605, -1.500000000000002220 ) ) ;
#61969 = CARTESIAN_POINT ( 'NONE',  ( -31.24388727629348139, -25.01186361887644694, 7.715500679490839175 ) ) ;
#61970 = LINE ( 'NONE', #14769, #40028 ) ;
#61971 = CARTESIAN_POINT ( 'NONE',  ( -53.62287095715005592, -24.66019654487199375, 8.947790411086135265 ) ) ;
#61972 = CARTESIAN_POINT ( 'NONE',  ( -71.31538854159695973, -25.28687673834294003, 5.910757521653128066 ) ) ;
#61973 = CARTESIAN_POINT ( 'NONE',  ( 3.368619518803146029, -22.26131067175759881, -1.500000000000002220 ) ) ;
#61974 = AXIS2_PLACEMENT_3D ( 'NONE', #82419, #20024, #67720 ) ;
#61975 = B_SPLINE_SURFACE_WITH_KNOTS ( 'NONE', 3, 1, ( 
 ( #93362, #23853 ),
 ( #16250, #85763 ),
 ( #79144, #40093 ),
 ( #8643, #32477 ),
 ( #39588, #24857 ),
 ( #70540, #3540 ),
 ( #96877, #63961 ),
 ( #88272, #58328 ),
 ( #41102, #2539 ),
 ( #27368, #79642 ),
 ( #34979, #94869 ),
 ( #10643, #65458 ),
 ( #50706, #41605 ),
 ( #10139, #73055 ),
 ( #87770, #89265 ) ),
 .UNSPECIFIED., .F., .F., .F.,
 ( 4, 1, 1, 1, 1, 1, 1, 1, 1, 1, 1, 1, 4 ),
 ( 2, 2 ),
 ( 0.000000000000000000, 0.1128134007444583364, 0.2253938839207267619, 0.3395948145626991321, 0.4596754102248635232, 0.5217351900879312332, 0.5839258387389140159, 0.6481741447653686095, 0.7138810381130654692, 0.7810044549073892339, 0.8514509275565547153, 0.9240506926641780527, 0.9999999999999998890 ),
 ( 0.000000000000000000, 1.000000000000000000 ),
 .UNSPECIFIED. ) ;
#61976 = CARTESIAN_POINT ( 'NONE',  ( -110.9395002407040636, -25.32390614315827193, 4.358500768180118889 ) ) ;
#61977 = EDGE_LOOP ( 'NONE', ( #70122, #75187 ) ) ;
#61978 = CARTESIAN_POINT ( 'NONE',  ( -98.92287095715006728, -23.47593901973090524, -1.443836447538996648 ) ) ;
#61979 = CARTESIAN_POINT ( 'NONE',  ( -9.247272915838292917, -17.29429475886123768, 11.49999999999999645 ) ) ;
#61980 = CARTESIAN_POINT ( 'NONE',  ( -124.6228709571500559, -29.50250243563736774, 8.947779886222134493 ) ) ;
#61981 = CARTESIAN_POINT ( 'NONE',  ( -4.568292318365942073, 5.965225279485572685, 30.06720597538392425 ) ) ;
#61982 = ORIENTED_EDGE ( 'NONE', *, *, #73259, .T. ) ;
#61983 = CARTESIAN_POINT ( 'NONE',  ( -99.62727921284333377, -24.34968618360934300, 0.1864209137778966852 ) ) ;
#61984 = FACE_OUTER_BOUND ( 'NONE', #33608, .T. ) ;
#61985 = CARTESIAN_POINT ( 'NONE',  ( -89.90192472445558280, -25.25787539255926717, 3.590294762828090125 ) ) ;
#61986 = CARTESIAN_POINT ( 'NONE',  ( 3.912202881759007767, 19.34271161525698091, -1.500000000000002220 ) ) ;
#61987 = ORIENTED_EDGE ( 'NONE', *, *, #22477, .T. ) ;
#61988 = AXIS2_PLACEMENT_3D ( 'NONE', #96191, #11943, #88579 ) ;
#61989 = CARTESIAN_POINT ( 'NONE',  ( 8.655157120194559184, 6.376774720514430506, -28.10018424674326099 ) ) ;
#61990 = ADVANCED_FACE ( 'NONE', ( #30371 ), #62338, .T. ) ;
#61991 = PERSON_AND_ORGANIZATION ( #70597, #27821 ) ;
#61992 = ORIENTED_EDGE ( 'NONE', *, *, #33925, .F. ) ;
#61993 = PLANE ( 'NONE',  #9500 ) ;
#61994 = CARTESIAN_POINT ( 'NONE',  ( -48.62287095715004881, -24.64965695001467694, 8.947790433994185832 ) ) ;
#61995 = CARTESIAN_POINT ( 'NONE',  ( -11.16000000000000014, -10.15233964170348457, 0.003711184059992174607 ) ) ;
#61996 = CARTESIAN_POINT ( 'NONE',  ( 31.74473449900405697, -4.976825198871215328, -4.259190951192157293 ) ) ;
#61997 = CARTESIAN_POINT ( 'NONE',  ( 5.635247460261607166, -6.376774720514424288, 21.53093896358932469 ) ) ;
#61998 = DIRECTION ( 'NONE',  ( -0.000000000000000000, 1.000000000000000000, -0.000000000000000000 ) ) ;
#61999 = CARTESIAN_POINT ( 'NONE',  ( 3.787259615384621636, -6.376774720514404748, 18.51923076923076650 ) ) ;
#62000 = CARTESIAN_POINT ( 'NONE',  ( -7.473237707827510512, 18.53023608995856009, -1.500000000000002220 ) ) ;
#62001 = CARTESIAN_POINT ( 'NONE',  ( -50.62287095715005592, -23.48786465467241058, 11.44779295918255180 ) ) ;
#62002 = CARTESIAN_POINT ( 'NONE',  ( -45.48766593856211671, -24.52399227489127043, 9.353111116836528183 ) ) ;
#62003 = ORIENTED_EDGE ( 'NONE', *, *, #52294, .T. ) ;
#62004 = CIRCLE ( 'NONE', #73383, 2.499999999999998668 ) ;
#62006 = DIRECTION ( 'NONE',  ( 0.000000000000000000, 0.9999999999976377785, 2.173523156925979128E-06 ) ) ;
#62005 = LOCAL_TIME ( 0, 54, 15.00000000000000000, #38134 ) ;
#62007 = CARTESIAN_POINT ( 'NONE',  ( -109.7130628311247591, -25.18430198549888388, 3.499763365511714408 ) ) ;
#62008 = CARTESIAN_POINT ( 'NONE',  ( -35.56111601897774932, -23.85016227208580730, -0.8807180028928170978 ) ) ;
#62009 = CARTESIAN_POINT ( 'NONE',  ( -28.62287095715004526, -24.50732993938405357, 8.947790418389013567 ) ) ;
#62010 = DIRECTION ( 'NONE',  ( -0.000000000000000000, 1.000000000000000000, -0.000000000000000000 ) ) ;
#62011 = CARTESIAN_POINT ( 'NONE',  ( -83.50069094083774246, -24.65952944569304606, 1.056160979905700126 ) ) ;
#62012 = EDGE_CURVE ( 'NONE', #95021, #73142, #53064, .T. ) ;
#62013 = DIRECTION ( 'NONE',  ( -0.8788171126619707119, 0.4771587602595986910, -0.000000000000000000 ) ) ;
#62014 = AXIS2_PLACEMENT_3D ( 'NONE', #96811, #95808, #11565 ) ;
#62015 = EDGE_CURVE ( 'NONE', #7626, #40793, #68441, .T. ) ;
#62016 = CARTESIAN_POINT ( 'NONE',  ( 0.03625801282051022839, -5.876774720514410077, 19.27714342948718240 ) ) ;
#62017 = ORIENTED_EDGE ( 'NONE', *, *, #45259, .T. ) ;
#62018 = CARTESIAN_POINT ( 'NONE',  ( -12.21837793623082113, -16.16665877782589433, -1.500000000000002220 ) ) ;
#62019 = VECTOR ( 'NONE', #93632, 1000.000000000000114 ) ;
#62020 = B_SPLINE_CURVE_WITH_KNOTS ( 'NONE', 3,
 ( #42371, #89025, #2800, #33736 ),
 .UNSPECIFIED., .F., .F.,
 ( 4, 4 ),
 ( 0.000000000000000000, 0.0001000000000000167422 ),
 .UNSPECIFIED. ) ;
#62021 = CARTESIAN_POINT ( 'NONE',  ( -28.62287095715006657, -24.50666107542846461, 1.056161637124864550 ) ) ;
#62022 = EDGE_CURVE ( 'NONE', #62319, #33918, #36832, .T. ) ;
#62023 = CARTESIAN_POINT ( 'NONE',  ( -105.6228709571500275, -25.00158670708909625, 2.256160236439166411 ) ) ;
#62024 = EDGE_CURVE ( 'NONE', #100004, #17029, #30875, .T. ) ;
#62025 = ORIENTED_EDGE ( 'NONE', *, *, #77124, .F. ) ;
#62026 = CARTESIAN_POINT ( 'NONE',  ( -28.98875734969026396, 5.965225279485572685, 10.11402280011862587 ) ) ;
#62027 = CARTESIAN_POINT ( 'NONE',  ( -14.78635263257777233, 13.65558988533819473, -1.500000000000002220 ) ) ;
#62028 = CARTESIAN_POINT ( 'NONE',  ( 2.841100885065937387, 20.89556961663114265, 11.49999999999999645 ) ) ;
#62029 = EDGE_CURVE ( 'NONE', #7917, #76864, #54230, .T. ) ;
#62030 = CARTESIAN_POINT ( 'NONE',  ( 18.18892703665305177, -12.56521834855340281, 11.49999999999998934 ) ) ;
#62031 = CARTESIAN_POINT ( 'NONE',  ( -20.49763986188970932, -1.003951800832726615, 11.49999999999998934 ) ) ;
#62032 = PLANE ( 'NONE',  #10603 ) ;
#62033 = AXIS2_PLACEMENT_3D ( 'NONE', #54611, #16526, #316 ) ;
#62034 = FACE_OUTER_BOUND ( 'NONE', #83267, .T. ) ;
#62035 = ORIENTED_EDGE ( 'NONE', *, *, #55861, .T. ) ;
#62036 = CARTESIAN_POINT ( 'NONE',  ( -54.62287095715005592, -29.50250786944525672, 11.44777988621624054 ) ) ;
#62037 = ORIENTED_EDGE ( 'NONE', *, *, #82410, .T. ) ;
#62038 = DIRECTION ( 'NONE',  ( 0.000000000000000000, -1.000000000000000000, 0.000000000000000000 ) ) ;
#62039 = CARTESIAN_POINT ( 'NONE',  ( -85.62287095715008434, -24.63345952396257488, 9.038047939301511846 ) ) ;
#62040 = ORIENTED_EDGE ( 'NONE', *, *, #65617, .F. ) ;
#62041 = ORIENTED_EDGE ( 'NONE', *, *, #50882, .T. ) ;
#62042 = ORIENTED_EDGE ( 'NONE', *, *, #50484, .F. ) ;
#62043 = CARTESIAN_POINT ( 'NONE',  ( 19.75748517575715368, 0.3587747205144265483, 28.87153971905864580 ) ) ;
#62044 = CARTESIAN_POINT ( 'NONE',  ( 13.91401389203221406, 5.965225279485572685, 158.0376437107427137 ) ) ;
#62045 = CARTESIAN_POINT ( 'NONE',  ( 10.24059822343757808, -5.876774720514426953, 22.08128695274315945 ) ) ;
#62046 = CARTESIAN_POINT ( 'NONE',  ( -20.60850594246137035, -0.7621957659720622891, -1.500000000000002220 ) ) ;
#62047 = EDGE_CURVE ( 'NONE', #48068, #2401, #96915, .T. ) ;
#62048 = CARTESIAN_POINT ( 'NONE',  ( 20.07693369621832602, 7.961103810760662647, 11.49999999999999645 ) ) ;
#62049 = ORIENTED_EDGE ( 'NONE', *, *, #53619, .F. ) ;
#62050 = VECTOR ( 'NONE', #9760, 1000.000000000000114 ) ;
#62051 = CARTESIAN_POINT ( 'NONE',  ( -88.52287095715006160, -24.64898659630367916, 1.056161002820827921 ) ) ;
#62052 = FACE_OUTER_BOUND ( 'NONE', #28095, .T. ) ;
#62053 = CARTESIAN_POINT ( 'NONE',  ( -20.95026660567425481, -7.857139728745305973, 11.49999999999998934 ) ) ;
#62054 = CARTESIAN_POINT ( 'NONE',  ( -47.63366713346987069, -24.35071581493542325, 9.817618358456030592 ) ) ;
#62055 = CARTESIAN_POINT ( 'NONE',  ( 32.33217928425140997, 6.376774720514426953, -12.20610769812822483 ) ) ;
#62056 = VERTEX_POINT ( 'NONE', #29873 ) ;
#62057 = CARTESIAN_POINT ( 'NONE',  ( -99.52764846858842418, -25.27419814425944011, 3.999772249604663710 ) ) ;
#62058 = CARTESIAN_POINT ( 'NONE',  ( -49.66060423489871312, -23.48786465467241058, 11.44779295918254824 ) ) ;
#62059 = VECTOR ( 'NONE', #53634, 1000.000000000000227 ) ;
#62060 = DIRECTION ( 'NONE',  ( -3.773278334453079030E-23, 0.9999999999976377785, 2.173523156925979128E-06 ) ) ;
#62061 = CARTESIAN_POINT ( 'NONE',  ( 10.02768300834196502, -18.34552750054021786, -1.500000000000002220 ) ) ;
#62062 = ORIENTED_EDGE ( 'NONE', *, *, #31082, .T. ) ;
#62064 = EDGE_CURVE ( 'NONE', #92642, #41756, #60349, .T. ) ;
#62063 = CARTESIAN_POINT ( 'NONE',  ( -45.52287095715006160, -24.99156044556202616, 7.747789690856173195 ) ) ;
#62065 = ORIENTED_EDGE ( 'NONE', *, *, #80875, .T. ) ;
#62066 = DIRECTION ( 'NONE',  ( 0.000000000000000000, 0.000000000000000000, 1.000000000000000000 ) ) ;
#62067 = CARTESIAN_POINT ( 'NONE',  ( -10.94853654022341516, 18.13385389444049522, -1.500000000000002220 ) ) ;
#62068 = EDGE_CURVE ( 'NONE', #76713, #35613, #60844, .T. ) ;
#62069 = ORIENTED_EDGE ( 'NONE', *, *, #68327, .F. ) ;
#62070 = CARTESIAN_POINT ( 'NONE',  ( -50.48973103951670538, -24.52300882791529801, 0.6510814631126389251 ) ) ;
#62071 = B_SPLINE_CURVE_WITH_KNOTS ( 'NONE', 3,
 ( #89444, #74218, #19426, #59005, #65633, #96549 ),
 .UNSPECIFIED., .F., .F.,
 ( 4, 2, 4 ),
 ( 6.384118678610336992E-06, 0.001386860460828373684, 0.002767336802978137122 ),
 .UNSPECIFIED. ) ;
#62072 = CARTESIAN_POINT ( 'NONE',  ( 4.771108217193557266, 21.26182814020628697, 11.49999999999998934 ) ) ;
#62073 = CARTESIAN_POINT ( 'NONE',  ( -6.818021687177533430, -6.376774720514408301, 19.14905311829361167 ) ) ;
#62074 = CARTESIAN_POINT ( 'NONE',  ( -48.52287095715006160, -24.65952944569304606, 1.056160979905693686 ) ) ;
#62075 = CARTESIAN_POINT ( 'NONE',  ( -79.34891651374461219, -25.27186867375041857, 6.035758440376426393 ) ) ;
#62076 = CARTESIAN_POINT ( 'NONE',  ( -1.534710021792092594, -21.76038796025502009, -1.500000000000002220 ) ) ;
#62077 = CARTESIAN_POINT ( 'NONE',  ( -30.57287095715007297, -24.98095046702749755, 2.202836320189033081 ) ) ;
#62078 = ORIENTED_EDGE ( 'NONE', *, *, #67258, .F. ) ;
#62079 = CARTESIAN_POINT ( 'NONE',  ( -30.51964735150444241, -23.47802267728122416, 11.44779284538084241 ) ) ;
#62080 = CARTESIAN_POINT ( 'NONE',  ( -66.52287095715006160, -29.50248528299804818, 1.056150453629036701 ) ) ;
#62082 = ORIENTED_EDGE ( 'NONE', *, *, #48921, .F. ) ;
#62081 = EDGE_CURVE ( 'NONE', #40266, #37899, #93521, .T. ) ;
#62083 = EDGE_CURVE ( 'NONE', #63420, #67116, #90801, .T. ) ;
#62084 = EDGE_LOOP ( 'NONE', ( #92989, #2321, #39240, #41090 ) ) ;
#62085 = VECTOR ( 'NONE', #20797, 1000.000000000000114 ) ;
#62086 = EDGE_CURVE ( 'NONE', #99683, #51818, #43359, .T. ) ;
#62087 = ORIENTED_EDGE ( 'NONE', *, *, #82760, .T. ) ;
#62088 = APPROVAL_PERSON_ORGANIZATION ( #84572, #69216, #24173 ) ;
#62089 = DIRECTION ( 'NONE',  ( -3.773278334453079030E-23, 0.9999999999976377785, 2.173523156925979128E-06 ) ) ;
#62090 = CARTESIAN_POINT ( 'NONE',  ( -19.77875734969026311, -6.143225279485574397, 29.49402280011862487 ) ) ;
#62091 = CARTESIAN_POINT ( 'NONE',  ( 7.993063233546146229, -19.64520799392144568, -1.500000000000002220 ) ) ;
#62092 = CARTESIAN_POINT ( 'NONE',  ( -94.58633464317938433, -24.51314013834315375, 0.6176544820404151759 ) ) ;
#62093 = CARTESIAN_POINT ( 'NONE',  ( -79.32136430576915131, -25.03138187970275652, 7.049788599829707181 ) ) ;
#62094 = CARTESIAN_POINT ( 'NONE',  ( -59.62287095715004881, -24.66019654487199020, 8.947790411086131712 ) ) ;
#62095 = CARTESIAN_POINT ( 'NONE',  ( -12.64432969575899968, 0.3587747205143967943, -26.13179214487285407 ) ) ;
#62097 = CARTESIAN_POINT ( 'NONE',  ( 19.02374887324148389, -3.781047496429098764, 11.49999999999998934 ) ) ;
#62096 = AXIS2_PLACEMENT_3D ( 'NONE', #92151, #28268, #21632 ) ;
#62098 = EDGE_CURVE ( 'NONE', #89773, #79651, #59464, .T. ) ;
#62099 = CARTESIAN_POINT ( 'NONE',  ( -69.75924279648913284, -25.30665621374858532, 5.475492409637942259 ) ) ;
#62100 = ORIENTED_EDGE ( 'NONE', *, *, #40303, .F. ) ;
#62101 = CARTESIAN_POINT ( 'NONE',  ( -12.17249226084429203, 15.20430173202493940, 11.49999999999999645 ) ) ;
#62102 = LINE ( 'NONE', #22504, #21216 ) ;
#62103 = FACE_OUTER_BOUND ( 'NONE', #86235, .T. ) ;
#62104 = VERTEX_POINT ( 'NONE', #422 ) ;
#62105 = CARTESIAN_POINT ( 'NONE',  ( 3.632744579681756569, -6.376774720514402972, 18.17103827887095946 ) ) ;
#62106 = DIRECTION ( 'NONE',  ( 0.000000000000000000, 1.000000000000000000, 0.000000000000000000 ) ) ;
#62107 = CARTESIAN_POINT ( 'NONE',  ( -91.62287095715004170, -24.64965695001468404, 8.947790433994180503 ) ) ;
#62108 = CARTESIAN_POINT ( 'NONE',  ( -55.62287095715007013, -24.83602698348158810, 1.605859176311264847 ) ) ;
#62109 = CARTESIAN_POINT ( 'NONE',  ( 13.10555085358618221, -14.64361678476065087, 11.49999999999998934 ) ) ;
#62110 = B_SPLINE_SURFACE_WITH_KNOTS ( 'NONE', 3, 1, ( 
 ( #13022, #20144 ),
 ( #28763, #29253 ),
 ( #6916, #59726 ),
 ( #98760, #13522 ),
 ( #43500, #82542 ) ),
 .UNSPECIFIED., .F., .F., .F.,
 ( 4, 1, 4 ),
 ( 2, 2 ),
 ( 0.000000000000000000, 0.5078576360847800730, 1.000000000000000000 ),
 ( 0.000000000000000000, 1.000000000000000000 ),
 .UNSPECIFIED. ) ;
#62111 = CARTESIAN_POINT ( 'NONE',  ( 282.9764569301858046, -0.3587747205144265483, 20.79159422840526616 ) ) ;
#62112 = VERTEX_POINT ( 'NONE', #22242 ) ;
#62113 = CARTESIAN_POINT ( 'NONE',  ( 20.63042821663210091, 6.393326493806346100, -1.500000000000002220 ) ) ;
#62114 = CARTESIAN_POINT ( 'NONE',  ( -95.52287095715009002, -24.52323809116984421, 9.355190652339429036 ) ) ;
#62115 = CARTESIAN_POINT ( 'NONE',  ( -40.64478534806120535, -24.40034930558990922, 0.3402023900116037392 ) ) ;
#62116 = DIRECTION ( 'NONE',  ( -0.8264557562326033668, 6.845827386180409975E-16, -0.5630016722799281448 ) ) ;
#62117 = CARTESIAN_POINT ( 'NONE',  ( -17.14199295335891904, -15.44578658782692671, -1.500000000000002220 ) ) ;
#62118 = COORDINATED_UNIVERSAL_TIME_OFFSET ( 0, 0, .AHEAD. ) ;
#62119 = CARTESIAN_POINT ( 'NONE',  ( -93.50973692245648294, -24.34968618360934656, 0.1864209137778838343 ) ) ;
#62120 = CARTESIAN_POINT ( 'NONE',  ( 0.1334620785917008390, -8.769264156269324317, 8.999999999999998224 ) ) ;
#62121 = CARTESIAN_POINT ( 'NONE',  ( -121.6275764894026423, -23.48786465467241413, 11.44779295918253581 ) ) ;
#62122 = CARTESIAN_POINT ( 'NONE',  ( -64.62287095715005592, -24.66019654487198665, 8.947790411086131712 ) ) ;
#62123 = CARTESIAN_POINT ( 'NONE',  ( -109.4873253428160922, -25.23964128780368554, 3.732949821448104721 ) ) ;
#62124 = CARTESIAN_POINT ( 'NONE',  ( -129.5556841849855232, -24.65952944569305316, 1.056160979905705899 ) ) ;
#62125 = CARTESIAN_POINT ( 'NONE',  ( -99.12529836037420239, -25.31565907717662967, 4.049155208725341737 ) ) ;
#62126 = CARTESIAN_POINT ( 'NONE',  ( 19.57267778704439820, -3.578973306870405047, -1.500000000000002220 ) ) ;
#62127 = AXIS2_PLACEMENT_3D ( 'NONE', #87913, #93503, #48356 ) ;
#62128 = CARTESIAN_POINT ( 'NONE',  ( -118.5562042904833930, -23.48786465467241769, 11.44779295918253403 ) ) ;
#62129 = CARTESIAN_POINT ( 'NONE',  ( -2.735935421901279696, -19.66989661884619522, -1.500000000000002220 ) ) ;
#62130 = CARTESIAN_POINT ( 'NONE',  ( 0.3906119451836247425, -5.876774720514418071, 20.56083401959467594 ) ) ;
#62131 = CARTESIAN_POINT ( 'NONE',  ( -39.44256650533377950, -25.10925678386670157, 3.228028143694820606 ) ) ;
#62132 = CARTESIAN_POINT ( 'NONE',  ( -35.62287095715006302, -23.84081130438200091, 10.88220057463248835 ) ) ;
#62133 = CARTESIAN_POINT ( 'NONE',  ( 20.09396958936853395, 5.161349618257207617, 11.49999999999999645 ) ) ;
#62134 = CARTESIAN_POINT ( 'NONE',  ( 5.271800844963591359, 3.316774720514426456, -28.56638892015329034 ) ) ;
#62135 = CARTESIAN_POINT ( 'NONE',  ( -78.52287095715004739, -23.95044443724992078, 10.65354141964648704 ) ) ;
#62136 = CARTESIAN_POINT ( 'NONE',  ( 2.720868037236281012, -22.60253418658637869, 11.49999999999999645 ) ) ;
#62138 = ADVANCED_FACE ( 'NONE', ( #68939 ), #22743, .F. ) ;
#62137 = EDGE_LOOP ( 'NONE', ( #31761, #59911, #93139, #94147, #34589 ) ) ;
#62139 = CARTESIAN_POINT ( 'NONE',  ( -57.62287095715003460, -24.65952944569304606, 1.056160979905696573 ) ) ;
#62141 = ADVANCED_FACE ( 'NONE', ( #71452 ), #10536, .F. ) ;
#62140 = CARTESIAN_POINT ( 'NONE',  ( -92.52287095715007581, -24.50321055353804667, 9.387540953477515160 ) ) ;
#62142 = VERTEX_POINT ( 'NONE', #39493 ) ;
#62143 = CARTESIAN_POINT ( 'NONE',  ( -19.13055903301823335, -6.388282315271819556, 11.49999999999998934 ) ) ;
#62144 = LINE ( 'NONE', #85459, #54870 ) ;
#62145 = EDGE_CURVE ( 'NONE', #98626, #82004, #50989, .T. ) ;
#62146 = CARTESIAN_POINT ( 'NONE',  ( -95.62287095715004170, -24.51163499207176244, 0.6490370598554217052 ) ) ;
#62147 = ADVANCED_FACE ( 'NONE', ( #47613 ), #93770, .F. ) ;
#62148 = ORIENTED_EDGE ( 'NONE', *, *, #22363, .F. ) ;
#62149 = ADVANCED_FACE ( 'NONE', ( #64358 ), #17652, .F. ) ;
#62150 = EDGE_LOOP ( 'NONE', ( #45715, #70424, #89904, #71171 ) ) ;
#62151 = VECTOR ( 'NONE', #28017, 1000.000000000000000 ) ;
#62152 = CARTESIAN_POINT ( 'NONE',  ( -97.62287095715005592, -23.47593901973091235, -1.443836447539001089 ) ) ;
#62153 = CARTESIAN_POINT ( 'NONE',  ( -2.380104427745746154, 22.76713797270899065, 11.49999999999998934 ) ) ;
#62154 = CARTESIAN_POINT ( 'NONE',  ( -50.40445135320379677, -25.27420563080442406, 3.293942922663647632 ) ) ;
#62155 = CARTESIAN_POINT ( 'NONE',  ( 5.966611984012316405, 20.80180421262142687, -1.500000000000002220 ) ) ;
#62156 = DIRECTION ( 'NONE',  ( -3.773278334444167608E-23, 1.000000000000000000, 0.000000000000000000 ) ) ;
#62157 = CARTESIAN_POINT ( 'NONE',  ( 0.8316226063609513108, 20.92010288561657205, 11.49999999999999645 ) ) ;
#62158 = VERTEX_POINT ( 'NONE', #72450 ) ;
#62159 = EDGE_CURVE ( 'NONE', #96649, #34238, #58592, .T. ) ;
#62160 = CARTESIAN_POINT ( 'NONE',  ( -124.6242032400218704, -24.34968618360933945, 0.1864209137778899961 ) ) ;
#62161 = CARTESIAN_POINT ( 'NONE',  ( -21.99024891984110752, 1.279939690139831665, -1.500000000000002220 ) ) ;
#62162 = DIRECTION ( 'NONE',  ( -0.000000000000000000, 1.000000000000000000, -0.000000000000000000 ) ) ;
#62163 = CARTESIAN_POINT ( 'NONE',  ( -30.47287095715007865, -25.30734145635176802, 5.571384887382079043 ) ) ;
#62164 = ORIENTED_EDGE ( 'NONE', *, *, #57927, .T. ) ;
#62165 = CARTESIAN_POINT ( 'NONE',  ( 3.825381322105384285, -6.376774720514401196, 18.16071977647550995 ) ) ;
#62166 = CARTESIAN_POINT ( 'NONE',  ( -67.52287095715006160, -24.64898659630528854, 1.056161002820824368 ) ) ;
#62167 = VERTEX_POINT ( 'NONE', #79042 ) ;
#62168 = FACE_OUTER_BOUND ( 'NONE', #6402, .T. ) ;
#62169 = ORIENTED_EDGE ( 'NONE', *, *, #280, .F. ) ;
#62170 = VECTOR ( 'NONE', #94409, 1000.000000000000000 ) ;
#62171 = ORIENTED_EDGE ( 'NONE', *, *, #85339, .F. ) ;
#62172 = CARTESIAN_POINT ( 'NONE',  ( -71.55916567469419931, -23.73791477778911840, 11.05961554403170766 ) ) ;
#62173 = CARTESIAN_POINT ( 'NONE',  ( -101.5300974081266787, -25.10935923999858588, 3.391563287084827127 ) ) ;
#62174 = CARTESIAN_POINT ( 'NONE',  ( -4.743266218460161276, -6.376774720514413630, 19.49357334786887108 ) ) ;
#62175 = CARTESIAN_POINT ( 'NONE',  ( 18.81987132735423174, -8.002443037797982939, -1.500000000000002220 ) ) ;
#62176 = ADVANCED_FACE ( 'NONE', ( #63351 ), #35262, .T. ) ;
#62177 = ORIENTED_EDGE ( 'NONE', *, *, #82188, .T. ) ;
#62178 = CARTESIAN_POINT ( 'NONE',  ( -61.58953762381671737, -23.47596703998600276, 11.44779298504227505 ) ) ;
#62179 = CARTESIAN_POINT ( 'NONE',  ( -100.5228709571500616, -24.99132157543084531, 2.256160258750667502 ) ) ;
#62180 = DIRECTION ( 'NONE',  ( -1.000000000000000000, 0.000000000000000000, 1.895872651340772790E-16 ) ) ;
#62181 = CARTESIAN_POINT ( 'NONE',  ( 20.80681148587913754, 8.022540738981085440, -1.500000000000002220 ) ) ;
#62182 = CARTESIAN_POINT ( 'NONE',  ( 27.53860345374808105, 1.682774720514426114, -1.352392034746782823 ) ) ;
#62183 = CARTESIAN_POINT ( 'NONE',  ( -26.80445111962029614, -24.62944456348768796, 8.034172700478890761 ) ) ;
#62184 = EDGE_CURVE ( 'NONE', #55923, #75111, #27901, .T. ) ;
#62185 = VERTEX_POINT ( 'NONE', #66228 ) ;
#62186 = FACE_OUTER_BOUND ( 'NONE', #100212, .T. ) ;
#62187 = CARTESIAN_POINT ( 'NONE',  ( -29.77636857527935277, -25.26247541502187488, 5.788902928198627507 ) ) ;
#62188 = CARTESIAN_POINT ( 'NONE',  ( 3.748101851616784774, 20.49759516964078188, 11.49999999999998934 ) ) ;
#62189 = ORIENTED_EDGE ( 'NONE', *, *, #92398, .F. ) ;
#62192 = ORIENTED_EDGE ( 'NONE', *, *, #48393, .T. ) ;
#62191 = EDGE_CURVE ( 'NONE', #73552, #81441, #97152, .T. ) ;
#62190 = CARTESIAN_POINT ( 'NONE',  ( 3.825970207471427020, -6.376774720514402972, 18.52126221587801780 ) ) ;
#62193 = B_SPLINE_SURFACE_WITH_KNOTS ( 'NONE', 3, 3, ( 
 ( #18053, #11939, #3845, #80455 ),
 ( #34785, #65756, #72353, #10947 ),
 ( #2849, #26166, #49523, #41912 ),
 ( #96674, #27174, #58135, #34290 ),
 ( #58623, #73841, #4341, #35291 ),
 ( #66256, #89568, #76315, #13925 ),
 ( #44399, #67242, #91056, #91552 ) ),
 .UNSPECIFIED., .F., .F., .F.,
 ( 4, 3, 4 ),
 ( 4, 4 ),
 ( 0.0004766839783818044361, 0.1029713700210893312, 0.2054660560637968647 ),
 ( 0.8096999710875462108, 0.8110862897224703216 ),
 .UNSPECIFIED. ) ;
#62194 = CARTESIAN_POINT ( 'NONE',  ( -119.5228709571500758, -23.47596703998600631, 11.44779298504227860 ) ) ;
#62195 = CARTESIAN_POINT ( 'NONE',  ( 20.92198360912786015, -1.804805560479522342, -1.500000000000002220 ) ) ;
#62196 = ORIENTED_EDGE ( 'NONE', *, *, #19902, .F. ) ;
#62197 = CARTESIAN_POINT ( 'NONE',  ( -0.3059464777392844059, -8.530684776139525027, 8.999999999999998224 ) ) ;
#62198 = CARTESIAN_POINT ( 'NONE',  ( -55.62287095715004170, -24.99156045073392463, 7.747789690856161648 ) ) ;
#62199 = LINE ( 'NONE', #92625, #72408 ) ;
#62200 = DIRECTION ( 'NONE',  ( -3.773278334453079618E-23, 0.9999999999976377785, 2.173523156925979975E-06 ) ) ;
#62201 = CARTESIAN_POINT ( 'NONE',  ( -92.58613717802586507, -24.51419770103156281, 9.386484678747175181 ) ) ;
#62202 = CARTESIAN_POINT ( 'NONE',  ( -27.96875734969026084, -6.376774720514426953, -0.08597719988137648983 ) ) ;
#62204 = ORIENTED_EDGE ( 'NONE', *, *, #22218, .T. ) ;
#62203 = CARTESIAN_POINT ( 'NONE',  ( 19.10802705166043580, 11.29804532628753044, 11.49999999999999645 ) ) ;
#62205 = DIRECTION ( 'NONE',  ( 0.000000000000000000, 1.000000000000000000, 0.000000000000000000 ) ) ;
#62206 = PLANE ( 'NONE',  #44003 ) ;
#62207 = ORIENTED_EDGE ( 'NONE', *, *, #59500, .T. ) ;
#62208 = AXIS2_PLACEMENT_3D ( 'NONE', #40567, #71519, #19700 ) ;
#62209 = CARTESIAN_POINT ( 'NONE',  ( 8.854694546379761277, 20.84150027139232364, -1.500000000000002220 ) ) ;
#62210 = ADVANCED_FACE ( 'NONE', ( #89539 ), #55235, .T. ) ;
#62212 = EDGE_LOOP ( 'NONE', ( #7028, #2055, #3510, #39180 ) ) ;
#62211 = CARTESIAN_POINT ( 'NONE',  ( -115.5200931463694332, -23.85049219812686871, 10.88485053497526778 ) ) ;
#62213 = VECTOR ( 'NONE', #97226, 1000.000000000000114 ) ;
#62214 = VERTEX_POINT ( 'NONE', #930 ) ;
#62215 = CARTESIAN_POINT ( 'NONE',  ( 30.53060340732036337, 5.297812262124996785, 1.539714685317421505 ) ) ;
#62216 = EDGE_CURVE ( 'NONE', #46658, #76257, #85942, .T. ) ;
#62217 = CARTESIAN_POINT ( 'NONE',  ( 17.11712468798820908, 10.61635618877791742, 11.49999999999998934 ) ) ;
#62218 = CARTESIAN_POINT ( 'NONE',  ( -81.62287095715004170, -23.96177878511307568, 10.65340807706330217 ) ) ;
#62219 = ORIENTED_EDGE ( 'NONE', *, *, #8636, .F. ) ;
#62220 = FACE_OUTER_BOUND ( 'NONE', #27346, .T. ) ;
#62221 = CARTESIAN_POINT ( 'NONE',  ( -13.97600220251353953, -17.46790257487896270, -1.500000000000002220 ) ) ;
#62222 = EDGE_CURVE ( 'NONE', #15342, #1176, #95656, .T. ) ;
#62223 = VERTEX_POINT ( 'NONE', #48622 ) ;
#62224 = ORIENTED_EDGE ( 'NONE', *, *, #35685, .F. ) ;
#62225 = CARTESIAN_POINT ( 'NONE',  ( -28.52287095715005805, -24.49960542107631056, 8.947790409070465856 ) ) ;
#62226 = CARTESIAN_POINT ( 'NONE',  ( -94.58632622716793037, -24.51419770103156281, 9.386484678747184063 ) ) ;
#62227 = CARTESIAN_POINT ( 'NONE',  ( -46.62287095715004881, -24.64965695001467694, 8.947790433994185832 ) ) ;
#62228 = CARTESIAN_POINT ( 'NONE',  ( -57.55620429048337883, -24.64965694238574301, 8.947790433994201820 ) ) ;
#62229 = B_SPLINE_CURVE_WITH_KNOTS ( 'NONE', 3,
 ( #3113, #64024, #25927, #28298 ),
 .UNSPECIFIED., .F., .F.,
 ( 4, 4 ),
 ( 0.000000000000000000, 9.999999999999593903E-05 ),
 .UNSPECIFIED. ) ;
#62230 = CARTESIAN_POINT ( 'NONE',  ( -100.5228709571500616, -29.50249982740957577, 7.747779886224967605 ) ) ;
#62231 = CARTESIAN_POINT ( 'NONE',  ( -8.292788067677484776, 17.68049324621676632, 11.49999999999998934 ) ) ;
#62232 = CARTESIAN_POINT ( 'NONE',  ( -38.92287095715006728, -23.47596703998600276, 11.44779298504227683 ) ) ;
#62233 = CARTESIAN_POINT ( 'NONE',  ( 20.96596170256846747, -4.772324250704091497, -1.500000000000002220 ) ) ;
#62234 = CARTESIAN_POINT ( 'NONE',  ( -128.6237110843704841, -24.34968618360935011, 0.1864209137779018477 ) ) ;
#62235 = CARTESIAN_POINT ( 'NONE',  ( 0.8126045299064830196, -1.450440077808301975, 8.999999999999987566 ) ) ;
#62236 = DIRECTION ( 'NONE',  ( 0.000000000000000000, -1.000000000000000000, 0.000000000000000000 ) ) ;
#62237 = LINE ( 'NONE', #70843, #217 ) ;
#62238 = CARTESIAN_POINT ( 'NONE',  ( -1.055347110731411187, -22.84297022578905612, -1.500000000000002220 ) ) ;
#62239 = PERSON_AND_ORGANIZATION ( #70597, #27821 ) ;
#62240 = CARTESIAN_POINT ( 'NONE',  ( -96.51886295441239838, -23.73791477778912196, 11.05961554403170410 ) ) ;
#62241 = CARTESIAN_POINT ( 'NONE',  ( -2.794644232660540961, -5.876774720514416295, 20.26757654895259009 ) ) ;
#62242 = CARTESIAN_POINT ( 'NONE',  ( -12.65591448191638335, 15.52279176289047236, 11.49999999999999645 ) ) ;
#62243 = CARTESIAN_POINT ( 'NONE',  ( -116.6228709571500559, -29.50248528299804818, 1.056150453629045360 ) ) ;
#62244 = DIRECTION ( 'NONE',  ( 0.000000000000000000, -1.000000000000000000, 0.000000000000000000 ) ) ;
#62245 = CARTESIAN_POINT ( 'NONE',  ( 4.190829928318763109, -5.876774720514402084, 18.23548058298382557 ) ) ;
#62246 = DIRECTION ( 'NONE',  ( -3.773278334453079618E-23, 0.9999999999976377785, 2.173523156925979975E-06 ) ) ;
#62247 = ORIENTED_EDGE ( 'NONE', *, *, #76885, .T. ) ;
#62248 = CARTESIAN_POINT ( 'NONE',  ( -109.5228709571500616, -23.47596703998600631, 11.44779298504228038 ) ) ;
#62249 = CARTESIAN_POINT ( 'NONE',  ( -108.9572686384559717, -25.27089656451258293, 4.080339631227976049 ) ) ;
#62250 = CARTESIAN_POINT ( 'NONE',  ( 17.47290450027814757, -12.96279059203284767, -1.500000000000002220 ) ) ;
#62251 = CARTESIAN_POINT ( 'NONE',  ( -56.62287095715007723, -23.96177878511307568, 10.65340807706329862 ) ) ;
#62252 = CARTESIAN_POINT ( 'NONE',  ( 16.02095076306289201, 11.36058263404076030, -1.500000000000002220 ) ) ;
#62253 = CARTESIAN_POINT ( 'NONE',  ( -128.6228709571500417, -24.64898659630529565, 1.056161002820834804 ) ) ;
#62254 = CARTESIAN_POINT ( 'NONE',  ( -109.3584176993576591, -25.31697944907574538, 4.206202445080533536 ) ) ;
#62255 = SECURITY_CLASSIFICATION_LEVEL ( 'unclassified' ) ;
#62256 = CARTESIAN_POINT ( 'NONE',  ( -56.62287095715005592, -23.72773821059536559, 11.05748984161097503 ) ) ;
#62257 = CARTESIAN_POINT ( 'NONE',  ( 13.91401389203221406, -3.316774720514426456, 158.0376437107427137 ) ) ;
#62258 = CARTESIAN_POINT ( 'NONE',  ( 9.245221688665949955, -18.36014492602614467, 11.49999999999999645 ) ) ;
#62259 = DIRECTION ( 'NONE',  ( -3.773278334453079030E-23, 0.9999999999976377785, 2.173523156925979128E-06 ) ) ;
#62260 = AXIS2_PLACEMENT_3D ( 'NONE', #24423, #88337, #74110 ) ;
#62261 = CARTESIAN_POINT ( 'NONE',  ( -47.62287095715008434, -23.96127896941632685, -0.6493128931037891460 ) ) ;
#62262 = EDGE_LOOP ( 'NONE', ( #75354, #53414, #27830, #38328 ) ) ;
#62263 = EDGE_CURVE ( 'NONE', #33073, #16993, #54495, .T. ) ;
#62264 = CARTESIAN_POINT ( 'NONE',  ( -80.80810426221744081, -25.29535151472738264, 4.196860092590704028 ) ) ;
#62265 = CARTESIAN_POINT ( 'NONE',  ( -40.06853693287165186, -25.18430885312715617, 3.358278162901255026 ) ) ;
#62267 = EDGE_CURVE ( 'NONE', #57214, #15127, #37250, .T. ) ;
#62266 = CARTESIAN_POINT ( 'NONE',  ( -97.56097956155602446, -23.48783264082477729, -1.443836473390088138 ) ) ;
#62268 = FACE_OUTER_BOUND ( 'NONE', #86009, .T. ) ;
#62269 = CARTESIAN_POINT ( 'NONE',  ( -26.05468383228075169, -24.93063430545317516, 7.311465254594289753 ) ) ;
#62270 = EDGE_CURVE ( 'NONE', #95575, #81379, #29155, .T. ) ;
#62271 = DIRECTION ( 'NONE',  ( 0.7512896232465892110, -0.000000000000000000, 0.6599726524652351767 ) ) ;
#62272 = EDGE_CURVE ( 'NONE', #647, #77342, #9291, .T. ) ;
#62273 = ORIENTED_EDGE ( 'NONE', *, *, #73195, .F. ) ;
#62274 = CARTESIAN_POINT ( 'NONE',  ( 21.06059016766346659, 9.494407541345388779, 11.49999999999999645 ) ) ;
#62275 = CARTESIAN_POINT ( 'NONE',  ( 21.74077840044056842, -6.890983112422549794, 11.49999999999998934 ) ) ;
#62276 = CARTESIAN_POINT ( 'NONE',  ( -74.63035518566482551, -24.34968618360933945, 0.1864209137778816139 ) ) ;
#62277 = AXIS2_PLACEMENT_3D ( 'NONE', #79241, #71647, #16343 ) ;
#62278 = CARTESIAN_POINT ( 'NONE',  ( -96.56113055612571827, -23.48783264082477018, -1.443836473390089914 ) ) ;
#62279 = CARTESIAN_POINT ( 'NONE',  ( -61.24303308397303880, -25.03284409833926105, 7.563174216509380265 ) ) ;
#62280 = CARTESIAN_POINT ( 'NONE',  ( -8.519796113377745783, 20.75715399588506926, 11.49999999999999645 ) ) ;
#62281 = VERTEX_POINT ( 'NONE', #74797 ) ;
#62282 = CARTESIAN_POINT ( 'NONE',  ( -69.58953762381672448, -24.65952944569304606, 1.056160979905704567 ) ) ;
#62283 = CYLINDRICAL_SURFACE ( 'NONE', #27043, 1.306876713926001354 ) ;
#62284 = CARTESIAN_POINT ( 'NONE',  ( 0.1985894851802381678, 21.93841921393417849, -1.500000000000002220 ) ) ;
#62285 = B_SPLINE_CURVE_WITH_KNOTS ( 'NONE', 3,
 ( #95759, #1423, #79024, #24243, #49105, #78013, #78516, #33863, #17636, #71433, #79533, #32358, #9023, #31866, #1922, #48608, #9522, #40980, #86645, #71940, #25243, #87147 ),
 .UNSPECIFIED., .F., .F.,
 ( 4, 2, 2, 2, 2, 2, 2, 2, 2, 2, 4 ),
 ( 0.000000000000000000, 0.0002789520332696046362, 0.0005579040665392092724, 0.0008368560998088139628, 0.001115808133078418545, 0.001673712199617617300, 0.002231616266156815839, 0.002789520332696014595, 0.003347424399235213784, 0.003905328465774412540, 0.004463232532313610862 ),
 .UNSPECIFIED. ) ;
#62286 = CARTESIAN_POINT ( 'NONE',  ( -5.293508136514246232, -6.376774720514410077, 19.18727597066021318 ) ) ;
#62287 = CARTESIAN_POINT ( 'NONE',  ( -44.58159999861633338, -24.51419770103159834, 9.386484678747169852 ) ) ;
#62288 = DIRECTION ( 'NONE',  ( 0.000000000000000000, 0.000000000000000000, 1.000000000000000000 ) ) ;
#62289 = ORIENTED_EDGE ( 'NONE', *, *, #99229, .F. ) ;
#62290 = DIRECTION ( 'NONE',  ( -0.1254312216594016538, 0.000000000000000000, -0.9921023176230513441 ) ) ;
#62291 = DIRECTION ( 'NONE',  ( 0.000000000000000000, 0.000000000000000000, 1.000000000000000000 ) ) ;
#62292 = EDGE_LOOP ( 'NONE', ( #100350, #17232, #16465, #72280 ) ) ;
#62293 = CARTESIAN_POINT ( 'NONE',  ( 1.259202695315177589, 20.44674571593545664, 11.49999999999998934 ) ) ;
#62294 = EDGE_LOOP ( 'NONE', ( #58795, #33500, #99123, #54813 ) ) ;
#62295 = ORIENTED_EDGE ( 'NONE', *, *, #43217, .T. ) ;
#62296 = ORIENTED_EDGE ( 'NONE', *, *, #16133, .T. ) ;
#62297 = VERTEX_POINT ( 'NONE', #91027 ) ;
#62298 = CARTESIAN_POINT ( 'NONE',  ( -13.34915495237762251, 18.83725853537101358, 11.49999999999998934 ) ) ;
#62299 = CARTESIAN_POINT ( 'NONE',  ( -49.17688710052657797, -25.23571112353340595, 3.608735733131122281 ) ) ;
#62300 = CARTESIAN_POINT ( 'NONE',  ( 18.81862293822770837, 7.596102252255398035, -1.500000000000002220 ) ) ;
#62301 = EDGE_LOOP ( 'NONE', ( #7807, #89620, #46364, #50576 ) ) ;
#62302 = FACE_OUTER_BOUND ( 'NONE', #30728, .T. ) ;
#62303 = CARTESIAN_POINT ( 'NONE',  ( -92.58398966098822314, -24.65952944569303895, 1.056160979905702346 ) ) ;
#62304 = DIRECTION ( 'NONE',  ( 0.000000000000000000, -2.173523156925980399E-06, 0.9999999999976378895 ) ) ;
#62305 = DIRECTION ( 'NONE',  ( 0.000000000000000000, 1.000000000000000000, 0.000000000000000000 ) ) ;
#62307 = VERTEX_POINT ( 'NONE', #81924 ) ;
#62306 = CARTESIAN_POINT ( 'NONE',  ( -5.860608850286626925, 20.67097946995454905, 11.49999999999999645 ) ) ;
#62308 = CARTESIAN_POINT ( 'NONE',  ( -75.49536848232909847, -24.73486907724918282, 1.287355809206967683 ) ) ;
#62309 = CARTESIAN_POINT ( 'NONE',  ( -61.58759230001847129, -24.35071581493543036, 9.817618358456030592 ) ) ;
#62310 = CIRCLE ( 'NONE', #12085, 251.4258649670780699 ) ;
#62311 = ORIENTED_EDGE ( 'NONE', *, *, #88871, .F. ) ;
#62312 = CARTESIAN_POINT ( 'NONE',  ( 20.56943099487245519, -2.726235779781958968, -1.500000000000002220 ) ) ;
#62313 = ORIENTED_EDGE ( 'NONE', *, *, #63667, .F. ) ;
#62315 = ORIENTED_EDGE ( 'NONE', *, *, #18839, .T. ) ;
#62314 = CARTESIAN_POINT ( 'NONE',  ( -27.96875734969026084, 6.143225279485574397, 23.50402280011861933 ) ) ;
#62316 = CARTESIAN_POINT ( 'NONE',  ( -111.5905771631722843, -24.15620529776629510, 10.23563542870659582 ) ) ;
#62318 = PLANE ( 'NONE',  #55069 ) ;
#62317 = B_SPLINE_CURVE_WITH_KNOTS ( 'NONE', 3,
 ( #44358, #35743, #19504, #73307 ),
 .UNSPECIFIED., .F., .F.,
 ( 4, 4 ),
 ( 0.000000000000000000, 1.000000000000000000 ),
 .UNSPECIFIED. ) ;
#62319 = VERTEX_POINT ( 'NONE', #36748 ) ;
#62320 = EDGE_LOOP ( 'NONE', ( #74846, #5473, #7799, #3396 ) ) ;
#62321 = CARTESIAN_POINT ( 'NONE',  ( -55.52287095715005449, -24.99156044556119483, 7.747789690856173195 ) ) ;
#62322 = CARTESIAN_POINT ( 'NONE',  ( -77.62287095715007013, -23.95044443724992433, 10.65354141964650125 ) ) ;
#62323 = CARTESIAN_POINT ( 'NONE',  ( 32.76111974776238611, 3.316774720514426900, -3.850861272813261849 ) ) ;
#62324 = CARTESIAN_POINT ( 'NONE',  ( -21.92701646642465008, -2.088449908657787457, 11.49999999999999645 ) ) ;
#62325 = DIRECTION ( 'NONE',  ( -3.773278334453079030E-23, 0.9999999999976377785, 2.173523156925979128E-06 ) ) ;
#62326 = CARTESIAN_POINT ( 'NONE',  ( -1.585881643086899606, 22.48459252949185228, -1.500000000000002220 ) ) ;
#62327 = CARTESIAN_POINT ( 'NONE',  ( -2.639205680565387624, -20.84613592336672028, -1.500000000000002220 ) ) ;
#62328 = LINE ( 'NONE', #69429, #57293 ) ;
#62329 = VERTEX_POINT ( 'NONE', #12401 ) ;
#62330 = EDGE_LOOP ( 'NONE', ( #81515, #83239, #52590, #52831 ) ) ;
#62331 = CARTESIAN_POINT ( 'NONE',  ( 14.76093561896379214, 5.965225279485572685, -26.55548769130089681 ) ) ;
#62332 = EDGE_CURVE ( 'NONE', #75868, #19742, #21766, .T. ) ;
#62333 = AXIS2_PLACEMENT_3D ( 'NONE', #98940, #4616, #82718 ) ;
#62334 = EDGE_CURVE ( 'NONE', #8243, #31435, #6040, .T. ) ;
#62335 = CARTESIAN_POINT ( 'NONE',  ( -113.6228709571501270, -23.95044443724993499, 10.65354141964649415 ) ) ;
#62336 = EDGE_LOOP ( 'NONE', ( #9758, #97956 ) ) ;
#62337 = CARTESIAN_POINT ( 'NONE',  ( 1.812468502196824760, -21.08352789287561180, 11.49999999999998934 ) ) ;
#62338 = PLANE ( 'NONE',  #33568 ) ;
#62339 = CARTESIAN_POINT ( 'NONE',  ( -51.06671402896819956, -25.03148719215326778, 7.458180231579937036 ) ) ;
#62340 = CARTESIAN_POINT ( 'NONE',  ( -121.6245723567604813, -24.34968618360934300, 0.1864209137778885528 ) ) ;
#62341 = CARTESIAN_POINT ( 'NONE',  ( -52.52287095715005449, -23.47593901973090524, -1.443836447538997092 ) ) ;
#62342 = CARTESIAN_POINT ( 'NONE',  ( -127.5228709571500900, -24.51387760970726504, 9.387446482453405849 ) ) ;
#62343 = CARTESIAN_POINT ( 'NONE',  ( -21.14055147415990277, -6.693858341896442354, -1.500000000000002220 ) ) ;
#62344 = CARTESIAN_POINT ( 'NONE',  ( -8.063330319165405768, -10.15233964170348457, 1.310587897985993733 ) ) ;
#62345 = AXIS2_PLACEMENT_3D ( 'NONE', #79122, #40072, #56317 ) ;
#62346 = ORIENTED_EDGE ( 'NONE', *, *, #39662, .F. ) ;
#62347 = CARTESIAN_POINT ( 'NONE',  ( 5.271800844830267785, -5.965225279485592225, -28.56638892017480913 ) ) ;
#62348 = DIRECTION ( 'NONE',  ( -3.773278334453079030E-23, 0.9999999999976377785, 2.173523156925979128E-06 ) ) ;
#62349 = CARTESIAN_POINT ( 'NONE',  ( -126.5206434123637393, -24.51314013834316086, 0.6176544820404181735 ) ) ;
#62350 = DIRECTION ( 'NONE',  ( 0.000000000000000000, 0.000000000000000000, 1.000000000000000000 ) ) ;
#62351 = DIRECTION ( 'NONE',  ( -3.773278334444167608E-23, 1.000000000000000000, 0.000000000000000000 ) ) ;
#62352 = CARTESIAN_POINT ( 'NONE',  ( 14.64286990871793392, 12.78475832571431070, 11.49999999999998934 ) ) ;
#62353 = CARTESIAN_POINT ( 'NONE',  ( 16.75108703964928480, -13.32659110743468212, 11.49999999999998934 ) ) ;
#62354 = CARTESIAN_POINT ( 'NONE',  ( -53.01255352321339842, 1.477225279485574028, 35.59556822165056644 ) ) ;
#62355 = CYLINDRICAL_SURFACE ( 'NONE', #39867, 24.00000000000000000 ) ;
#62356 = DIRECTION ( 'NONE',  ( -3.773278334444166432E-23, 1.000000000000000000, 0.000000000000000000 ) ) ;
#62357 = CARTESIAN_POINT ( 'NONE',  ( -101.2905359165590227, -25.27360087335221550, 3.812648439097560793 ) ) ;
#62358 = CARTESIAN_POINT ( 'NONE',  ( -21.72567761722203628, 6.514095075961352954, -1.500000000000002220 ) ) ;
#62359 = CARTESIAN_POINT ( 'NONE',  ( -103.6228709571500701, -23.96127896941633750, -0.6493128931037811524 ) ) ;
#62360 = CARTESIAN_POINT ( 'NONE',  ( -80.52287095715006160, -23.47593901973090169, -1.443836447538996648 ) ) ;
#62361 = CARTESIAN_POINT ( 'NONE',  ( 17.59243620335545799, -9.192777620008959261, 11.49999999999999645 ) ) ;
#62362 = CARTESIAN_POINT ( 'NONE',  ( -123.5900400688965561, -24.15620529776629866, 10.23563542870659582 ) ) ;
#62363 = CARTESIAN_POINT ( 'NONE',  ( -88.52287095715006160, -24.64898659630367916, 1.056161002820827921 ) ) ;
#62364 = VERTEX_POINT ( 'NONE', #76289 ) ;
#62365 = FACE_OUTER_BOUND ( 'NONE', #41349, .T. ) ;
#62366 = LINE ( 'NONE', #63385, #10215 ) ;
#62367 = PLANE ( 'NONE',  #88507 ) ;
#62368 = CARTESIAN_POINT ( 'NONE',  ( 11.52859134480388903, -18.33581920571378632, -1.500000000000002220 ) ) ;
#62369 = CARTESIAN_POINT ( 'NONE',  ( 6.420673076923079314, -6.376774720514427841, 21.83974358974358765 ) ) ;
#62370 = CARTESIAN_POINT ( 'NONE',  ( -5.694372300836820777, 18.57635362771370424, -1.500000000000002220 ) ) ;
#62371 = CARTESIAN_POINT ( 'NONE',  ( -55.58579905264048904, -24.63419186844611275, 9.035850630976927533 ) ) ;
#62372 = EDGE_CURVE ( 'NONE', #24081, #99074, #91523, .T. ) ;
#62373 = EDGE_LOOP ( 'NONE', ( #97526, #78509, #4045, #23616 ) ) ;
#62374 = AXIS2_PLACEMENT_3D ( 'NONE', #51634, #88702, #97796 ) ;
#62375 = CARTESIAN_POINT ( 'NONE',  ( 14.85214116200856083, 13.97194181870810326, 11.49999999999999645 ) ) ;
#62376 = CARTESIAN_POINT ( 'NONE',  ( -80.50908809528748122, -24.15503026093913164, -0.2815557561904567518 ) ) ;
#62377 = B_SPLINE_CURVE_WITH_KNOTS ( 'NONE', 3,
 ( #28123, #43850, #4785, #57589, #67197, #98112 ),
 .UNSPECIFIED., .F., .F.,
 ( 4, 2, 4 ),
 ( 0.000000000000000000, 0.001380901958385390062, 0.002761803916770780125 ),
 .UNSPECIFIED. ) ;
#62378 = CARTESIAN_POINT ( 'NONE',  ( 12.16765770914787304, 6.475225279485573360, -27.57618308014988173 ) ) ;
#62379 = VERTEX_POINT ( 'NONE', #52477 ) ;
#62380 = CARTESIAN_POINT ( 'NONE',  ( -41.32712894388434677, -25.24779038991585267, 3.715000390373129679 ) ) ;
#62381 = CARTESIAN_POINT ( 'NONE',  ( -92.52287095715010423, -24.33832256527049509, 0.1851278514138617326 ) ) ;
#62382 = CARTESIAN_POINT ( 'NONE',  ( -49.27237840819080361, -25.31601884727480822, 5.251752407945899925 ) ) ;
#62383 = ADVANCED_FACE ( 'NONE', ( #28143 ), #44371, .T. ) ;
#62384 = DIRECTION ( 'NONE',  ( -3.773278334453079030E-23, 0.9999999999976377785, 2.173523156925979128E-06 ) ) ;
#62385 = CARTESIAN_POINT ( 'NONE',  ( -0.9827876235267493099, -6.376774720514415407, 19.81240905262004404 ) ) ;
#62386 = CARTESIAN_POINT ( 'NONE',  ( 12.55954966114946458, -15.69740789531843461, -1.500000000000002220 ) ) ;
#62387 = DIRECTION ( 'NONE',  ( 0.9975640502598243087, -0.06975647374412546897, -0.000000000000000000 ) ) ;
#62389 = ORIENTED_EDGE ( 'NONE', *, *, #27192, .T. ) ;
#62388 = ADVANCED_FACE ( 'NONE', ( #97640 ), #21997, .T. ) ;
#62390 = CARTESIAN_POINT ( 'NONE',  ( -81.62287095715005592, -23.47593901973091235, -1.443836447539004642 ) ) ;
#62391 = ADVANCED_FACE ( 'NONE', ( #75793 ), #22495, .F. ) ;
#62392 = CARTESIAN_POINT ( 'NONE',  ( -9.520747347383798243, -20.79447232172871907, 11.49999999999999645 ) ) ;
#62393 = CARTESIAN_POINT ( 'NONE',  ( -22.07869367785253090, -5.390224856484156390, 11.49999999999998934 ) ) ;
#62394 = EDGE_LOOP ( 'NONE', ( #92298, #18713, #70978, #61697 ) ) ;
#62395 = CARTESIAN_POINT ( 'NONE',  ( -30.47287095715007155, -24.75375236407085566, 8.603495955171387877 ) ) ;
#62396 = EDGE_CURVE ( 'NONE', #63282, #42731, #12896, .T. ) ;
#62397 = CARTESIAN_POINT ( 'NONE',  ( 32.16024265030974050, 0.3587747205144265483, 16.27760796525321751 ) ) ;
#62398 = CARTESIAN_POINT ( 'NONE',  ( -38.51305747304791538, -23.73791477778911485, 11.05961554403170766 ) ) ;
#62399 = ADVANCED_FACE ( 'NONE', ( #67217 ), #45372, .F. ) ;
#62400 = CARTESIAN_POINT ( 'NONE',  ( -30.57287095715007297, -25.31506640534328056, 5.571610402288234454 ) ) ;
#62401 = VECTOR ( 'NONE', #83333, 1000.000000000000000 ) ;
#62402 = B_SPLINE_CURVE_WITH_KNOTS ( 'NONE', 3,
 ( #59435, #5140, #27982, #74156 ),
 .UNSPECIFIED., .F., .F.,
 ( 4, 4 ),
 ( 0.000000000000000000, 9.999999999998897304E-05 ),
 .UNSPECIFIED. ) ;
#62403 = CARTESIAN_POINT ( 'NONE',  ( -4.141025641025642301, -6.376774720514408301, 19.19230769230769695 ) ) ;
#62404 = CARTESIAN_POINT ( 'NONE',  ( -124.5228709571500900, -23.48783264082477373, -1.443836473390085029 ) ) ;
#62405 = ORIENTED_EDGE ( 'NONE', *, *, #71872, .F. ) ;
#62406 = CARTESIAN_POINT ( 'NONE',  ( 15.56926775127050000, -13.18612581554039132, -1.500000000000002220 ) ) ;
#62407 = VERTEX_POINT ( 'NONE', #37740 ) ;
#62408 = EDGE_CURVE ( 'NONE', #44155, #9237, #98630, .T. ) ;
#62409 = B_SPLINE_CURVE_WITH_KNOTS ( 'NONE', 3,
 ( #42075, #50673, #34450, #10606, #12598, #35940, #97830, #81619, #28325, #80116, #59279, #90228 ),
 .UNSPECIFIED., .F., .F.,
 ( 4, 2, 2, 2, 2, 4 ),
 ( 4.336808689942017736E-18, 0.0001760285354383833852, 0.0003520570708767624337, 0.0007041141417535211810, 0.001056171212630279983, 0.001408228283507038676 ),
 .UNSPECIFIED. ) ;
#62410 = CARTESIAN_POINT ( 'NONE',  ( -21.12268324108725892, 9.058254180033936009, -1.500000000000002220 ) ) ;
#62411 = CARTESIAN_POINT ( 'NONE',  ( -54.56747899101539190, -23.48786465467240703, 11.44779295918255180 ) ) ;
#62412 = CIRCLE ( 'NONE', #76943, 0.8160000000000007248 ) ;
#62413 = EDGE_LOOP ( 'NONE', ( #19235, #3017, #36728, #3027 ) ) ;
#62414 = CARTESIAN_POINT ( 'NONE',  ( -10.59832330691884117, 0.3587747205144061757, -27.05373799718300987 ) ) ;
#62415 = VECTOR ( 'NONE', #59546, 1000.000000000000000 ) ;
#62416 = B_SPLINE_CURVE_WITH_KNOTS ( 'NONE', 3,
 ( #25442, #49302, #18334, #72136, #2622, #33561, #95453, #10727, #41689, #3127, #65042, #78546, #40002, #25271 ),
 .UNSPECIFIED., .F., .F.,
 ( 4, 2, 2, 2, 2, 2, 4 ),
 ( 0.000000000000000000, 0.0002387142825911133296, 0.0004774285651822266592, 0.0009548571303644522341, 0.001432285695546677701, 0.001670999978137770701, 0.001909714260728863702 ),
 .UNSPECIFIED. ) ;
#62417 = FACE_OUTER_BOUND ( 'NONE', #3916, .T. ) ;
#62418 = DIRECTION ( 'NONE',  ( -0.000000000000000000, 1.000000000000000000, -0.000000000000000000 ) ) ;
#62420 = ORIENTED_EDGE ( 'NONE', *, *, #21614, .F. ) ;
#62419 = CARTESIAN_POINT ( 'NONE',  ( 17.02398533174402218, 12.79255474601471043, 11.49999999999999645 ) ) ;
#62421 = ORIENTED_EDGE ( 'NONE', *, *, #76050, .T. ) ;
#62422 = CARTESIAN_POINT ( 'NONE',  ( 16.02632597834478645, 15.35701383120132313, 11.49999999999998934 ) ) ;
#62423 = CARTESIAN_POINT ( 'NONE',  ( 1.453578435135240321, -20.60874541997745268, 11.49999999999998934 ) ) ;
#62424 = ORIENTED_EDGE ( 'NONE', *, *, #95705, .T. ) ;
#62425 = ORIENTED_EDGE ( 'NONE', *, *, #82022, .F. ) ;
#62426 = CARTESIAN_POINT ( 'NONE',  ( -4.977357939505175466, -5.876774720514410077, 19.14913681718893557 ) ) ;
#62427 = CARTESIAN_POINT ( 'NONE',  ( -71.72343159422317171, -25.32724624944561853, 4.398071659717722959 ) ) ;
#62428 = ORIENTED_EDGE ( 'NONE', *, *, #79796, .F. ) ;
#62429 = CARTESIAN_POINT ( 'NONE',  ( -91.58383859757618950, -24.65952944569304606, 1.056160979905701680 ) ) ;
#62430 = EDGE_LOOP ( 'NONE', ( #90234, #39683, #83031, #13264 ) ) ;
#62431 = CARTESIAN_POINT ( 'NONE',  ( -58.53810489024537844, -24.51419770103156637, 9.386484678747176957 ) ) ;
#62432 = FACE_OUTER_BOUND ( 'NONE', #63211, .T. ) ;
#62433 = CARTESIAN_POINT ( 'NONE',  ( -3.686900873480770002, -20.48319827837541141, -1.500000000000002220 ) ) ;
#62434 = CARTESIAN_POINT ( 'NONE',  ( 3.267597511969735802, 21.59432767039258394, 11.49999999999999645 ) ) ;
#62435 = CARTESIAN_POINT ( 'NONE',  ( -91.94687923781920347, -25.22391124735684187, 6.409327647371628522 ) ) ;
#62436 = CARTESIAN_POINT ( 'NONE',  ( -78.58481383403142218, -24.51419770103157347, 9.386484678747175181 ) ) ;
#62437 = CARTESIAN_POINT ( 'NONE',  ( 12.99221220249228281, -18.32192329980629708, -1.500000000000002220 ) ) ;
#62438 = CARTESIAN_POINT ( 'NONE',  ( -38.52201953751992392, -23.48783264082477729, -1.443836473390076591 ) ) ;
#62439 = EDGE_CURVE ( 'NONE', #93762, #73142, #99619, .T. ) ;
#62440 = PLANE ( 'NONE',  #63110 ) ;
#62441 = CARTESIAN_POINT ( 'NONE',  ( 4.966987340572156739, -5.876774720514418071, 20.16530235339958210 ) ) ;
#62442 = VECTOR ( 'NONE', #56519, 1000.000000000000000 ) ;
#62443 = ORIENTED_EDGE ( 'NONE', *, *, #19983, .T. ) ;
#62444 = ORIENTED_EDGE ( 'NONE', *, *, #61490, .T. ) ;
#62445 = ADVANCED_FACE ( 'NONE', ( #92022 ), #90527, .F. ) ;
#62446 = ORIENTED_EDGE ( 'NONE', *, *, #35715, .T. ) ;
#62447 = CARTESIAN_POINT ( 'NONE',  ( -18.12654925440673637, -11.31956730046968751, -1.500000000000002220 ) ) ;
#62448 = VERTEX_POINT ( 'NONE', #60104 ) ;
#62449 = CARTESIAN_POINT ( 'NONE',  ( 21.00884048613226440, 1.293913838035418040, -1.500000000000002220 ) ) ;
#62450 = CARTESIAN_POINT ( 'NONE',  ( -30.43338820629497476, -24.47561425214244224, 0.5642940035406436294 ) ) ;
#62451 = B_SPLINE_CURVE_WITH_KNOTS ( 'NONE', 3,
 ( #82056, #13027, #5426, #36877 ),
 .UNSPECIFIED., .F., .F.,
 ( 4, 4 ),
 ( 0.5609005253356335041, 0.5699069566077490379 ),
 .UNSPECIFIED. ) ;
#62452 = CARTESIAN_POINT ( 'NONE',  ( 11.38277053702107899, 16.36964821499295653, -1.500000000000002220 ) ) ;
#62453 = CARTESIAN_POINT ( 'NONE',  ( -50.63202991560478949, -24.73531770709094602, 8.716586749053508498 ) ) ;
#62454 = CARTESIAN_POINT ( 'NONE',  ( 2.904244945035652670, -6.376774720514415407, 20.04207437776001299 ) ) ;
#62455 = CARTESIAN_POINT ( 'NONE',  ( 12.33731239738771102, -18.22686410513083288, -1.500000000000002220 ) ) ;
#62456 = CARTESIAN_POINT ( 'NONE',  ( -87.52287095715003318, -24.33832256527048088, 0.1851278514138628983 ) ) ;
#62457 = EDGE_LOOP ( 'NONE', ( #1274, #70587, #97104, #24078 ) ) ;
#62458 = DIRECTION ( 'NONE',  ( -3.773278334453079618E-23, 0.9999999999976377785, 2.173523156925979975E-06 ) ) ;
#62459 = DIRECTION ( 'NONE',  ( 0.000000000000000000, 0.000000000000000000, -1.000000000000000000 ) ) ;
#62460 = CARTESIAN_POINT ( 'NONE',  ( -12.81329989551134751, 16.42372500408851366, 11.49999999999999645 ) ) ;
#62461 = CARTESIAN_POINT ( 'NONE',  ( 31.62551770808318707, -4.240436435409185911, 26.92952082091879973 ) ) ;
#62462 = CARTESIAN_POINT ( 'NONE',  ( -125.5228709571500616, -23.47596703998600631, 11.44779298504227683 ) ) ;
#62463 = CARTESIAN_POINT ( 'NONE',  ( -56.55620429048338593, -23.48783264082477729, -1.443836473390068376 ) ) ;
#62464 = CARTESIAN_POINT ( 'NONE',  ( -17.77299844720193533, 11.79293508692305537, 11.49999999999998934 ) ) ;
#62465 = CARTESIAN_POINT ( 'NONE',  ( -31.24388727629348494, -25.12217695392594763, 7.176903142167552652 ) ) ;
#62466 = CARTESIAN_POINT ( 'NONE',  ( -27.47983700607433732, -24.75185972549630264, 2.285866012509995215 ) ) ;
#62467 = AXIS2_PLACEMENT_3D ( 'NONE', #12706, #43672, #67516 ) ;
#62468 = FACE_OUTER_BOUND ( 'NONE', #70214, .T. ) ;
#62469 = CARTESIAN_POINT ( 'NONE',  ( -5.544977400725785266, -5.876774720514411854, 19.92818918856636401 ) ) ;
#62470 = CC_DESIGN_PERSON_AND_ORGANIZATION_ASSIGNMENT ( #62239, #85556, ( #79677 ) ) ;
#62471 = CARTESIAN_POINT ( 'NONE',  ( -8.307687032909205627, 20.95097986170506488, -1.500000000000002220 ) ) ;
#62472 = VECTOR ( 'NONE', #39806, 1000.000000000000000 ) ;
#62473 = CARTESIAN_POINT ( 'NONE',  ( -110.9400161722045794, -25.25626643526282322, 3.571638612575482874 ) ) ;
#62474 = ORIENTED_EDGE ( 'NONE', *, *, #34992, .T. ) ;
#62475 = CARTESIAN_POINT ( 'NONE',  ( -79.06619145297914031, -25.30163491681836874, 5.325055240909210674 ) ) ;
#62476 = CARTESIAN_POINT ( 'NONE',  ( 2.993365552154886089, -6.376774720514413630, 19.24059921568563425 ) ) ;
#62477 = CARTESIAN_POINT ( 'NONE',  ( 15.15379598424239838, -12.58889634127381640, 11.49999999999999645 ) ) ;
#62478 = CARTESIAN_POINT ( 'NONE',  ( -9.150000000000000355, -5.876774720514426953, -15.69999999999999929 ) ) ;
#62479 = VECTOR ( 'NONE', #95911, 1000.000000000000114 ) ;
#62480 = CARTESIAN_POINT ( 'NONE',  ( -39.55620429048339304, -24.64898659630528499, 1.056161002820822370 ) ) ;
#62481 = EDGE_LOOP ( 'NONE', ( #57202, #48565, #22281, #10872 ) ) ;
#62482 = CIRCLE ( 'NONE', #2515, 8.452410033082758289 ) ;
#62483 = CARTESIAN_POINT ( 'NONE',  ( -99.59111762178828542, -24.15543982623907837, -0.2315651400026449425 ) ) ;
#62484 = CARTESIAN_POINT ( 'NONE',  ( -42.55620429048339304, -24.64965694238574656, 8.947790433994203596 ) ) ;
#62485 = CARTESIAN_POINT ( 'NONE',  ( -91.96772508908847499, -25.06732983082694233, 7.447789526168957508 ) ) ;
#62486 = VECTOR ( 'NONE', #21333, 1000.000000000000000 ) ;
#62487 = LINE ( 'NONE', #39636, #73976 ) ;
#62488 = CARTESIAN_POINT ( 'NONE',  ( 5.037983044326730386, -19.10262670698400100, -1.500000000000002220 ) ) ;
#62489 = VERTEX_POINT ( 'NONE', #22991 ) ;
#62490 = CARTESIAN_POINT ( 'NONE',  ( -120.5228709571500900, -24.83620972994592435, 8.398175272781360334 ) ) ;
#62491 = DATE_TIME_ROLE ( 'classification_date' ) ;
#62492 = ORIENTED_EDGE ( 'NONE', *, *, #12453, .T. ) ;
#62493 = DIRECTION ( 'NONE',  ( 1.000000000000000000, -0.000000000000000000, 0.000000000000000000 ) ) ;
#62494 = CARTESIAN_POINT ( 'NONE',  ( -53.62287095715006302, -23.72747288104441665, -1.053458166803663998 ) ) ;
#62495 = DIRECTION ( 'NONE',  ( 0.000000000000000000, 0.000000000000000000, -1.000000000000000000 ) ) ;
#62496 = CARTESIAN_POINT ( 'NONE',  ( -98.94109201664207376, -25.26638307310151532, 6.485444322923475724 ) ) ;
#62497 = CARTESIAN_POINT ( 'NONE',  ( 6.132272708306365949, -6.376774720514424288, 21.80683391321003839 ) ) ;
#62498 = CARTESIAN_POINT ( 'NONE',  ( -36.62287095715005592, -29.50247984919015209, -1.443849546365060466 ) ) ;
#62499 = LINE ( 'NONE', #8714, #28385 ) ;
#62501 = EDGE_CURVE ( 'NONE', #58389, #922, #73915, .T. ) ;
#62500 = CARTESIAN_POINT ( 'NONE',  ( -15.86121933104946535, 12.22609501325904624, -1.500000000000002220 ) ) ;
#62502 = CARTESIAN_POINT ( 'NONE',  ( -99.12594121859551421, -25.27533104972792799, 3.952132688946379702 ) ) ;
#62503 = CARTESIAN_POINT ( 'NONE',  ( -51.70072539166535108, -25.27314792116673203, 3.987152059579775809 ) ) ;
#62504 = VERTEX_POINT ( 'NONE', #30620 ) ;
#62505 = B_SPLINE_CURVE_WITH_KNOTS ( 'NONE', 3,
 ( #81000, #51057, #65308, #56685 ),
 .UNSPECIFIED., .F., .F.,
 ( 4, 4 ),
 ( 0.000000000000000000, 0.0001000000000000028644 ),
 .UNSPECIFIED. ) ;
#62506 = CARTESIAN_POINT ( 'NONE',  ( 22.02124265030973760, 6.143225279485574397, 13.95402280011862395 ) ) ;
#62507 = VECTOR ( 'NONE', #5091, 1000.000000000000000 ) ;
#62508 = CARTESIAN_POINT ( 'NONE',  ( -110.2348554541972874, -25.29012726010009970, 3.296590529549364490 ) ) ;
#62509 = EDGE_CURVE ( 'NONE', #35033, #96004, #24006, .T. ) ;
#62510 = PLANE ( 'NONE',  #57491 ) ;
#62511 = CARTESIAN_POINT ( 'NONE',  ( 23.60872659128563811, -0.9000000000000000222, -2.097483029078132777 ) ) ;
#62512 = EDGE_CURVE ( 'NONE', #48580, #74478, #145, .T. ) ;
#62513 = CARTESIAN_POINT ( 'NONE',  ( -34.52287095715006160, -29.50250243563736774, 8.947779886222150481 ) ) ;
#62514 = CARTESIAN_POINT ( 'NONE',  ( -83.50635389765871253, -24.34968618360933590, 0.1864209137778810865 ) ) ;
#62515 = CARTESIAN_POINT ( 'NONE',  ( 18.72495633783376334, -0.5000000000000000000, -1.691563534834430227 ) ) ;
#62516 = CARTESIAN_POINT ( 'NONE',  ( 5.464387484610083057, -6.376774720514420736, 21.31215092858952431 ) ) ;
#62517 = ORIENTED_EDGE ( 'NONE', *, *, #63921, .F. ) ;
#62518 = CARTESIAN_POINT ( 'NONE',  ( 18.81862293822770837, 7.596102252255398035, -1.500000000000002220 ) ) ;
#62519 = EDGE_CURVE ( 'NONE', #70921, #61839, #45859, .T. ) ;
#62520 = CARTESIAN_POINT ( 'NONE',  ( -121.5228709571501042, -23.48783264082477018, -1.443836473390083253 ) ) ;
#62521 = CARTESIAN_POINT ( 'NONE',  ( -31.62287095715005236, -29.50250243563736774, 8.947779886222150481 ) ) ;
#62522 = ORIENTED_EDGE ( 'NONE', *, *, #48287, .T. ) ;
#62523 = CARTESIAN_POINT ( 'NONE',  ( -65.05438548721848235, 6.143225279485573509, 29.49402280011861777 ) ) ;
#62524 = CARTESIAN_POINT ( 'NONE',  ( -20.09103079077430820, 1.113595961413322177, -1.500000000000002220 ) ) ;
#62525 = B_SPLINE_CURVE_WITH_KNOTS ( 'NONE', 3,
 ( #2151, #33084, #70642, #39184 ),
 .UNSPECIFIED., .F., .F.,
 ( 4, 4 ),
 ( 0.5501787936871235241, 0.5591852249592388358 ),
 .UNSPECIFIED. ) ;
#62526 = CARTESIAN_POINT ( 'NONE',  ( -20.28541985502614509, -5.886007371444655689, 11.49999999999999645 ) ) ;
#62527 = CARTESIAN_POINT ( 'NONE',  ( -7.320055889550622474, -20.87099576385019972, -1.500000000000002220 ) ) ;
#62528 = CARTESIAN_POINT ( 'NONE',  ( -19.86366060283327784, 5.362777492974458049, 11.49999999999998934 ) ) ;
#62529 = AXIS2_PLACEMENT_3D ( 'NONE', #32817, #63794, #95217 ) ;
#62530 = B_SPLINE_CURVE_WITH_KNOTS ( 'NONE', 3,
 ( #53186, #59804, #90237, #45074 ),
 .UNSPECIFIED., .F., .F.,
 ( 4, 4 ),
 ( 0.000000000000000000, 9.999999999998897304E-05 ),
 .UNSPECIFIED. ) ;
#62531 = CARTESIAN_POINT ( 'NONE',  ( -60.53843391936359097, -24.63355581998385446, 0.9682620441943891043 ) ) ;
#62532 = VERTEX_POINT ( 'NONE', #54470 ) ;
#62533 = CARTESIAN_POINT ( 'NONE',  ( -32.62287095715007013, -24.33832256527047377, 0.1851278514138576803 ) ) ;
#62534 = ORIENTED_EDGE ( 'NONE', *, *, #43503, .F. ) ;
#62535 = CARTESIAN_POINT ( 'NONE',  ( -6.185411026474866958, -6.376774720514411854, 19.34586827028016742 ) ) ;
#62536 = LINE ( 'NONE', #86368, #63188 ) ;
#62537 = ORIENTED_EDGE ( 'NONE', *, *, #82879, .T. ) ;
#62538 = VECTOR ( 'NONE', #47229, 1000.000000000000000 ) ;
#62539 = ORIENTED_EDGE ( 'NONE', *, *, #15491, .F. ) ;
#62540 = VECTOR ( 'NONE', #9425, 1000.000000000000000 ) ;
#62541 = ORIENTED_EDGE ( 'NONE', *, *, #78076, .F. ) ;
#62542 = DIRECTION ( 'NONE',  ( 0.000000000000000000, 0.9999999999976377785, 2.173523156925979975E-06 ) ) ;
#62543 = DIRECTION ( 'NONE',  ( -3.773278334444167608E-23, 1.000000000000000000, 0.000000000000000000 ) ) ;
#62544 = DIRECTION ( 'NONE',  ( 0.000000000000000000, 0.9999999999976377785, 2.173523156925979128E-06 ) ) ;
#62545 = CARTESIAN_POINT ( 'NONE',  ( -12.00526669028610272, -16.82065764665920682, -1.500000000000002220 ) ) ;
#62546 = ADVANCED_FACE ( 'NONE', ( #1184 ), #5310, .T. ) ;
#62547 = AXIS2_PLACEMENT_3D ( 'NONE', #941, #70457, #31892 ) ;
#62548 = CARTESIAN_POINT ( 'NONE',  ( 2.580163054138214562, 21.43444414123800712, 11.49999999999999645 ) ) ;
#62549 = ORIENTED_EDGE ( 'NONE', *, *, #76929, .F. ) ;
#62550 = DIRECTION ( 'NONE',  ( -3.773278334453079030E-23, 0.9999999999976377785, 2.173523156925979128E-06 ) ) ;
#62551 = CARTESIAN_POINT ( 'NONE',  ( 2.790451961050095520, -5.876774720514409189, 18.85195250256714417 ) ) ;
#62552 = CARTESIAN_POINT ( 'NONE',  ( -15.27869365379592281, -16.34152646814254339, -1.500000000000002220 ) ) ;
#62553 = VECTOR ( 'NONE', #62271, 1000.000000000000227 ) ;
#62554 = CARTESIAN_POINT ( 'NONE',  ( -47.59972437050590344, -23.96169478059712432, 10.65365249895718591 ) ) ;
#62555 = CARTESIAN_POINT ( 'NONE',  ( -120.6228709571500417, -23.47596703998600631, 11.44779298504227683 ) ) ;
#62557 = ORIENTED_EDGE ( 'NONE', *, *, #17189, .F. ) ;
#62556 = EDGE_CURVE ( 'NONE', #29304, #39840, #61601, .T. ) ;
#62558 = FACE_OUTER_BOUND ( 'NONE', #27871, .T. ) ;
#62559 = CARTESIAN_POINT ( 'NONE',  ( -35.52841444253756009, -24.73531770709095312, 8.716586749053508498 ) ) ;
#62560 = CARTESIAN_POINT ( 'NONE',  ( -12.67655569012464944, 16.65582705476778358, 11.49999999999998934 ) ) ;
#62561 = ORIENTED_EDGE ( 'NONE', *, *, #61320, .T. ) ;
#62562 = PLANE ( 'NONE',  #58763 ) ;
#62563 = VERTEX_POINT ( 'NONE', #38730 ) ;
#62564 = B_SPLINE_CURVE_WITH_KNOTS ( 'NONE', 3,
 ( #8276, #77763, #85899, #17388 ),
 .UNSPECIFIED., .F., .F.,
 ( 4, 4 ),
 ( 0.000000000000000000, 9.999999999998897304E-05 ),
 .UNSPECIFIED. ) ;
#62565 = EDGE_CURVE ( 'NONE', #91753, #20665, #36, .T. ) ;
#62566 = FACE_OUTER_BOUND ( 'NONE', #92322, .T. ) ;
#62567 = CARTESIAN_POINT ( 'NONE',  ( 6.572693220633653688, -20.11273663914708365, -1.500000000000002220 ) ) ;
#62568 = VERTEX_POINT ( 'NONE', #178 ) ;
#62569 = DIRECTION ( 'NONE',  ( 0.000000000000000000, -0.9999999999976377785, -2.173523156925979975E-06 ) ) ;
#62570 = CARTESIAN_POINT ( 'NONE',  ( -18.25314811174894913, -11.95880190493418738, -1.500000000000002220 ) ) ;
#62571 = CARTESIAN_POINT ( 'NONE',  ( -121.5228709571500758, -24.35013146730204525, 9.818937971375099494 ) ) ;
#62572 = CARTESIAN_POINT ( 'NONE',  ( 7.267403311989051318, -6.376774720514426065, 21.43157132964656952 ) ) ;
#62573 = DIRECTION ( 'NONE',  ( 0.000000000000000000, 0.000000000000000000, 1.000000000000000000 ) ) ;
#62574 = CARTESIAN_POINT ( 'NONE',  ( -0.2038501785326352067, 21.78777694363981254, -1.500000000000002220 ) ) ;
#62575 = CARTESIAN_POINT ( 'NONE',  ( 6.555906488453394410, -6.376774720514426065, 21.46941147007026274 ) ) ;
#62576 = ORIENTED_EDGE ( 'NONE', *, *, #19409, .T. ) ;
#62577 = CARTESIAN_POINT ( 'NONE',  ( 1.095236984349686971, 8.494825072090639750, -1.700000000000008837 ) ) ;
#62578 = CARTESIAN_POINT ( 'NONE',  ( -48.52287095715006160, -29.50247984919015209, -1.443849546365058689 ) ) ;
#62579 = VERTEX_POINT ( 'NONE', #39234 ) ;
#62580 = AXIS2_PLACEMENT_3D ( 'NONE', #78563, #33403, #87196 ) ;
#62581 = VERTEX_POINT ( 'NONE', #70190 ) ;
#62582 = VERTEX_POINT ( 'NONE', #16900 ) ;
#62583 = CARTESIAN_POINT ( 'NONE',  ( -29.18684743162721418, -25.15141295360018603, 3.928745580597657661 ) ) ;
#62584 = DIRECTION ( 'NONE',  ( -1.000000000000000000, 0.000000000000000000, -2.338552693767719605E-15 ) ) ;
#62585 = CARTESIAN_POINT ( 'NONE',  ( 20.46717832272283033, -5.532298862796615424, -1.500000000000002220 ) ) ;
#62586 = CARTESIAN_POINT ( 'NONE',  ( -94.55479543721645541, -23.96119346886881019, -0.6495511937832051386 ) ) ;
#62587 = CARTESIAN_POINT ( 'NONE',  ( -79.53726446675389639, -25.03138232695337706, 7.255560784353935588 ) ) ;
#62588 = DIRECTION ( 'NONE',  ( 1.000000000000000000, -0.000000000000000000, 0.000000000000000000 ) ) ;
#62589 = CARTESIAN_POINT ( 'NONE',  ( -58.52287095715006160, -29.50248528299804818, 1.056150453629034924 ) ) ;
#62590 = EDGE_CURVE ( 'NONE', #26321, #46936, #47863, .T. ) ;
#62591 = CARTESIAN_POINT ( 'NONE',  ( 4.481524277812761525, 18.85844072219565604, -1.500000000000002220 ) ) ;
#62592 = CARTESIAN_POINT ( 'NONE',  ( -51.82569660508215748, -25.29890250005943031, 5.651905355509026840 ) ) ;
#62593 = VERTEX_POINT ( 'NONE', #79293 ) ;
#62594 = CARTESIAN_POINT ( 'NONE',  ( -10.28394983263804185, -16.58134856480417341, 11.49999999999999645 ) ) ;
#62595 = CARTESIAN_POINT ( 'NONE',  ( -20.27875734969026311, -5.356774720514425603, 24.00402280011862288 ) ) ;
#62596 = ADVANCED_FACE ( 'NONE', ( #3200 ), #48868, .F. ) ;
#62597 = CARTESIAN_POINT ( 'NONE',  ( -79.90946178028013946, -25.14686779016199836, 6.961378012461956644 ) ) ;
#62598 = ORIENTED_EDGE ( 'NONE', *, *, #82331, .T. ) ;
#62599 = LINE ( 'NONE', #93525, #26373 ) ;
#62600 = EDGE_CURVE ( 'NONE', #41185, #39688, #65109, .T. ) ;
#62601 = DIRECTION ( 'NONE',  ( 0.000000000000000000, 0.000000000000000000, -1.000000000000000000 ) ) ;
#62602 = ADVANCED_FACE ( 'NONE', ( #95028 ), #17404, .T. ) ;
#62603 = VECTOR ( 'NONE', #13436, 1000.000000000000000 ) ;
#62604 = CARTESIAN_POINT ( 'NONE',  ( -64.62287095715005592, -23.72747288104470087, -1.053458166803226348 ) ) ;
#62605 = B_SPLINE_CURVE_WITH_KNOTS ( 'NONE', 3,
 ( #12695, #36041, #19805, #81722 ),
 .UNSPECIFIED., .F., .F.,
 ( 4, 4 ),
 ( 0.000000000000000000, 9.999999999998897304E-05 ),
 .UNSPECIFIED. ) ;
#62606 = B_SPLINE_CURVE_WITH_KNOTS ( 'NONE', 3,
 ( #72099, #87812, #72595, #34026 ),
 .UNSPECIFIED., .F., .F.,
 ( 4, 4 ),
 ( 0.8994249224030640422, 0.9004256694438294018 ),
 .UNSPECIFIED. ) ;
#62607 = CARTESIAN_POINT ( 'NONE',  ( -93.62801294614813230, -24.35071581493543391, 9.817618358456016381 ) ) ;
#62608 = CARTESIAN_POINT ( 'NONE',  ( 16.91694316922610497, -9.995573847407506207, 11.49999999999998934 ) ) ;
#62609 = CARTESIAN_POINT ( 'NONE',  ( -41.46379453422112249, -25.27805965137699218, 4.278542394115019576 ) ) ;
#62610 = VERTEX_POINT ( 'NONE', #25517 ) ;
#62611 = CARTESIAN_POINT ( 'NONE',  ( -19.30636564405121902, 9.640216152154000184, 11.49999999999998934 ) ) ;
#62612 = CARTESIAN_POINT ( 'NONE',  ( -40.54156941310200324, -24.40034930558990922, 0.3402023900116037947 ) ) ;
#62613 = CARTESIAN_POINT ( 'NONE',  ( -78.52287095715006160, -23.47593901973090169, -1.443836447538996648 ) ) ;
#62614 = CARTESIAN_POINT ( 'NONE',  ( 22.67273400128462058, 4.441195646929153362, -1.500000000000002220 ) ) ;
#62615 = CIRCLE ( 'NONE', #57771, 129.7684398600581517 ) ;
#62616 = COORDINATED_UNIVERSAL_TIME_OFFSET ( 0, 0, .AHEAD. ) ;
#62617 = PLANE ( 'NONE',  #64517 ) ;
#62618 = CARTESIAN_POINT ( 'NONE',  ( -130.5728709571500588, -23.50395946778992595, -1.461890965025840927 ) ) ;
#62619 = CARTESIAN_POINT ( 'NONE',  ( -20.27875734969026311, -4.776774720514394446, 25.40402280011861080 ) ) ;
#62620 = PLANE ( 'NONE',  #51549 ) ;
#62621 = CIRCLE ( 'NONE', #78811, 252.4458649670781085 ) ;
#62623 = CARTESIAN_POINT ( 'NONE',  ( -110.0874522194761056, -25.18851129330323602, 3.319341060603216764 ) ) ;
#62622 = CIRCLE ( 'NONE', #65905, 1.000000000000000000 ) ;
#62624 = CARTESIAN_POINT ( 'NONE',  ( -129.6237315874382432, -23.96119346886881019, -0.6495511937831975890 ) ) ;
#62625 = CARTESIAN_POINT ( 'NONE',  ( -111.3439979973304332, -25.18425758082677746, 4.101024256656019773 ) ) ;
#62627 = ADVANCED_FACE ( 'NONE', ( #66110 ), #48364, .F. ) ;
#62626 = CARTESIAN_POINT ( 'NONE',  ( -19.25010300378637851, 5.133817055790010464, -1.500000000000002220 ) ) ;
#62628 = CARTESIAN_POINT ( 'NONE',  ( -113.6228709571500559, -24.64898659630368627, 1.056161002820831474 ) ) ;
#62629 = CARTESIAN_POINT ( 'NONE',  ( 4.927431051831622000, -19.18327824014073357, -1.500000000000002220 ) ) ;
#62630 = VECTOR ( 'NONE', #35430, 1000.000000000000114 ) ;
#62631 = CARTESIAN_POINT ( 'NONE',  ( -56.56717033891496982, -23.48783264082477018, -1.443836473390095909 ) ) ;
#62632 = B_SPLINE_CURVE_WITH_KNOTS ( 'NONE', 3,
 ( #8210, #7702, #14801, #16313 ),
 .UNSPECIFIED., .F., .F.,
 ( 4, 4 ),
 ( 0.000000000000000000, 9.999999999998206125E-05 ),
 .UNSPECIFIED. ) ;
#62633 = CARTESIAN_POINT ( 'NONE',  ( 6.660000000000001030, -9.572916487583196243, -0.7764348688322058045 ) ) ;
#62634 = FACE_OUTER_BOUND ( 'NONE', #90733, .T. ) ;
#62635 = CARTESIAN_POINT ( 'NONE',  ( 8.056674255711671506, 19.11000797562349618, 11.49999999999999645 ) ) ;
#62636 = DIRECTION ( 'NONE',  ( 1.000000000000000000, 3.773278334444167608E-23, 8.201307833595939069E-29 ) ) ;
#62637 = EDGE_CURVE ( 'NONE', #26765, #81702, #83597, .T. ) ;
#62638 = CARTESIAN_POINT ( 'NONE',  ( -88.62287095715002749, -23.72747288104441665, -1.053458166803660889 ) ) ;
#62639 = CARTESIAN_POINT ( 'NONE',  ( 18.68554041145753786, -12.99315341008173519, 11.49999999999999645 ) ) ;
#62640 = ORIENTED_EDGE ( 'NONE', *, *, #49595, .F. ) ;
#62641 = CARTESIAN_POINT ( 'NONE',  ( -69.63557792188336748, -24.15543982623907127, -0.2315651400026648155 ) ) ;
#62642 = ADVANCED_FACE ( 'NONE', ( #56491 ), #96525, .T. ) ;
#62643 = CARTESIAN_POINT ( 'NONE',  ( -4.993225604111835914, 5.965225279485592225, -29.11654937215278593 ) ) ;
#62644 = ORIENTED_EDGE ( 'NONE', *, *, #81316, .T. ) ;
#62645 = B_SPLINE_CURVE_WITH_KNOTS ( 'NONE', 3,
 ( #43559, #66908, #26830, #97829 ),
 .UNSPECIFIED., .F., .F.,
 ( 4, 4 ),
 ( 0.000000000000000000, 9.999999999997510880E-05 ),
 .UNSPECIFIED. ) ;
#62646 = CARTESIAN_POINT ( 'NONE',  ( -9.470923242388245455, -17.85692771776473364, -1.500000000000002220 ) ) ;
#62647 = FACE_OUTER_BOUND ( 'NONE', #20479, .T. ) ;
#62648 = ADVANCED_FACE ( 'NONE', ( #18896 ), #80304, .T. ) ;
#62649 = LINE ( 'NONE', #16446, #43155 ) ;
#62650 = VECTOR ( 'NONE', #22705, 1000.000000000000000 ) ;
#62651 = ORIENTED_EDGE ( 'NONE', *, *, #86421, .F. ) ;
#62652 = EDGE_CURVE ( 'NONE', #80103, #39944, #72769, .T. ) ;
#62653 = ORIENTED_EDGE ( 'NONE', *, *, #13033, .T. ) ;
#62654 = LINE ( 'NONE', #40798, #77627 ) ;
#62655 = CARTESIAN_POINT ( 'NONE',  ( 10.67403711042701353, -20.27515232684288549, -1.500000000000002220 ) ) ;
#62657 = EDGE_CURVE ( 'NONE', #26067, #86027, #65607, .T. ) ;
#62656 = CARTESIAN_POINT ( 'NONE',  ( -41.15328318997018897, -25.14988170789391830, 3.000103590172058077 ) ) ;
#62658 = CARTESIAN_POINT ( 'NONE',  ( -0.6006773669993965559, 21.62980403441659760, -1.500000000000002220 ) ) ;
#62659 = CARTESIAN_POINT ( 'NONE',  ( -104.6228709571500985, -24.34917612406837861, 0.1852690917426659811 ) ) ;
#62660 = CARTESIAN_POINT ( 'NONE',  ( 13.94627346685978075, -15.57361473980792255, 11.49999999999999645 ) ) ;
#62661 = ORIENTED_EDGE ( 'NONE', *, *, #30809, .F. ) ;
#62662 = DIRECTION ( 'NONE',  ( -0.000000000000000000, 1.000000000000000000, -0.000000000000000000 ) ) ;
#62663 = CARTESIAN_POINT ( 'NONE',  ( -103.5228709571500758, -24.64965694238408034, 8.947790433994194714 ) ) ;
#62664 = CARTESIAN_POINT ( 'NONE',  ( -18.71521858236628333, -11.60751834597489740, -1.500000000000002220 ) ) ;
#62665 = CARTESIAN_POINT ( 'NONE',  ( -4.141025641025642301, -6.376774720514408301, 19.19230769230769695 ) ) ;
#62666 = CARTESIAN_POINT ( 'NONE',  ( -30.57287095715006231, -23.48210175247266562, -1.443836490256470428 ) ) ;
#62667 = VERTEX_POINT ( 'NONE', #27021 ) ;
#62668 = CARTESIAN_POINT ( 'NONE',  ( -49.68454138742491466, -25.18440160747184464, 3.564592644700640189 ) ) ;
#62669 = CARTESIAN_POINT ( 'NONE',  ( 3.036358173076929123, -6.376774720514420736, 20.87990785256409865 ) ) ;
#62670 = ORIENTED_EDGE ( 'NONE', *, *, #15691, .T. ) ;
#62671 = CARTESIAN_POINT ( 'NONE',  ( 2.790451961050095520, -6.376774720514408301, 18.85195250256714417 ) ) ;
#62672 = ORIENTED_EDGE ( 'NONE', *, *, #66531, .F. ) ;
#62673 = B_SPLINE_CURVE_WITH_KNOTS ( 'NONE', 3,
 ( #10984, #96711, #41949, #41437 ),
 .UNSPECIFIED., .F., .F.,
 ( 4, 4 ),
 ( 0.05879740816001716858, 0.05979815520078245183 ),
 .UNSPECIFIED. ) ;
#62674 = ORIENTED_EDGE ( 'NONE', *, *, #92973, .F. ) ;
#62675 = CARTESIAN_POINT ( 'NONE',  ( -71.55402431509982364, -23.96169478059713498, 10.65365249895718058 ) ) ;
#62676 = CARTESIAN_POINT ( 'NONE',  ( -101.7453191491394477, -25.10936024163003211, 3.852396405368743171 ) ) ;
#62677 = CARTESIAN_POINT ( 'NONE',  ( -4.854568188115255367, -6.376774720514410077, 19.46611907402017394 ) ) ;
#62678 = CARTESIAN_POINT ( 'NONE',  ( -20.44062828730913139, -1.133067592104922694, -1.500000000000002220 ) ) ;
#62679 = ORIENTED_EDGE ( 'NONE', *, *, #52235, .T. ) ;
#62680 = CARTESIAN_POINT ( 'NONE',  ( -71.62287095715005592, -24.66019654487199020, 8.947790411086131712 ) ) ;
#62681 = CARTESIAN_POINT ( 'NONE',  ( -4.686006777320704586, 6.376774720514426953, 29.60911411231905888 ) ) ;
#62682 = CARTESIAN_POINT ( 'NONE',  ( -56.62287095715007013, -24.50216790748205042, 0.6166512839542496183 ) ) ;
#62683 = CARTESIAN_POINT ( 'NONE',  ( 21.78807519107708401, 4.755904613692067073, 11.49999999999998934 ) ) ;
#62684 = AXIS2_PLACEMENT_3D ( 'NONE', #75432, #99757, #6438 ) ;
#62685 = LINE ( 'NONE', #62182, #15704 ) ;
#62686 = CARTESIAN_POINT ( 'NONE',  ( -1.409217194013772101, -5.876774720514418071, 20.11414146978959749 ) ) ;
#62687 = ORIENTED_EDGE ( 'NONE', *, *, #64019, .F. ) ;
#62688 = CARTESIAN_POINT ( 'NONE',  ( -29.78660512628383472, -25.21957512536681989, 4.203493191755291569 ) ) ;
#62689 = DIRECTION ( 'NONE',  ( -0.000000000000000000, 1.000000000000000000, -0.000000000000000000 ) ) ;
#62690 = B_SPLINE_CURVE_WITH_KNOTS ( 'NONE', 3,
 ( #71458, #26271, #25770, #17657, #1445, #41502 ),
 .UNSPECIFIED., .F., .F.,
 ( 4, 2, 4 ),
 ( 0.000000000000000000, 0.001380901958385383774, 0.002761803916770767548 ),
 .UNSPECIFIED. ) ;
#62691 = CARTESIAN_POINT ( 'NONE',  ( -19.76906661924035191, -6.534152953431121347, -1.500000000000002220 ) ) ;
#62692 = ORIENTED_EDGE ( 'NONE', *, *, #39127, .F. ) ;
#62694 = VERTEX_POINT ( 'NONE', #9790 ) ;
#62693 = CARTESIAN_POINT ( 'NONE',  ( -0.4909855769230799249, -6.376774720514410077, 19.14743589743590491 ) ) ;
#62695 = AXIS2_PLACEMENT_3D ( 'NONE', #74864, #5368, #44439 ) ;
#62696 = ORIENTED_EDGE ( 'NONE', *, *, #36745, .F. ) ;
#62697 = DIRECTION ( 'NONE',  ( 0.000000000000000000, 0.000000000000000000, -1.000000000000000000 ) ) ;
#62698 = CARTESIAN_POINT ( 'NONE',  ( -0.6469382494902750080, 20.97623560764392181, -1.500000000000002220 ) ) ;
#62699 = ORIENTED_EDGE ( 'NONE', *, *, #29102, .F. ) ;
#62700 = AXIS2_PLACEMENT_3D ( 'NONE', #18013, #40848, #70809 ) ;
#62701 = CARTESIAN_POINT ( 'NONE',  ( -110.6228709571500701, -24.51163499207180152, 0.6490370598555511572 ) ) ;
#62702 = CARTESIAN_POINT ( 'NONE',  ( -28.84663072490566194, 5.965225279485572685, 28.73989617533406715 ) ) ;
#62703 = CARTESIAN_POINT ( 'NONE',  ( 9.464509667910858681, -5.356774720513593380, -27.03659963401723942 ) ) ;
#62704 = VECTOR ( 'NONE', #36731, 1000.000000000000114 ) ;
#62705 = LINE ( 'NONE', #84519, #25879 ) ;
#62706 = CARTESIAN_POINT ( 'NONE',  ( -59.57900456839059444, -24.65952944569304961, 1.056160979905697905 ) ) ;
#62707 = DIRECTION ( 'NONE',  ( -0.000000000000000000, 1.000000000000000000, -0.000000000000000000 ) ) ;
#62709 = ORIENTED_EDGE ( 'NONE', *, *, #73518, .F. ) ;
#62708 = CARTESIAN_POINT ( 'NONE',  ( 17.07819277939130842, -14.19623557145530057, 11.49999999999999645 ) ) ;
#62710 = CARTESIAN_POINT ( 'NONE',  ( -4.444543648262984981, 12.92677669529668627, 2.100000000000000089 ) ) ;
#62711 = CARTESIAN_POINT ( 'NONE',  ( -38.62287095715005592, -24.65952944569303895, 1.056160979905692798 ) ) ;
#62712 = ORIENTED_EDGE ( 'NONE', *, *, #31679, .F. ) ;
#62713 = B_SPLINE_CURVE_WITH_KNOTS ( 'NONE', 3,
 ( #43283, #28051, #83822, #29529 ),
 .UNSPECIFIED., .F., .F.,
 ( 4, 4 ),
 ( 0.000000000000000000, 0.0001000000000000167422 ),
 .UNSPECIFIED. ) ;
#62714 = CARTESIAN_POINT ( 'NONE',  ( -5.639450322166912777, -21.95568564230989850, -1.500000000000002220 ) ) ;
#62715 = VECTOR ( 'NONE', #79179, 1000.000000000000114 ) ;
#62717 = ORIENTED_EDGE ( 'NONE', *, *, #83651, .F. ) ;
#62716 = CARTESIAN_POINT ( 'NONE',  ( -76.62287095715007013, -24.64898659630367916, 1.056161002820826145 ) ) ;
#62718 = ORIENTED_EDGE ( 'NONE', *, *, #22910, .T. ) ;
#62719 = DIRECTION ( 'NONE',  ( -0.000000000000000000, 1.000000000000000000, -0.000000000000000000 ) ) ;
#62720 = EDGE_CURVE ( 'NONE', #85245, #55779, #82306, .T. ) ;
#62721 = CARTESIAN_POINT ( 'NONE',  ( 5.670567493371958534, -19.34269084982597775, -1.500000000000002220 ) ) ;
#62722 = DIRECTION ( 'NONE',  ( -3.773278334453079030E-23, 0.9999999999976377785, 2.173523156925979128E-06 ) ) ;
#62723 = VERTEX_POINT ( 'NONE', #50367 ) ;
#62724 = CARTESIAN_POINT ( 'NONE',  ( 14.70320764097976074, -3.414808732104013256, -28.39448918867740446 ) ) ;
#62725 = CARTESIAN_POINT ( 'NONE',  ( 21.16571772479873204, -7.350578744355993344, -1.500000000000002220 ) ) ;
#62726 = VERTEX_POINT ( 'NONE', #55987 ) ;
#62727 = VERTEX_POINT ( 'NONE', #35139 ) ;
#62728 = CARTESIAN_POINT ( 'NONE',  ( -101.2523990460597503, -25.16257427658810641, 6.807414179791832609 ) ) ;
#62729 = CARTESIAN_POINT ( 'NONE',  ( -4.141025641025642301, -5.876774720514411854, 19.63681891025641235 ) ) ;
#62730 = CARTESIAN_POINT ( 'NONE',  ( -39.93645079509425244, -25.31561181395491289, 4.983313389499331336 ) ) ;
#62731 = EDGE_CURVE ( 'NONE', #46085, #88746, #26014, .T. ) ;
#62732 = VECTOR ( 'NONE', #92008, 1000.000000000000000 ) ;
#62733 = EDGE_CURVE ( 'NONE', #38686, #1347, #64107, .T. ) ;
#62734 = CARTESIAN_POINT ( 'NONE',  ( 32.84232313084847732, 4.840274619473232676, -11.71291885348859196 ) ) ;
#62735 = EDGE_CURVE ( 'NONE', #3834, #97929, #17908, .T. ) ;
#62736 = CARTESIAN_POINT ( 'NONE',  ( -130.5728709571500588, -24.47827083238276202, 0.5637492489085990099 ) ) ;
#62737 = CARTESIAN_POINT ( 'NONE',  ( -1.979602623192304955, -19.45764201480039901, -1.500000000000002220 ) ) ;
#62738 = CARTESIAN_POINT ( 'NONE',  ( -39.52287095715006870, -23.47596703998600631, 11.44779298504229281 ) ) ;
#62740 = EDGE_CURVE ( 'NONE', #76298, #36478, #56984, .T. ) ;
#62739 = VERTEX_POINT ( 'NONE', #33635 ) ;
#62741 = CARTESIAN_POINT ( 'NONE',  ( 3.930203739357332360, 21.12693704021120666, -1.500000000000002220 ) ) ;
#62742 = AXIS2_PLACEMENT_3D ( 'NONE', #71698, #33125, #26012 ) ;
#62743 = CARTESIAN_POINT ( 'NONE',  ( -62.52287095715006160, -23.73934037231757088, 11.05740245334329153 ) ) ;
#62744 = CARTESIAN_POINT ( 'NONE',  ( -38.62287095715005592, -23.47593901973091235, -1.443836447539011525 ) ) ;
#62745 = CARTESIAN_POINT ( 'NONE',  ( -59.58953762381671027, -23.48783264082478794, -1.443836473390069042 ) ) ;
#62746 = CARTESIAN_POINT ( 'NONE',  ( -111.6228709571500559, -23.48783264082479505, -1.443836473390060604 ) ) ;
#62747 = CARTESIAN_POINT ( 'NONE',  ( -21.29394331855728240, -8.360804490491451801, -1.500000000000002220 ) ) ;
#62748 = APPROVAL_DATE_TIME ( #76432, #80452 ) ;
#62749 = CARTESIAN_POINT ( 'NONE',  ( -101.5228709571500758, -23.47593901973090524, -1.443836447538996426 ) ) ;
#62750 = CARTESIAN_POINT ( 'NONE',  ( -92.62287095715005592, -24.33832256527048088, 0.1851278514138620102 ) ) ;
#62751 = CARTESIAN_POINT ( 'NONE',  ( -17.62595516807937557, -9.487554784798948759, 11.49999999999999645 ) ) ;
#62752 = CARTESIAN_POINT ( 'NONE',  ( -80.30894842687054336, -25.31594316168605374, 4.506568925094878608 ) ) ;
#62753 = CARTESIAN_POINT ( 'NONE',  ( -87.52287095715006160, -24.64965694238575011, 8.947790433994196491 ) ) ;
#62754 = LINE ( 'NONE', #54628, #79790 ) ;
#62755 = CARTESIAN_POINT ( 'NONE',  ( -37.52287095715006870, -29.50250786944525672, 11.44777988621624232 ) ) ;
#62756 = ORIENTED_EDGE ( 'NONE', *, *, #75076, .T. ) ;
#62757 = DIRECTION ( 'NONE',  ( 0.000000000000000000, 0.000000000000000000, 1.000000000000000000 ) ) ;
#62758 = EDGE_CURVE ( 'NONE', #1553, #48376, #48279, .T. ) ;
#62759 = CARTESIAN_POINT ( 'NONE',  ( 21.64095104908334122, -2.195182070091274529, -1.500000000000002220 ) ) ;
#62760 = DIRECTION ( 'NONE',  ( 0.000000000000000000, 1.000000000000000000, 0.000000000000000000 ) ) ;
#62761 = CARTESIAN_POINT ( 'NONE',  ( -3.718233408413001762, 19.32670252783854536, -1.500000000000002220 ) ) ;
#62762 = AXIS2_PLACEMENT_3D ( 'NONE', #15654, #46623, #431 ) ;
#62763 = CARTESIAN_POINT ( 'NONE',  ( -122.6228709571500843, -23.96127896941633750, -0.6493128931037740470 ) ) ;
#62764 = ADVANCED_FACE ( 'NONE', ( #68078 ), #90386, .T. ) ;
#62765 = CARTESIAN_POINT ( 'NONE',  ( -109.5056412146432052, -25.27925783859062037, 4.749485557442086225 ) ) ;
#62766 = CONTEXT_DEPENDENT_SHAPE_REPRESENTATION ( #12904, #11767 ) ;
#62767 = DIRECTION ( 'NONE',  ( 0.4725087886537609472, -0.000000000000000000, 0.8813259582271223413 ) ) ;
#62768 = CARTESIAN_POINT ( 'NONE',  ( -73.62287095715008434, -24.35013146730204525, 9.818937971375108376 ) ) ;
#62769 = CARTESIAN_POINT ( 'NONE',  ( 11.66944253441096002, 16.90307425063352298, 11.49999999999999645 ) ) ;
#62770 = CARTESIAN_POINT ( 'NONE',  ( 25.61870917940689196, 5.965225279485572685, 29.49402280011862487 ) ) ;
#62771 = EDGE_CURVE ( 'NONE', #65202, #27379, #97026, .T. ) ;
#62772 = AXIS2_PLACEMENT_3D ( 'NONE', #100051, #86738, #17227 ) ;
#62773 = CARTESIAN_POINT ( 'NONE',  ( -120.6249283607330085, -24.63355581998386157, 0.9682620441943888823 ) ) ;
#62774 = CARTESIAN_POINT ( 'NONE',  ( 1.383477600506065164, -22.57338898373578218, 11.49999999999999645 ) ) ;
#62775 = ORIENTED_EDGE ( 'NONE', *, *, #50981, .T. ) ;
#62776 = CARTESIAN_POINT ( 'NONE',  ( -83.52287095715006160, -23.47596703998600631, 11.44779298504228571 ) ) ;
#62777 = CARTESIAN_POINT ( 'NONE',  ( -26.71433665274188130, -24.81880000428164124, 7.190069475304298408 ) ) ;
#62778 = CARTESIAN_POINT ( 'NONE',  ( -97.63857696127199404, -23.48783264082477018, -1.443836473390088360 ) ) ;
#62779 = PLANE ( 'NONE',  #30503 ) ;
#62780 = AXIS2_PLACEMENT_3D ( 'NONE', #29371, #7036, #85663 ) ;
#62781 = CARTESIAN_POINT ( 'NONE',  ( -25.53098197642538736, -24.61459394604217010, 4.942812361920813302 ) ) ;
#62782 = EDGE_CURVE ( 'NONE', #6498, #28719, #44744, .T. ) ;
#62783 = CARTESIAN_POINT ( 'NONE',  ( -2.794644232660540961, -6.376774720514415407, 20.26757654895259009 ) ) ;
#62784 = EDGE_CURVE ( 'NONE', #33865, #62952, #75080, .T. ) ;
#62785 = VERTEX_POINT ( 'NONE', #83288 ) ;
#62786 = CARTESIAN_POINT ( 'NONE',  ( -79.51137944035450289, -25.31596313913097873, 5.389239573282282869 ) ) ;
#62787 = CARTESIAN_POINT ( 'NONE',  ( 7.682656365740156090, -21.48159684637525046, -1.500000000000002220 ) ) ;
#62788 = CARTESIAN_POINT ( 'NONE',  ( -74.62680018750160116, -24.51314013834315375, 0.6176544820404124003 ) ) ;
#62789 = CARTESIAN_POINT ( 'NONE',  ( -96.58652322487247943, -24.51314013834316086, 0.6176544820404182845 ) ) ;
#62790 = CARTESIAN_POINT ( 'NONE',  ( -119.5895376238167245, -24.64898659630368627, 1.056161002820393602 ) ) ;
#62791 = CARTESIAN_POINT ( 'NONE',  ( 15.70178742502441693, -15.98865493379879332, 11.49999999999999645 ) ) ;
#62792 = ORIENTED_EDGE ( 'NONE', *, *, #46281, .F. ) ;
#62793 = CARTESIAN_POINT ( 'NONE',  ( -70.62287095715001328, -24.63345952396257488, 9.038047939301510070 ) ) ;
#62794 = EDGE_CURVE ( 'NONE', #29229, #69616, #6664, .T. ) ;
#62795 = CARTESIAN_POINT ( 'NONE',  ( -21.91604229967229500, -0.6759211909499470705, 11.49999999999998934 ) ) ;
#62796 = LINE ( 'NONE', #369, #89981 ) ;
#62797 = B_SPLINE_CURVE_WITH_KNOTS ( 'NONE', 3,
 ( #50930, #60543, #28087, #6231 ),
 .UNSPECIFIED., .F., .F.,
 ( 4, 4 ),
 ( 3.895932028743765719E-09, 0.001954337564626884745 ),
 .UNSPECIFIED. ) ;
#62798 = CARTESIAN_POINT ( 'NONE',  ( -44.62857276611402568, -24.51419770103159834, 9.386484678747169852 ) ) ;
#62799 = PLANE ( 'NONE',  #53561 ) ;
#62800 = ORIENTED_EDGE ( 'NONE', *, *, #87319, .T. ) ;
#62801 = CARTESIAN_POINT ( 'NONE',  ( 30.53060340732036337, -4.132774720517318201, 3.744237563515920634E-15 ) ) ;
#62802 = LINE ( 'NONE', #93716, #97077 ) ;
#62803 = ORIENTED_EDGE ( 'NONE', *, *, #67515, .F. ) ;
#62804 = CARTESIAN_POINT ( 'NONE',  ( -20.46784169311667867, 0.4426517378232717737, 11.49999999999998934 ) ) ;
#62805 = ORIENTED_EDGE ( 'NONE', *, *, #100198, .F. ) ;
#62806 = ORIENTED_EDGE ( 'NONE', *, *, #98727, .T. ) ;
#62807 = VERTEX_POINT ( 'NONE', #75665 ) ;
#62808 = ORIENTED_EDGE ( 'NONE', *, *, #22368, .F. ) ;
#62809 = CARTESIAN_POINT ( 'NONE',  ( -3.381418692465893105, -22.81955385325859709, 11.49999999999998934 ) ) ;
#62810 = CARTESIAN_POINT ( 'NONE',  ( -40.11496927896248366, -25.30524842186639844, 5.093185296294494790 ) ) ;
#62811 = CARTESIAN_POINT ( 'NONE',  ( 11.02309159617336221, -17.05227643984133934, -1.500000000000002220 ) ) ;
#62812 = VERTEX_POINT ( 'NONE', #6166 ) ;
#62813 = AXIS2_PLACEMENT_3D ( 'NONE', #56849, #32996, #64474 ) ;
#62814 = CYLINDRICAL_SURFACE ( 'NONE', #42874, 2.040000000000000036 ) ;
#62815 = CARTESIAN_POINT ( 'NONE',  ( 9.315600972258339496, 6.376774720514426953, 28.35070303307545458 ) ) ;
#62816 = CARTESIAN_POINT ( 'NONE',  ( -113.2228709571500502, -23.47593901973090524, -1.443836447538996426 ) ) ;
#62817 = CARTESIAN_POINT ( 'NONE',  ( -97.92287095715008149, -23.47596703998600276, 11.44779298504227860 ) ) ;
#62819 = ORIENTED_EDGE ( 'NONE', *, *, #14530, .T. ) ;
#62818 = CARTESIAN_POINT ( 'NONE',  ( -17.67684169981329845, 12.20363403927300183, 11.49999999999999645 ) ) ;
#62820 = CARTESIAN_POINT ( 'NONE',  ( -125.5562042904833930, -24.99132157543167310, 2.256160258750667946 ) ) ;
#62821 = CARTESIAN_POINT ( 'NONE',  ( -34.62287095715005592, -24.33832256527048088, 0.1851278514138579023 ) ) ;
#62822 = ORIENTED_EDGE ( 'NONE', *, *, #65079, .F. ) ;
#62823 = AXIS2_PLACEMENT_3D ( 'NONE', #38744, #83928, #39746 ) ;
#62824 = CARTESIAN_POINT ( 'NONE',  ( -2.856624844580134770, 20.53689577262001364, -1.500000000000002220 ) ) ;
#62825 = ORIENTED_EDGE ( 'NONE', *, *, #6706, .T. ) ;
#62827 = ORIENTED_EDGE ( 'NONE', *, *, #24045, .T. ) ;
#62826 = CARTESIAN_POINT ( 'NONE',  ( -125.5222534793145854, -23.48783264082478794, -1.443836473390061936 ) ) ;
#62828 = B_SPLINE_SURFACE_WITH_KNOTS ( 'NONE', 3, 3, ( 
 ( #30029, #60514, #61003, #68608 ),
 ( #91937, #4717, #67621, #98041 ),
 ( #91427, #89944, #21907, #29035 ),
 ( #51391, #35668, #74707, #76203 ),
 ( #82329, #43779, #37652, #5206 ),
 ( #20919, #70106, #23402, #46773 ),
 ( #47275, #9199, #71115, #38143 ) ),
 .UNSPECIFIED., .F., .F., .F.,
 ( 4, 3, 4 ),
 ( 4, 4 ),
 ( 0.0004766839783846337159, 0.1029713700210910243, 0.2054660560637974198 ),
 ( 0.2295523914546782895, 0.2306710310623432680 ),
 .UNSPECIFIED. ) ;
#62829 = CARTESIAN_POINT ( 'NONE',  ( -41.54628241281430689, -24.15620529776627734, 10.23563542870660825 ) ) ;
#62830 = DIRECTION ( 'NONE',  ( -3.773278334453079030E-23, 0.9999999999976377785, 2.173523156925979128E-06 ) ) ;
#62831 = EDGE_LOOP ( 'NONE', ( #89534, #55301, #47962, #62313 ) ) ;
#62832 = ORIENTED_EDGE ( 'NONE', *, *, #30542, .F. ) ;
#62833 = CARTESIAN_POINT ( 'NONE',  ( -109.5228709571500616, -23.47596703998600631, 11.44779298504228038 ) ) ;
#62834 = CARTESIAN_POINT ( 'NONE',  ( -42.52203033503141683, -23.48786465467240347, 11.44779295918255535 ) ) ;
#62835 = CARTESIAN_POINT ( 'NONE',  ( -78.52287095715000476, -23.94994826722564696, -0.6494450866342719175 ) ) ;
#62836 = CARTESIAN_POINT ( 'NONE',  ( -7.037580251249667462, -20.86201633182841420, 11.49999999999999645 ) ) ;
#62837 = CARTESIAN_POINT ( 'NONE',  ( -29.49875734969026198, 5.965225279485572685, 10.11402280011862587 ) ) ;
#62838 = CARTESIAN_POINT ( 'NONE',  ( -14.53490578827140212, -17.26895500059623956, 11.49999999999998934 ) ) ;
#62839 = AXIS2_PLACEMENT_3D ( 'NONE', #69075, #34763, #60978 ) ;
#62840 = CARTESIAN_POINT ( 'NONE',  ( 3.785439364192078937, -20.66625369722972749, 11.49999999999998934 ) ) ;
#62841 = DIRECTION ( 'NONE',  ( 7.960204194457801640E-17, 1.000000000000000000, 2.891205793294678326E-16 ) ) ;
#62843 = EDGE_LOOP ( 'NONE', ( #92793, #45476, #88759, #46176 ) ) ;
#62842 = PLANE ( 'NONE',  #97650 ) ;
#62844 = ORIENTED_EDGE ( 'NONE', *, *, #30239, .F. ) ;
#62845 = CARTESIAN_POINT ( 'NONE',  ( -80.62287095715005592, -23.84047902841602351, -0.8780736468305712084 ) ) ;
#62846 = VECTOR ( 'NONE', #22436, 1000.000000000000114 ) ;
#62847 = B_SPLINE_CURVE_WITH_KNOTS ( 'NONE', 1,
 ( #54647, #86081 ),
 .UNSPECIFIED., .F., .F.,
 ( 2, 2 ),
 ( 0.000000000000000000, 1.000000000000000000 ),
 .UNSPECIFIED. ) ;
#62848 = DIRECTION ( 'NONE',  ( -0.000000000000000000, -1.000000000000000000, -0.000000000000000000 ) ) ;
#62849 = EDGE_LOOP ( 'NONE', ( #37728, #15466, #50089, #63192 ) ) ;
#62850 = CARTESIAN_POINT ( 'NONE',  ( 16.66693084842116335, 13.01107939256401913, -1.500000000000002220 ) ) ;
#62851 = CARTESIAN_POINT ( 'NONE',  ( 27.53860345374771867, 1.477225279485574028, -9.482392034746242260 ) ) ;
#62852 = ADVANCED_FACE ( 'NONE', ( #43745 ), #44221, .T. ) ;
#62853 = CARTESIAN_POINT ( 'NONE',  ( -60.72545834919631602, -25.33009847151395633, 4.495758292450051208 ) ) ;
#62854 = CARTESIAN_POINT ( 'NONE',  ( -41.52287095715006870, -29.50250243563736774, 8.947779886222148704 ) ) ;
#62855 = FACE_OUTER_BOUND ( 'NONE', #7482, .T. ) ;
#62857 = B_SPLINE_CURVE_WITH_KNOTS ( 'NONE', 3,
 ( #13840, #51428, #82363, #76234 ),
 .UNSPECIFIED., .F., .F.,
 ( 4, 4 ),
 ( 0.000000000000000000, 0.0001000000000000028644 ),
 .UNSPECIFIED. ) ;
#62856 = DIRECTION ( 'NONE',  ( 0.7689940216596069522, -5.365801633547218220E-16, -0.6392559695863496705 ) ) ;
#62858 = CARTESIAN_POINT ( 'NONE',  ( -2.516727866726558460, 22.04588476715296963, -1.500000000000002220 ) ) ;
#62859 = EDGE_CURVE ( 'NONE', #25204, #94122, #32008, .T. ) ;
#62860 = CARTESIAN_POINT ( 'NONE',  ( -8.160000000000000142, -9.728493947732140157, 1.239948043688426926 ) ) ;
#62861 = ADVANCED_FACE ( 'NONE', ( #46232 ), #45734, .T. ) ;
#62862 = EDGE_LOOP ( 'NONE', ( #80147, #40194, #87340, #23285 ) ) ;
#62863 = CARTESIAN_POINT ( 'NONE',  ( -51.72290159494567519, -25.31633202804502147, 5.484617888210121528 ) ) ;
#62864 = CARTESIAN_POINT ( 'NONE',  ( -48.62287095715003460, -24.33832256526968862, 0.1851278514119848728 ) ) ;
#62865 = CARTESIAN_POINT ( 'NONE',  ( -126.5899062329566505, -24.15543982623907482, -0.2315651400026573492 ) ) ;
#62866 = EDGE_CURVE ( 'NONE', #56809, #90981, #68575, .T. ) ;
#62867 = CARTESIAN_POINT ( 'NONE',  ( -85.52287095715004739, -24.99156044556120193, 7.747789690856173195 ) ) ;
#62868 = LINE ( 'NONE', #55247, #4847 ) ;
#62869 = CARTESIAN_POINT ( 'NONE',  ( 13.74000504945409418, 13.82049530813991467, 11.49999999999998934 ) ) ;
#62870 = CARTESIAN_POINT ( 'NONE',  ( -21.38522110535750542, 1.317000383210971792, -1.500000000000002220 ) ) ;
#62871 = CARTESIAN_POINT ( 'NONE',  ( -62.65462279266101575, -23.48783264082476308, -1.443836473390090580 ) ) ;
#62872 = CARTESIAN_POINT ( 'NONE',  ( -60.55142834745385727, -24.15602025861357660, 10.28564288302606933 ) ) ;
#62873 = CARTESIAN_POINT ( 'NONE',  ( -8.160000000000000142, -10.15233964170348457, 0.003711184059992174607 ) ) ;
#62874 = CYLINDRICAL_SURFACE ( 'NONE', #16814, 2.249999999999998668 ) ;
#62875 = CARTESIAN_POINT ( 'NONE',  ( -20.89466310375201985, -8.809181082428260368, -1.500000000000002220 ) ) ;
#62876 = EDGE_CURVE ( 'NONE', #5494, #47230, #87164, .T. ) ;
#62877 = CARTESIAN_POINT ( 'NONE',  ( -98.59358066329336623, -23.96119346886881019, -0.6495511937832081362 ) ) ;
#62878 = FACE_OUTER_BOUND ( 'NONE', #85878, .T. ) ;
#62879 = CARTESIAN_POINT ( 'NONE',  ( -17.31707178780640533, -9.736581320607820444, 11.49999999999999645 ) ) ;
#62880 = CARTESIAN_POINT ( 'NONE',  ( -123.5194348897975516, -24.51419770103158768, 9.386484678747160970 ) ) ;
#62881 = CARTESIAN_POINT ( 'NONE',  ( 8.271845302688323187, -0.3854532800250802249, 3.722136940144805450 ) ) ;
#62882 = DIRECTION ( 'NONE',  ( 0.000000000000000000, 0.000000000000000000, -1.000000000000000000 ) ) ;
#62883 = EDGE_LOOP ( 'NONE', ( #58418, #4143, #99536, #70623 ) ) ;
#62884 = CARTESIAN_POINT ( 'NONE',  ( 29.93983266611829563, 5.350981799920698556, 19.84760796525321780 ) ) ;
#62885 = CARTESIAN_POINT ( 'NONE',  ( 13.91401389203221406, -6.475225279485573360, 158.0376437107427137 ) ) ;
#62886 = CARTESIAN_POINT ( 'NONE',  ( -51.70072539166533687, -25.10936008140465248, 3.987152415576288522 ) ) ;
#62887 = CARTESIAN_POINT ( 'NONE',  ( -18.45943378446990835, 11.37049804852326140, -1.500000000000002220 ) ) ;
#62888 = AXIS2_PLACEMENT_3D ( 'NONE', #54595, #62719, #7908 ) ;
#62889 = FACE_OUTER_BOUND ( 'NONE', #50758, .T. ) ;
#62890 = CARTESIAN_POINT ( 'NONE',  ( 16.53150372360616771, 10.32350692489952593, -1.500000000000002220 ) ) ;
#62891 = CARTESIAN_POINT ( 'NONE',  ( -95.52287095715006160, -29.50249982740957577, 7.747779886224967605 ) ) ;
#62892 = ORIENTED_EDGE ( 'NONE', *, *, #2617, .T. ) ;
#62893 = CARTESIAN_POINT ( 'NONE',  ( -13.40315722217803973, 15.35114911505495172, 11.49999999999999645 ) ) ;
#62894 = CARTESIAN_POINT ( 'NONE',  ( -62.62287095715004881, -24.64898659630528854, 1.056161002820822592 ) ) ;
#62895 = DIRECTION ( 'NONE',  ( -3.773278334453079618E-23, 0.9999999999976377785, 2.173523156925979975E-06 ) ) ;
#62896 = VERTEX_POINT ( 'NONE', #54356 ) ;
#62897 = CARTESIAN_POINT ( 'NONE',  ( -79.01456066750945695, -25.21459190771157566, 6.490408043050610587 ) ) ;
#62898 = DIRECTION ( 'NONE',  ( 1.000000000000000000, 0.000000000000000000, 0.000000000000000000 ) ) ;
#62899 = CARTESIAN_POINT ( 'NONE',  ( -48.90136019426822145, -25.31602018323131986, 5.866402636874745724 ) ) ;
#62900 = CARTESIAN_POINT ( 'NONE',  ( -40.63662915703572054, -24.63419186844611630, 9.035850630976923981 ) ) ;
#62901 = CARTESIAN_POINT ( 'NONE',  ( -1.030996059302438761, -6.376774720514415407, 20.06599527532949878 ) ) ;
#62902 = CARTESIAN_POINT ( 'NONE',  ( 19.44710440357065551, 5.058846670610233076, 11.49999999999998934 ) ) ;
#62903 = CARTESIAN_POINT ( 'NONE',  ( -109.6310386362097518, -23.73766607897670156, -1.055555164236452681 ) ) ;
#62904 = VERTEX_POINT ( 'NONE', #62981 ) ;
#62905 = PLANE ( 'NONE',  #78679 ) ;
#62906 = AXIS2_PLACEMENT_3D ( 'NONE', #33781, #3354, #71853 ) ;
#62907 = ADVANCED_FACE ( 'NONE', ( #7669 ), #76658, .T. ) ;
#62908 = CARTESIAN_POINT ( 'NONE',  ( -18.82434810282327220, -12.99595988342530362, 11.49999999999999645 ) ) ;
#62909 = CARTESIAN_POINT ( 'NONE',  ( 1.118074629359579797, -22.68859683979520980, -1.500000000000002220 ) ) ;
#62910 = ORIENTED_EDGE ( 'NONE', *, *, #96853, .F. ) ;
#62911 = CARTESIAN_POINT ( 'NONE',  ( -53.62287095715003460, -24.51387760970723662, 9.387446482453425389 ) ) ;
#62912 = CYLINDRICAL_SURFACE ( 'NONE', #9080, 10.80000000000000782 ) ;
#62913 = PLANE ( 'NONE',  #98635 ) ;
#62914 = CARTESIAN_POINT ( 'NONE',  ( -49.52287095715009002, -23.96127896941631619, -0.6493128931038038010 ) ) ;
#62915 = EDGE_CURVE ( 'NONE', #26478, #45688, #66671, .T. ) ;
#62916 = CIRCLE ( 'NONE', #56399, 22.69500000000000384 ) ;
#62917 = CARTESIAN_POINT ( 'NONE',  ( -128.5220659786135116, -23.73791477778912551, 11.05961554403169522 ) ) ;
#62918 = DIRECTION ( 'NONE',  ( 0.7071067811865435759, 0.7071067811865515695, -0.000000000000000000 ) ) ;
#62919 = EDGE_LOOP ( 'NONE', ( #99972, #98419, #28982, #70049 ) ) ;
#62920 = VECTOR ( 'NONE', #84996, 1000.000000000000000 ) ;
#62921 = CARTESIAN_POINT ( 'NONE',  ( -16.54958403137900191, 11.88860064210666856, 11.49999999999998934 ) ) ;
#62922 = ORIENTED_EDGE ( 'NONE', *, *, #88205, .F. ) ;
#62923 = CARTESIAN_POINT ( 'NONE',  ( -5.582908757718670678, 22.30220962497079285, 11.49999999999998934 ) ) ;
#62924 = DIRECTION ( 'NONE',  ( -4.335561085774420994E-16, -0.000000000000000000, 1.000000000000000000 ) ) ;
#62925 = FACE_OUTER_BOUND ( 'NONE', #11620, .T. ) ;
#62926 = ORIENTED_EDGE ( 'NONE', *, *, #78757, .T. ) ;
#62927 = B_SPLINE_CURVE_WITH_KNOTS ( 'NONE', 3,
 ( #40177, #72638, #33565, #40681, #56919, #24939, #10225, #79224, #94458, #33067, #80741, #71128, #1624, #39665 ),
 .UNSPECIFIED., .F., .F.,
 ( 4, 2, 2, 2, 2, 2, 4 ),
 ( 0.000000000000000000, 0.0001567136917012794807, 0.0003134273834025589614, 0.0004701410751038384420, 0.0006268547668051179227, 0.0009402821502076935808, 0.001253709533610269239 ),
 .UNSPECIFIED. ) ;
#62928 = CARTESIAN_POINT ( 'NONE',  ( -97.52287095715003318, -24.66019654487200441, 8.947790411086119278 ) ) ;
#62929 = LINE ( 'NONE', #80133, #48062 ) ;
#62930 = VECTOR ( 'NONE', #56405, 1000.000000000000000 ) ;
#62932 = ORIENTED_EDGE ( 'NONE', *, *, #13604, .F. ) ;
#62931 = CARTESIAN_POINT ( 'NONE',  ( 11.00477826368897283, 18.22718707545001138, 11.49999999999999645 ) ) ;
#62933 = EDGE_LOOP ( 'NONE', ( #83345, #3442, #92126, #11106 ) ) ;
#62934 = CARTESIAN_POINT ( 'NONE',  ( -17.05807961832342912, 14.25954964135033265, -1.500000000000002220 ) ) ;
#62935 = CARTESIAN_POINT ( 'NONE',  ( -6.358105417860958397, -19.66046682221446318, 11.49999999999998934 ) ) ;
#62936 = VERTEX_POINT ( 'NONE', #39115 ) ;
#62937 = FACE_OUTER_BOUND ( 'NONE', #43844, .T. ) ;
#62938 = CARTESIAN_POINT ( 'NONE',  ( -69.85508590344461766, -25.32724624944561853, 4.398071659717722959 ) ) ;
#62939 = ORIENTED_EDGE ( 'NONE', *, *, #39135, .F. ) ;
#62940 = DIRECTION ( 'NONE',  ( -3.773278334453079618E-23, 0.9999999999976377785, 2.173523156925979975E-06 ) ) ;
#62941 = ORIENTED_EDGE ( 'NONE', *, *, #6288, .T. ) ;
#62942 = CARTESIAN_POINT ( 'NONE',  ( 8.971512145086499856, -1.028487854913501032, 5.500000000000000000 ) ) ;
#62943 = CARTESIAN_POINT ( 'NONE',  ( 10.86264264036872440, 0.3587747205144257157, -28.05717073575603138 ) ) ;
#62944 = CARTESIAN_POINT ( 'NONE',  ( -17.86878485216894319, -10.78119150571587781, -1.500000000000002220 ) ) ;
#62945 = CARTESIAN_POINT ( 'NONE',  ( 17.39636294008568740, -13.23181597624684791, 11.49999999999999645 ) ) ;
#62946 = CARTESIAN_POINT ( 'NONE',  ( -102.6228709571500417, -23.73934037231757443, 11.05740245334328087 ) ) ;
#62947 = CARTESIAN_POINT ( 'NONE',  ( -78.55425796183220655, -23.96169478059713498, 10.65365249895717881 ) ) ;
#62948 = CARTESIAN_POINT ( 'NONE',  ( 8.471766090126642723, -20.80389698432254519, 11.49999999999998934 ) ) ;
#62949 = CARTESIAN_POINT ( 'NONE',  ( -118.6289526454650058, -23.48786465467241769, 11.44779295918253581 ) ) ;
#62950 = CARTESIAN_POINT ( 'NONE',  ( -71.70841769935766763, -25.25720466352798255, 6.192981421160952848 ) ) ;
#62951 = CARTESIAN_POINT ( 'NONE',  ( -31.58953762381672092, -24.64965694238574656, 8.947790433994208925 ) ) ;
#62952 = VERTEX_POINT ( 'NONE', #9168 ) ;
#62953 = B_SPLINE_SURFACE_WITH_KNOTS ( 'NONE', 3, 1, ( 
 ( #10430, #12428 ),
 ( #41391, #43396 ),
 ( #96668, #72847 ),
 ( #66248, #34284 ),
 ( #19042, #80951 ),
 ( #81456, #42413 ),
 ( #80448, #95675 ),
 ( #20045, #66749 ),
 ( #4333, #4825 ),
 ( #35778, #27667 ),
 ( #50016, #18545 ) ),
 .UNSPECIFIED., .F., .F., .F.,
 ( 4, 1, 1, 1, 1, 1, 1, 1, 4 ),
 ( 2, 2 ),
 ( 0.000000000000000000, 0.1022030370352139811, 0.2110233423738757941, 0.3250996615652070321, 0.4465020971348850898, 0.5737877176488546116, 0.7089007097660665613, 0.8503578712933955730, 1.000000000000000000 ),
 ( 0.000000000000000000, 1.000000000000000000 ),
 .UNSPECIFIED. ) ;
#62954 = EDGE_LOOP ( 'NONE', ( #32697, #68774, #11018, #37145 ) ) ;
#62955 = ORIENTED_EDGE ( 'NONE', *, *, #48299, .T. ) ;
#62956 = ORIENTED_EDGE ( 'NONE', *, *, #43262, .T. ) ;
#62957 = CARTESIAN_POINT ( 'NONE',  ( -8.434714792116727367, -19.68496499552307455, -1.500000000000002220 ) ) ;
#62958 = CARTESIAN_POINT ( 'NONE',  ( 15.34105849444754455, 16.31744944422920440, 11.49999999999999645 ) ) ;
#62959 = EDGE_LOOP ( 'NONE', ( #92219, #88055, #85504, #15596 ) ) ;
#62960 = CARTESIAN_POINT ( 'NONE',  ( -5.931750313267273533, -20.21149935180699231, 11.49999999999998934 ) ) ;
#62961 = FACE_OUTER_BOUND ( 'NONE', #23615, .T. ) ;
#62962 = ADVANCED_FACE ( 'NONE', ( #70068 ), #24392, .F. ) ;
#62963 = CARTESIAN_POINT ( 'NONE',  ( 0.05828707793547563409, -19.95834144014285272, -1.500000000000002220 ) ) ;
#62964 = DIRECTION ( 'NONE',  ( -3.773278334444166432E-23, 1.000000000000000000, 0.000000000000000000 ) ) ;
#62965 = CARTESIAN_POINT ( 'NONE',  ( -43.52287095715007581, -24.66019654487199375, 8.947790411086128159 ) ) ;
#62966 = CARTESIAN_POINT ( 'NONE',  ( -16.59477544326466969, -14.39948450415919723, -1.500000000000002220 ) ) ;
#62967 = PLANE ( 'NONE',  #75485 ) ;
#62968 = EDGE_LOOP ( 'NONE', ( #16442, #57561, #49329, #75261 ) ) ;
#62969 = CARTESIAN_POINT ( 'NONE',  ( -15.82668884360736961, -1.684774720514424118, 42.07822029717483758 ) ) ;
#62970 = B_SPLINE_CURVE_WITH_KNOTS ( 'NONE', 3,
 ( #10928, #2829, #49504, #93648, #56120, #64750, #24143, #71836, #41383, #62730, #56623, #16522, #95667, #25138, #31764, #64241 ),
 .UNSPECIFIED., .F., .F.,
 ( 4, 2, 2, 2, 2, 2, 2, 4 ),
 ( 0.000000000000000000, 0.0001831894960030059445, 0.0003663789920060118890, 0.0007327579840120237780, 0.0009159474800150220518, 0.001099136976018020434, 0.001282326472021018708, 0.001465515968024016982 ),
 .UNSPECIFIED. ) ;
#62971 = EDGE_CURVE ( 'NONE', #69183, #72199, #7162, .T. ) ;
#62972 = DIRECTION ( 'NONE',  ( -0.4009304992412300317, -6.845827386180410961E-16, -0.9161084732596779245 ) ) ;
#62973 = CARTESIAN_POINT ( 'NONE',  ( 20.80141654084381386, -1.409215765453083469, 11.49999999999999645 ) ) ;
#62974 = VECTOR ( 'NONE', #53149, 1000.000000000000000 ) ;
#62975 = EDGE_CURVE ( 'NONE', #62904, #6142, #17036, .T. ) ;
#62976 = CARTESIAN_POINT ( 'NONE',  ( 31.63505726983280297, -3.634951944882593988, 27.30823744647568674 ) ) ;
#62977 = EDGE_CURVE ( 'NONE', #78888, #25133, #25486, .T. ) ;
#62978 = CARTESIAN_POINT ( 'NONE',  ( -108.6228709571501128, -24.35013146730204525, 9.818937971375106599 ) ) ;
#62979 = CARTESIAN_POINT ( 'NONE',  ( -90.62287095715004170, -25.00158670708908915, 2.256160236439166411 ) ) ;
#62980 = CARTESIAN_POINT ( 'NONE',  ( 3.065528897535349628, -21.08962430476942274, 11.49999999999998934 ) ) ;
#62981 = CARTESIAN_POINT ( 'NONE',  ( -46.62287095715004881, -23.48786465467241058, 11.44779295918255180 ) ) ;
#62982 = EDGE_CURVE ( 'NONE', #84523, #88166, #67925, .T. ) ;
#62983 = CARTESIAN_POINT ( 'NONE',  ( -66.52287095715006160, -23.47596703998600631, 11.44779298504228748 ) ) ;
#62984 = CARTESIAN_POINT ( 'NONE',  ( -64.62738566448841482, -24.51419770103159124, 9.386484678747168076 ) ) ;
#62985 = CARTESIAN_POINT ( 'NONE',  ( -5.576923076923076650, -5.876774720514418071, 20.44941907051282470 ) ) ;
#62986 = CARTESIAN_POINT ( 'NONE',  ( 6.936750662203477802, 21.44973376661030429, -1.500000000000002220 ) ) ;
#62987 = CARTESIAN_POINT ( 'NONE',  ( 0.6000000000000007550, 0.000000000000000000, 0.000000000000000000 ) ) ;
#62988 = ORIENTED_EDGE ( 'NONE', *, *, #77021, .F. ) ;
#62989 = CARTESIAN_POINT ( 'NONE',  ( -35.62287095715005592, -25.00158670708908915, 2.256160236439166855 ) ) ;
#62990 = CARTESIAN_POINT ( 'NONE',  ( -31.60165186599006049, -23.96169478059712432, 10.65365249895719124 ) ) ;
#62991 = CARTESIAN_POINT ( 'NONE',  ( 8.085132396474181249, 17.94908993440701295, 11.49999999999999645 ) ) ;
#62992 = FACE_OUTER_BOUND ( 'NONE', #95621, .T. ) ;
#62993 = VECTOR ( 'NONE', #25186, 1000.000000000000000 ) ;
#62994 = LINE ( 'NONE', #47758, #56115 ) ;
#62995 = EDGE_CURVE ( 'NONE', #13572, #89454, #17791, .T. ) ;
#62996 = ORIENTED_EDGE ( 'NONE', *, *, #77588, .T. ) ;
#62997 = CARTESIAN_POINT ( 'NONE',  ( -90.52287095715003318, -25.00182538069145366, 7.747789668545104647 ) ) ;
#62998 = DIRECTION ( 'NONE',  ( -0.000000000000000000, 1.000000000000000000, -0.000000000000000000 ) ) ;
#62999 = CARTESIAN_POINT ( 'NONE',  ( 8.160000000000000142, 0.1579206558577706254, 7.788828319098143105 ) ) ;
#63000 = CARTESIAN_POINT ( 'NONE',  ( -68.58953762381672448, -24.64965694238406968, 8.947790433994660120 ) ) ;
#63001 = CARTESIAN_POINT ( 'NONE',  ( 15.11087362536062173, -12.71848776332401521, 11.49999999999998934 ) ) ;
#63002 = CIRCLE ( 'NONE', #50034, 2.039999999999998703 ) ;
#63003 = ORIENTED_EDGE ( 'NONE', *, *, #94937, .T. ) ;
#63004 = CARTESIAN_POINT ( 'NONE',  ( -16.64171244834553676, 11.49637152377623828, 11.49999999999999645 ) ) ;
#63005 = CARTESIAN_POINT ( 'NONE',  ( 9.818046095193736278, 3.316774720514088504, -28.04791984001701621 ) ) ;
#63006 = APPROVAL_ROLE ( '' ) ;
#63007 = ORIENTED_EDGE ( 'NONE', *, *, #92731, .F. ) ;
#63008 = CARTESIAN_POINT ( 'NONE',  ( -53.62287095715004170, -24.50216790748098461, 0.6166512839513605959 ) ) ;
#63009 = CARTESIAN_POINT ( 'NONE',  ( 1.351731822651893733, -3.882286141751412067, -8.999999999999998224 ) ) ;
#63010 = CARTESIAN_POINT ( 'NONE',  ( -51.04919692492541117, -25.30031294595708857, 5.371548930483984741 ) ) ;
#63011 = CARTESIAN_POINT ( 'NONE',  ( -67.62287095715004170, -24.50216790748098816, 0.6166512839513741406 ) ) ;
#63012 = CARTESIAN_POINT ( 'NONE',  ( 3.252401863874215593, 0.3587747205143964613, -29.35688408629929214 ) ) ;
#63013 = FACE_OUTER_BOUND ( 'NONE', #6758, .T. ) ;
#63014 = CARTESIAN_POINT ( 'NONE',  ( -14.99618758923778117, -13.25627519679515665, -1.500000000000002220 ) ) ;
#63015 = ADVANCED_FACE ( 'NONE', ( #64496 ), #1574, .T. ) ;
#63016 = CARTESIAN_POINT ( 'NONE',  ( -58.62287095715002039, -24.33832256526968862, 0.1851278514119840124 ) ) ;
#63017 = CARTESIAN_POINT ( 'NONE',  ( -5.023036858974361252, -5.876774720514410077, 19.14743589743590846 ) ) ;
#63018 = EDGE_LOOP ( 'NONE', ( #54920, #44630, #7884, #40718 ) ) ;
#63019 = EDGE_CURVE ( 'NONE', #33587, #58273, #40050, .T. ) ;
#63020 = CARTESIAN_POINT ( 'NONE',  ( -79.59200941457424960, -24.15620529776628089, 10.23563542870660470 ) ) ;
#63021 = CARTESIAN_POINT ( 'NONE',  ( -109.3750630267952317, -25.29012884606049383, 4.026263179138138248 ) ) ;
#63022 = CARTESIAN_POINT ( 'NONE',  ( -89.62287095715004170, -24.64898659630529210, 1.056161002820827921 ) ) ;
#63023 = LINE ( 'NONE', #55912, #93763 ) ;
#63024 = CARTESIAN_POINT ( 'NONE',  ( -118.1692003789631684, -25.31326721218303888, 3.500953664922430431 ) ) ;
#63025 = CARTESIAN_POINT ( 'NONE',  ( -83.62626469299168264, -24.51314013834315020, 0.6176544820404096248 ) ) ;
#63026 = CARTESIAN_POINT ( 'NONE',  ( -3.085512303079157359, -5.876774720514415407, 19.95084900476495093 ) ) ;
#63027 = ADVANCED_FACE ( 'NONE', ( #42147 ), #3576, .T. ) ;
#63028 = CARTESIAN_POINT ( 'NONE',  ( -101.9689938327708774, -25.25978491487772004, 3.590542621692357717 ) ) ;
#63029 = EDGE_LOOP ( 'NONE', ( #23786, #63838, #3068, #49717 ) ) ;
#63030 = AXIS2_PLACEMENT_3D ( 'NONE', #95337, #21684, #67896 ) ;
#63031 = AXIS2_PLACEMENT_3D ( 'NONE', #82172, #28379, #12154 ) ;
#63032 = CARTESIAN_POINT ( 'NONE',  ( -3.904290608643684379, -19.93223805144805283, -1.500000000000002220 ) ) ;
#63033 = EDGE_CURVE ( 'NONE', #49913, #27337, #32511, .T. ) ;
#63034 = VECTOR ( 'NONE', #42971, 1000.000000000000000 ) ;
#63035 = CARTESIAN_POINT ( 'NONE',  ( -59.64293371994119752, -23.96169478059713143, 10.65365249895718769 ) ) ;
#63036 = EDGE_LOOP ( 'NONE', ( #48615, #87467, #21589, #75750 ) ) ;
#63037 = CARTESIAN_POINT ( 'NONE',  ( -94.52287095715006160, -23.47596703998600631, 11.44779298504228393 ) ) ;
#63038 = CARTESIAN_POINT ( 'NONE',  ( -19.70923665959843873, 4.302044407003456250, -1.500000000000002220 ) ) ;
#63039 = CARTESIAN_POINT ( 'NONE',  ( -20.67868931609407213, -4.308284118179648736, 11.49999999999999645 ) ) ;
#63040 = AXIS2_PLACEMENT_3D ( 'NONE', #76818, #85441, #85952 ) ;
#63041 = CARTESIAN_POINT ( 'NONE',  ( 21.58644828898399481, -4.983269013152989757, -1.500000000000002220 ) ) ;
#63043 = CARTESIAN_POINT ( 'NONE',  ( -12.99546161633903552, -15.93940442571882876, 11.49999999999998934 ) ) ;
#63042 = PRODUCT_RELATED_PRODUCT_CATEGORY ( 'detail', '', ( #71682 ) ) ;
#63044 = CARTESIAN_POINT ( 'NONE',  ( -55.52287095715008292, -23.47593901973090169, -1.443836447538997092 ) ) ;
#63045 = ORIENTED_EDGE ( 'NONE', *, *, #86469, .T. ) ;
#63046 = LINE ( 'NONE', #40193, #76587 ) ;
#63047 = ORIENTED_EDGE ( 'NONE', *, *, #93631, .F. ) ;
#63048 = LINE ( 'NONE', #40195, #39726 ) ;
#63049 = PLANE ( 'NONE',  #3224 ) ;
#63050 = EDGE_LOOP ( 'NONE', ( #21127, #33444, #22852, #98952 ) ) ;
#63051 = ORIENTED_EDGE ( 'NONE', *, *, #11070, .F. ) ;
#63052 = VECTOR ( 'NONE', #51412, 1000.000000000000114 ) ;
#63053 = ORIENTED_EDGE ( 'NONE', *, *, #81947, .T. ) ;
#63054 = PLANE ( 'NONE',  #16215 ) ;
#63055 = CARTESIAN_POINT ( 'NONE',  ( -55.52287095715005449, -24.99156044556119483, 7.747789690856173195 ) ) ;
#63056 = CARTESIAN_POINT ( 'NONE',  ( -68.59719453268294842, -23.96169478059712787, 10.65365249895718414 ) ) ;
#63057 = CARTESIAN_POINT ( 'NONE',  ( 20.35908867758196550, 3.722869731652943770, -1.500000000000002220 ) ) ;
#63058 = CARTESIAN_POINT ( 'NONE',  ( 12.90450488963236353, -17.39418326053592168, 11.49999999999999645 ) ) ;
#63059 = VERTEX_POINT ( 'NONE', #48754 ) ;
#63060 = DIRECTION ( 'NONE',  ( -1.000000000000000000, 0.000000000000000000, -0.000000000000000000 ) ) ;
#63061 = CARTESIAN_POINT ( 'NONE',  ( -55.52287095715006870, -29.50247984919015209, -1.443849546365056913 ) ) ;
#63062 = CARTESIAN_POINT ( 'NONE',  ( -9.622923231576368863, -20.19340101508991125, -1.500000000000002220 ) ) ;
#63063 = CARTESIAN_POINT ( 'NONE',  ( -47.50043236403589475, -24.15620529776627379, 10.23563542870660825 ) ) ;
#63064 = CARTESIAN_POINT ( 'NONE',  ( -84.50114960218334659, -24.65952944569303895, 1.056160979905700348 ) ) ;
#63065 = EDGE_LOOP ( 'NONE', ( #84312, #59476 ) ) ;
#63066 = CARTESIAN_POINT ( 'NONE',  ( -100.6814946224345846, -25.31267346029541443, 4.736250531364077254 ) ) ;
#63067 = CARTESIAN_POINT ( 'NONE',  ( -52.58953762381673158, -24.64965694238406968, 8.947790433994663672 ) ) ;
#63068 = EDGE_LOOP ( 'NONE', ( #31577, #7413, #24750, #24472 ) ) ;
#63069 = CARTESIAN_POINT ( 'NONE',  ( -39.62287095715005592, -24.66019654487199020, 8.947790411086135265 ) ) ;
#63070 = VERTEX_POINT ( 'NONE', #63486 ) ;
#63071 = VECTOR ( 'NONE', #18056, 1000.000000000000114 ) ;
#63072 = PLANE ( 'NONE',  #11436 ) ;
#63073 = CARTESIAN_POINT ( 'NONE',  ( -19.86647519178106691, -7.318714840676754818, -1.500000000000002220 ) ) ;
#63074 = VERTEX_POINT ( 'NONE', #25899 ) ;
#63075 = CARTESIAN_POINT ( 'NONE',  ( -50.53277973184150795, -24.73486907724918282, 1.287355809206963464 ) ) ;
#63076 = CARTESIAN_POINT ( 'NONE',  ( 11.26692973276593968, -18.67385317477220497, -1.500000000000002220 ) ) ;
#63077 = FACE_OUTER_BOUND ( 'NONE', #65161, .T. ) ;
#63078 = DIRECTION ( 'NONE',  ( 0.000000000000000000, 0.9999999999976377785, 2.173523156925979128E-06 ) ) ;
#63079 = PLANE ( 'NONE',  #4428 ) ;
#63080 = CARTESIAN_POINT ( 'NONE',  ( -8.334044162642690878, 20.12857247364870616, -1.500000000000002220 ) ) ;
#63081 = CARTESIAN_POINT ( 'NONE',  ( -67.52287095715003318, -23.47593901973090169, -1.443836447538996870 ) ) ;
#63082 = EDGE_CURVE ( 'NONE', #75990, #57717, #57871, .T. ) ;
#63083 = VERTEX_POINT ( 'NONE', #34017 ) ;
#63084 = PLANE ( 'NONE',  #30789 ) ;
#63085 = CARTESIAN_POINT ( 'NONE',  ( -19.80875734969026425, -0.3587747205144265483, 31.02402280011862246 ) ) ;
#63086 = VERTEX_POINT ( 'NONE', #2572 ) ;
#63087 = DIRECTION ( 'NONE',  ( 1.000000000000000000, 3.773278334444166432E-23, 8.201307841325785021E-29 ) ) ;
#63088 = VERTEX_POINT ( 'NONE', #40633 ) ;
#63089 = VERTEX_POINT ( 'NONE', #94406 ) ;
#63090 = EDGE_CURVE ( 'NONE', #10228, #41756, #20632, .T. ) ;
#63091 = DIRECTION ( 'NONE',  ( 0.000000000000000000, 0.9999999999976377785, 2.173523156925979975E-06 ) ) ;
#63092 = CARTESIAN_POINT ( 'NONE',  ( -82.51328383053662208, -23.96119346886881019, -0.6495511937831923710 ) ) ;
#63093 = CARTESIAN_POINT ( 'NONE',  ( 7.950249384483326409, 19.69624408967213469, 11.49999999999998934 ) ) ;
#63094 = CARTESIAN_POINT ( 'NONE',  ( -94.55207186148825826, -24.15543982623907482, -0.2315651400026595141 ) ) ;
#63095 = EDGE_CURVE ( 'NONE', #67184, #32503, #79937, .T. ) ;
#63096 = CARTESIAN_POINT ( 'NONE',  ( -69.62287095715005592, -24.66019654487199020, 8.947790411086131712 ) ) ;
#63097 = DIRECTION ( 'NONE',  ( -1.000000000000000000, -3.773278334444166432E-23, -8.201307841325785021E-29 ) ) ;
#63098 = DIRECTION ( 'NONE',  ( 0.000000000000000000, 0.000000000000000000, 1.000000000000000000 ) ) ;
#63099 = CARTESIAN_POINT ( 'NONE',  ( 18.72033823704212097, 5.060218808788302880, 11.49999999999998934 ) ) ;
#63100 = DIRECTION ( 'NONE',  ( -0.000000000000000000, 1.000000000000000000, -0.000000000000000000 ) ) ;
#63101 = ORIENTED_EDGE ( 'NONE', *, *, #97357, .T. ) ;
#63102 = CARTESIAN_POINT ( 'NONE',  ( -15.27948257512286645, 12.15582775940324822, 11.49999999999999645 ) ) ;
#63103 = CARTESIAN_POINT ( 'NONE',  ( -91.52287095715006160, -24.65952944569304606, 1.056160979905700570 ) ) ;
#63104 = VECTOR ( 'NONE', #8044, 1000.000000000000000 ) ;
#63105 = CARTESIAN_POINT ( 'NONE',  ( -41.32836283488544638, 2.682774720514426559, 39.26872235229541985 ) ) ;
#63106 = EDGE_CURVE ( 'NONE', #22592, #5790, #81212, .T. ) ;
#63107 = EDGE_LOOP ( 'NONE', ( #86435, #2838, #25219, #11343 ) ) ;
#63108 = CARTESIAN_POINT ( 'NONE',  ( 4.959846025536391423, -6.376774720514417183, 20.32314756232572250 ) ) ;
#63109 = CARTESIAN_POINT ( 'NONE',  ( -89.59823067049254064, -23.73766607897671221, -1.055555164236434029 ) ) ;
#63110 = AXIS2_PLACEMENT_3D ( 'NONE', #22842, #30478, #46715 ) ;
#63111 = B_SPLINE_CURVE_WITH_KNOTS ( 'NONE', 3,
 ( #39706, #71173, #94501, #93994 ),
 .UNSPECIFIED., .F., .F.,
 ( 4, 4 ),
 ( 0.000000000000000000, 9.999999999997510880E-05 ),
 .UNSPECIFIED. ) ;
#63112 = DIRECTION ( 'NONE',  ( 0.000000000000000000, 0.000000000000000000, -1.000000000000000000 ) ) ;
#63113 = FACE_OUTER_BOUND ( 'NONE', #69645, .T. ) ;
#63114 = CARTESIAN_POINT ( 'NONE',  ( -17.62174901100306101, -8.731699659924187173, -1.500000000000002220 ) ) ;
#63115 = CIRCLE ( 'NONE', #12891, 130.2784398600581710 ) ;
#63116 = ORIENTED_EDGE ( 'NONE', *, *, #30239, .T. ) ;
#63117 = CARTESIAN_POINT ( 'NONE',  ( -20.99440926880444636, 4.982473936180791263, 11.49999999999998934 ) ) ;
#63118 = VECTOR ( 'NONE', #82609, 1000.000000000000000 ) ;
#63119 = DIRECTION ( 'NONE',  ( -0.000000000000000000, 2.173523156925979552E-06, -0.9999999999976378895 ) ) ;
#63120 = DIRECTION ( 'NONE',  ( -0.9890158633619158257, -0.1478094111296165414, -0.000000000000000000 ) ) ;
#63121 = CARTESIAN_POINT ( 'NONE',  ( 13.31140876108729998, -18.89465134148960956, -1.500000000000002220 ) ) ;
#63122 = PERSON_AND_ORGANIZATION ( #70597, #27821 ) ;
#63123 = CARTESIAN_POINT ( 'NONE',  ( 3.165726958143470160, -5.876774720514421624, 21.14296526391294506 ) ) ;
#63124 = CARTESIAN_POINT ( 'NONE',  ( 4.281508569253434260, -6.376774720514422512, 21.28700241941785265 ) ) ;
#63125 = CARTESIAN_POINT ( 'NONE',  ( 6.727764423076923350, -6.376774720514413630, 19.76442307692307665 ) ) ;
#63126 = DIRECTION ( 'NONE',  ( 1.000000000000000000, 0.000000000000000000, 0.000000000000000000 ) ) ;
#63127 = CARTESIAN_POINT ( 'NONE',  ( -111.0058427071010527, -25.29823846644867658, 2.995660944314382679 ) ) ;
#63128 = CARTESIAN_POINT ( 'NONE',  ( -129.6234738294825206, -24.65952944569305316, 1.056160979905705677 ) ) ;
#63129 = CARTESIAN_POINT ( 'NONE',  ( -99.15308351095438866, -25.26400742361759555, 4.278189958765021395 ) ) ;
#63130 = CARTESIAN_POINT ( 'NONE',  ( -17.57349146297605103, 9.389787994052484876, -1.500000000000002220 ) ) ;
#63131 = CARTESIAN_POINT ( 'NONE',  ( -75.59706082321993392, -24.15602025860895807, 10.28564288303536678 ) ) ;
#63132 = CARTESIAN_POINT ( 'NONE',  ( -19.37706247964952411, -4.161318200553020041, -1.500000000000002220 ) ) ;
#63133 = ORIENTED_EDGE ( 'NONE', *, *, #29498, .T. ) ;
#63134 = CARTESIAN_POINT ( 'NONE',  ( -56.55353067738275286, -23.96119346886880663, -0.6495511937832126881 ) ) ;
#63135 = EDGE_CURVE ( 'NONE', #48998, #21576, #71510, .T. ) ;
#63136 = CARTESIAN_POINT ( 'NONE',  ( -39.08546997848264226, -25.10925814828167546, 3.855771613512330109 ) ) ;
#63137 = DIRECTION ( 'NONE',  ( 0.000000000000000000, 0.9999999999976377785, 2.173523156925979128E-06 ) ) ;
#63138 = CARTESIAN_POINT ( 'NONE',  ( 14.61947915221463923, 14.71393552341326760, 11.49999999999999645 ) ) ;
#63139 = CARTESIAN_POINT ( 'NONE',  ( -83.62287095715005592, -29.50250243563736774, 8.947779886222141599 ) ) ;
#63140 = EDGE_CURVE ( 'NONE', #62812, #82726, #40127, .T. ) ;
#63141 = CARTESIAN_POINT ( 'NONE',  ( -38.62287095715005592, -24.64898659630528144, 1.056161002820819261 ) ) ;
#63142 = CARTESIAN_POINT ( 'NONE',  ( -4.239441843796335263, -22.36999388947090139, 11.49999999999999645 ) ) ;
#63143 = B_SPLINE_CURVE_WITH_KNOTS ( 'NONE', 3,
 ( #51721, #74554, #4558, #35504, #89784, #67450, #81168, #83154, #66962, #42625, #97875, #66480 ),
 .UNSPECIFIED., .F., .F.,
 ( 4, 2, 2, 2, 2, 4 ),
 ( 0.000000000000000000, 0.0003156378818151490723, 0.0006312757636302981446, 0.0009469136454454471627, 0.001104732586353022322, 0.001262551527260597373 ),
 .UNSPECIFIED. ) ;
#63144 = ORIENTED_EDGE ( 'NONE', *, *, #5567, .F. ) ;
#63145 = PLANE ( 'NONE',  #78634 ) ;
#63146 = LINE ( 'NONE', #94071, #72751 ) ;
#63147 = ORIENTED_EDGE ( 'NONE', *, *, #51290, .T. ) ;
#63148 = CARTESIAN_POINT ( 'NONE',  ( 19.32837167043147986, -5.866312143582237404, -1.500000000000002220 ) ) ;
#63149 = CARTESIAN_POINT ( 'NONE',  ( -29.49875734969025842, 0.3587747205144265483, 17.86602280011862476 ) ) ;
#63150 = CARTESIAN_POINT ( 'NONE',  ( -29.49875734969026198, -0.3587747205144262708, 7.870022800118625206 ) ) ;
#63151 = VERTEX_POINT ( 'NONE', #56373 ) ;
#63152 = CARTESIAN_POINT ( 'NONE',  ( -40.55620429048340014, -23.48786465467240347, 11.44779295918255180 ) ) ;
#63153 = CARTESIAN_POINT ( 'NONE',  ( -20.38739128398232836, 10.50225141308550292, 11.49999999999998934 ) ) ;
#63154 = CARTESIAN_POINT ( 'NONE',  ( -50.40445135320379677, -25.18439649812517089, 3.293943117865877124 ) ) ;
#63155 = CARTESIAN_POINT ( 'NONE',  ( -16.84340083857899018, -10.81494551495373457, -1.500000000000002220 ) ) ;
#63156 = CARTESIAN_POINT ( 'NONE',  ( -71.52287095715010423, -24.66019654487200086, 8.947790411086115725 ) ) ;
#63157 = CARTESIAN_POINT ( 'NONE',  ( 20.71091302404612833, 3.140364381853995912, 11.49999999999999645 ) ) ;
#63158 = CARTESIAN_POINT ( 'NONE',  ( -4.141025641025642301, -5.876774720514412742, 19.63681891025641235 ) ) ;
#63159 = CARTESIAN_POINT ( 'NONE',  ( -68.96115101070704156, -25.31612651568953254, 5.914983513647228186 ) ) ;
#63160 = CARTESIAN_POINT ( 'NONE',  ( -21.92701646642465008, -2.088449908657787457, -1.500000000000002220 ) ) ;
#63161 = VECTOR ( 'NONE', #87176, 1000.000000000000000 ) ;
#63162 = EDGE_CURVE ( 'NONE', #35655, #13725, #4533, .T. ) ;
#63163 = EDGE_CURVE ( 'NONE', #32836, #25405, #60368, .T. ) ;
#63164 = CARTESIAN_POINT ( 'NONE',  ( -127.4728709548940486, -25.21112548385454843, 2.000950964958115197 ) ) ;
#63165 = VERTEX_POINT ( 'NONE', #36004 ) ;
#63166 = CARTESIAN_POINT ( 'NONE',  ( -49.54012794836013001, -25.27344868860170379, 3.796733121357704022 ) ) ;
#63167 = DIRECTION ( 'NONE',  ( -0.000000000000000000, 1.000000000000000000, -0.000000000000000000 ) ) ;
#63168 = ORIENTED_EDGE ( 'NONE', *, *, #84588, .F. ) ;
#63169 = FACE_OUTER_BOUND ( 'NONE', #34714, .T. ) ;
#63170 = ORIENTED_EDGE ( 'NONE', *, *, #40223, .T. ) ;
#63171 = VERTEX_POINT ( 'NONE', #89798 ) ;
#63172 = CARTESIAN_POINT ( 'NONE',  ( 23.91005183030481263, -2.682774720514426559, -14.40591128290692069 ) ) ;
#63173 = CARTESIAN_POINT ( 'NONE',  ( -100.6747599127204040, -25.10935806245408841, 2.849795651036889588 ) ) ;
#63174 = CARTESIAN_POINT ( 'NONE',  ( -36.58086577407884477, -24.51314013834316086, 0.6176544820404111791 ) ) ;
#63175 = CARTESIAN_POINT ( 'NONE',  ( -9.379331868514380943, 18.20734191464070406, -1.500000000000002220 ) ) ;
#63176 = VERTEX_POINT ( 'NONE', #35015 ) ;
#63177 = CARTESIAN_POINT ( 'NONE',  ( 282.9764569301858046, -5.965225279485572685, 20.79159422840526616 ) ) ;
#63178 = ADVANCED_FACE ( 'NONE', ( #97891 ), #28387, .F. ) ;
#63179 = AXIS2_PLACEMENT_3D ( 'NONE', #16888, #38223, #47849 ) ;
#63180 = CARTESIAN_POINT ( 'NONE',  ( -44.54662673226112446, -24.15543982623906771, -0.2315651400026670914 ) ) ;
#63181 = CARTESIAN_POINT ( 'NONE',  ( -54.62287095715004881, -23.48783264082478084, -1.443836473390070596 ) ) ;
#63182 = CARTESIAN_POINT ( 'NONE',  ( -21.75032768068154354, -4.810781854073628239, 11.49999999999998934 ) ) ;
#63183 = CARTESIAN_POINT ( 'NONE',  ( -101.5895376238167245, -24.64965694238407679, 8.947790433994649462 ) ) ;
#63184 = CARTESIAN_POINT ( 'NONE',  ( -81.52287095715006160, -29.50248528299804818, 1.056150453629038477 ) ) ;
#63185 = ORIENTED_EDGE ( 'NONE', *, *, #13007, .T. ) ;
#63186 = B_SPLINE_CURVE_WITH_KNOTS ( 'NONE', 3,
 ( #84791, #28511, #67592, #15275 ),
 .UNSPECIFIED., .F., .F.,
 ( 4, 4 ),
 ( 0.000000000000000000, 0.0001002978966067895783 ),
 .UNSPECIFIED. ) ;
#63187 = DIRECTION ( 'NONE',  ( -3.773278334453079618E-23, 0.9999999999976377785, 2.173523156925979975E-06 ) ) ;
#63188 = VECTOR ( 'NONE', #93464, 1000.000000000000114 ) ;
#63189 = DIRECTION ( 'NONE',  ( 0.000000000000000000, 2.173523156925980399E-06, -0.9999999999976378895 ) ) ;
#63190 = AXIS2_PLACEMENT_3D ( 'NONE', #49942, #2258, #42332 ) ;
#63191 = CARTESIAN_POINT ( 'NONE',  ( -19.40898059523135544, 7.551958013340856368, 11.49999999999998934 ) ) ;
#63192 = ORIENTED_EDGE ( 'NONE', *, *, #21717, .F. ) ;
#63194 = ORIENTED_EDGE ( 'NONE', *, *, #52191, .T. ) ;
#63193 = CARTESIAN_POINT ( 'NONE',  ( 9.278253834636473130, -6.376774720514426953, 18.21871304725684482 ) ) ;
#63195 = VERTEX_POINT ( 'NONE', #12663 ) ;
#63196 = AXIS2_PLACEMENT_3D ( 'NONE', #62854, #31882, #24263 ) ;
#63197 = CARTESIAN_POINT ( 'NONE',  ( -51.52589570729855950, -25.12217672741640584, 6.227984225844234167 ) ) ;
#63198 = CARTESIAN_POINT ( 'NONE',  ( -16.09219062524700661, 13.46031615953476468, -1.500000000000002220 ) ) ;
#63199 = ORIENTED_EDGE ( 'NONE', *, *, #71911, .T. ) ;
#63200 = CARTESIAN_POINT ( 'NONE',  ( -93.62287095715002749, -24.51387760970724727, 9.387446482453412955 ) ) ;
#63201 = DIRECTION ( 'NONE',  ( 0.000000000000000000, 0.000000000000000000, 1.000000000000000000 ) ) ;
#63202 = CARTESIAN_POINT ( 'NONE',  ( 10.73283225838973642, -5.356774720506346732, -27.03068772369604744 ) ) ;
#63203 = CARTESIAN_POINT ( 'NONE',  ( -86.59885718012090194, -23.73791477778911840, 11.05961554403170766 ) ) ;
#63204 = CARTESIAN_POINT ( 'NONE',  ( -60.62287095715006302, -24.91570333823099404, 8.075032458375554612 ) ) ;
#63205 = DIRECTION ( 'NONE',  ( 1.000000000000000000, -7.960204194457801640E-17, 0.000000000000000000 ) ) ;
#63206 = EDGE_CURVE ( 'NONE', #14471, #47759, #49781, .T. ) ;
#63208 = VERTEX_POINT ( 'NONE', #82676 ) ;
#63207 = CARTESIAN_POINT ( 'NONE',  ( 19.86420646539740176, -9.926203236129387264, 11.49999999999999645 ) ) ;
#63209 = CARTESIAN_POINT ( 'NONE',  ( -109.2228709571500644, -23.47593901973090524, -1.443836447538996648 ) ) ;
#63210 = CARTESIAN_POINT ( 'NONE',  ( -37.58953762381672448, -23.48786465467240347, 11.44779295918255180 ) ) ;
#63211 = EDGE_LOOP ( 'NONE', ( #96918, #95948, #99209, #430 ) ) ;
#63212 = CARTESIAN_POINT ( 'NONE',  ( -14.80616194778269623, -17.16973004002414882, -1.500000000000002220 ) ) ;
#63214 = EDGE_LOOP ( 'NONE', ( #86301, #94875, #15980, #43963 ) ) ;
#63213 = CARTESIAN_POINT ( 'NONE',  ( -5.891025641025639636, -6.376774720514420736, 20.75510817307693046 ) ) ;
#63215 = EDGE_LOOP ( 'NONE', ( #42970, #31099, #51835, #64970 ) ) ;
#63216 = PLANE ( 'NONE',  #36796 ) ;
#63217 = EDGE_CURVE ( 'NONE', #96655, #18999, #97406, .T. ) ;
#63218 = CARTESIAN_POINT ( 'NONE',  ( 2.654622155064554789, -19.98241913370796041, 11.49999999999998934 ) ) ;
#63219 = EDGE_CURVE ( 'NONE', #32487, #96155, #44127, .T. ) ;
#63220 = CARTESIAN_POINT ( 'NONE',  ( -81.62287095715004170, -24.51387760970723662, 9.387446482453421837 ) ) ;
#63221 = ORIENTED_EDGE ( 'NONE', *, *, #36699, .T. ) ;
#63222 = CARTESIAN_POINT ( 'NONE',  ( -39.52287095715006870, -23.48786465467241058, 11.44779295918255180 ) ) ;
#63223 = CARTESIAN_POINT ( 'NONE',  ( -17.59303920844588376, -13.82112144285918731, -1.500000000000002220 ) ) ;
#63224 = EDGE_CURVE ( 'NONE', #19118, #74917, #98390, .T. ) ;
#63225 = ORIENTED_EDGE ( 'NONE', *, *, #77025, .F. ) ;
#63226 = ORIENTED_EDGE ( 'NONE', *, *, #43488, .F. ) ;
#63227 = DIRECTION ( 'NONE',  ( -0.000000000000000000, -1.000000000000000000, -0.000000000000000000 ) ) ;
#63228 = CARTESIAN_POINT ( 'NONE',  ( -94.55206473217479868, -24.15620529776628089, 10.23563542870660470 ) ) ;
#63229 = CARTESIAN_POINT ( 'NONE',  ( -96.55620429048340725, -23.47596703998600631, 11.44779298504227683 ) ) ;
#63230 = DIRECTION ( 'NONE',  ( 0.000000000000000000, -0.000000000000000000, -1.000000000000000000 ) ) ;
#63231 = ADVANCED_FACE ( 'NONE', ( #83168 ), #66979, .F. ) ;
#63232 = DIRECTION ( 'NONE',  ( 0.000000000000000000, 0.000000000000000000, -1.000000000000000000 ) ) ;
#63233 = CARTESIAN_POINT ( 'NONE',  ( 6.425176733589397671, 18.50107501292125178, -1.500000000000002220 ) ) ;
#63234 = CARTESIAN_POINT ( 'NONE',  ( -5.115065434581078208, -5.876774720514409189, 19.15054976246387497 ) ) ;
#63235 = ORIENTED_EDGE ( 'NONE', *, *, #1321, .T. ) ;
#63236 = CARTESIAN_POINT ( 'NONE',  ( 2.564635614221720594, -21.35862533600356983, -1.500000000000002220 ) ) ;
#63237 = CARTESIAN_POINT ( 'NONE',  ( -102.5228709571500758, -23.48786465467241769, 11.44779295918254114 ) ) ;
#63238 = LINE ( 'NONE', #40391, #99875 ) ;
#63239 = CARTESIAN_POINT ( 'NONE',  ( -71.62287095715005592, -23.48786465467241413, 11.44779295918254469 ) ) ;
#63240 = CIRCLE ( 'NONE', #25990, 1.249999999999997558 ) ;
#63241 = CARTESIAN_POINT ( 'NONE',  ( -68.62287095715007013, -23.72773821059536559, 11.05748984161097681 ) ) ;
#63242 = CARTESIAN_POINT ( 'NONE',  ( 22.74528686061176685, 3.085755641335488964, -1.500000000000002220 ) ) ;
#63243 = PERSON_AND_ORGANIZATION ( #70597, #27821 ) ;
#63244 = CARTESIAN_POINT ( 'NONE',  ( 11.62916340711181284, -5.965225279485572685, 28.75961759920349792 ) ) ;
#63245 = DIRECTION ( 'NONE',  ( -3.773278334453079618E-23, 0.9999999999976377785, 2.173523156925978705E-06 ) ) ;
#63246 = CARTESIAN_POINT ( 'NONE',  ( -14.99618758923778117, -13.25627519679515665, 11.49999999999999645 ) ) ;
#63247 = CARTESIAN_POINT ( 'NONE',  ( 13.32458981842495049, -5.152774720514427642, -26.34181586963115507 ) ) ;
#63248 = CARTESIAN_POINT ( 'NONE',  ( -46.52287095715006160, -29.50248528299804818, 1.056150453629033370 ) ) ;
#63249 = VECTOR ( 'NONE', #21338, 1000.000000000000114 ) ;
#63250 = CARTESIAN_POINT ( 'NONE',  ( 4.334227700317904386, -5.876774720514402972, 18.30971318885719157 ) ) ;
#63251 = CARTESIAN_POINT ( 'NONE',  ( -60.52287095715006160, -23.48786465467241058, 11.44779295918254824 ) ) ;
#63252 = ORIENTED_EDGE ( 'NONE', *, *, #10579, .T. ) ;
#63253 = DIRECTION ( 'NONE',  ( 0.000000000000000000, -1.000000000000000000, 0.000000000000000000 ) ) ;
#63254 = CIRCLE ( 'NONE', #94013, 130.2784398600581710 ) ;
#63255 = CARTESIAN_POINT ( 'NONE',  ( 19.96715809174937561, -8.635335823514383335, 11.49999999999998934 ) ) ;
#63256 = CYLINDRICAL_SURFACE ( 'NONE', #5882, 2.040000000000000036 ) ;
#63257 = CARTESIAN_POINT ( 'NONE',  ( 5.252985061998082017, 18.97096265210048571, -1.500000000000002220 ) ) ;
#63258 = CARTESIAN_POINT ( 'NONE',  ( -27.70544111104076990, -24.60484793945295934, 1.628749883096155981 ) ) ;
#63259 = EDGE_CURVE ( 'NONE', #84371, #53585, #73828, .T. ) ;
#63260 = AXIS2_PLACEMENT_3D ( 'NONE', #12149, #35510, #66485 ) ;
#63261 = CARTESIAN_POINT ( 'NONE',  ( -109.3640311185025098, -25.31697976619958013, 4.352105570880266505 ) ) ;
#63262 = APPROVAL_DATE_TIME ( #32292, #76640 ) ;
#63263 = VECTOR ( 'NONE', #96849, 1000.000000000000114 ) ;
#63264 = FACE_OUTER_BOUND ( 'NONE', #31560, .T. ) ;
#63265 = CARTESIAN_POINT ( 'NONE',  ( 7.089543269230769162, -6.376774720514413630, 19.75741185897435415 ) ) ;
#63266 = CARTESIAN_POINT ( 'NONE',  ( -15.41819309731374510, 13.62919173607049927, 11.49999999999999645 ) ) ;
#63267 = CARTESIAN_POINT ( 'NONE',  ( 4.518955212990007908, -5.876774720514421624, 20.94857968174986951 ) ) ;
#63268 = B_SPLINE_CURVE_WITH_KNOTS ( 'NONE', 3,
 ( #7278, #99617, #92020, #85913 ),
 .UNSPECIFIED., .F., .F.,
 ( 4, 4 ),
 ( 0.000000000000000000, 9.999999999998897304E-05 ),
 .UNSPECIFIED. ) ;
#63269 = CARTESIAN_POINT ( 'NONE',  ( -47.62287095715007723, -24.34917612406837861, 0.1852690917426594308 ) ) ;
#63270 = AXIS2_PLACEMENT_3D ( 'NONE', #31898, #85684, #16164 ) ;
#63272 = EDGE_CURVE ( 'NONE', #15143, #72803, #21869, .T. ) ;
#63271 = CARTESIAN_POINT ( 'NONE',  ( -20.05226876979747530, -10.47825485868949613, 11.49999999999999645 ) ) ;
#63273 = ORIENTED_EDGE ( 'NONE', *, *, #96308, .F. ) ;
#63274 =( NAMED_UNIT ( * ) PLANE_ANGLE_UNIT ( ) SI_UNIT ( $, .RADIAN. ) );
#63275 = CARTESIAN_POINT ( 'NONE',  ( -99.59758909298055585, -25.26387354126681117, 4.277504120023178480 ) ) ;
#63276 = CARTESIAN_POINT ( 'NONE',  ( -28.98875734969026041, -0.3587747205144265483, 25.61802280011862720 ) ) ;
#63277 = AXIS2_PLACEMENT_3D ( 'NONE', #78483, #24699, #17599 ) ;
#63278 = CARTESIAN_POINT ( 'NONE',  ( -74.52287095715007581, -23.47596703998600631, 11.44779298504228748 ) ) ;
#63279 = CARTESIAN_POINT ( 'NONE',  ( 15.22396167909262488, -3.565890571771469286, -27.22573842070922367 ) ) ;
#63280 = CARTESIAN_POINT ( 'NONE',  ( -25.53098197642538736, -24.93062915712978977, 4.942811675010964301 ) ) ;
#63281 = FACE_OUTER_BOUND ( 'NONE', #797, .T. ) ;
#63282 = VERTEX_POINT ( 'NONE', #29389 ) ;
#63283 = CARTESIAN_POINT ( 'NONE',  ( -79.71799800425125682, -25.31596267615770657, 5.176233665374946114 ) ) ;
#63284 = CARTESIAN_POINT ( 'NONE',  ( 2.723195454624489642, 22.67993996152103620, -1.500000000000002220 ) ) ;
#63285 = DIRECTION ( 'NONE',  ( 0.000000000000000000, -0.9999999999976377785, -2.173523156925979552E-06 ) ) ;
#63286 = CARTESIAN_POINT ( 'NONE',  ( -7.641025641025640525, -5.876774720514418071, 20.36458333333334281 ) ) ;
#63287 = CARTESIAN_POINT ( 'NONE',  ( -63.63676845969973073, -24.15620529776628089, 10.23563542870660470 ) ) ;
#63288 = CARTESIAN_POINT ( 'NONE',  ( -18.83616483605274539, -12.25834331966736102, 11.49999999999999645 ) ) ;
#63289 = ORIENTED_EDGE ( 'NONE', *, *, #32636, .T. ) ;
#63290 = CARTESIAN_POINT ( 'NONE',  ( -86.52287095715006160, -29.50248528299804818, 1.056150453629040253 ) ) ;
#63291 = CARTESIAN_POINT ( 'NONE',  ( -4.809782828112996178, 21.40371668077904488, -1.500000000000002220 ) ) ;
#63292 = CARTESIAN_POINT ( 'NONE',  ( -126.8949105597723417, -25.34741607406076724, 3.801658267186113438 ) ) ;
#63293 = EDGE_CURVE ( 'NONE', #41031, #36561, #59860, .T. ) ;
#63294 = CARTESIAN_POINT ( 'NONE',  ( -44.59357593954516119, -24.15620529776627734, 10.23563542870660470 ) ) ;
#63295 = CARTESIAN_POINT ( 'NONE',  ( -69.21694530810552237, -25.13479670434804447, 7.034542371138676309 ) ) ;
#63296 = ORIENTED_EDGE ( 'NONE', *, *, #33058, .F. ) ;
#63297 = DIRECTION ( 'NONE',  ( 0.000000000000000000, 0.000000000000000000, -1.000000000000000000 ) ) ;
#63298 = LINE ( 'NONE', #56184, #59226 ) ;
#63299 = VERTEX_POINT ( 'NONE', #75549 ) ;
#63300 = CARTESIAN_POINT ( 'NONE',  ( -7.951223608505463503, 18.87544906973805325, 11.49999999999998934 ) ) ;
#63301 = ORIENTED_EDGE ( 'NONE', *, *, #100223, .T. ) ;
#63302 = ORIENTED_EDGE ( 'NONE', *, *, #58727, .T. ) ;
#63303 = ORIENTED_EDGE ( 'NONE', *, *, #46204, .F. ) ;
#63304 = EDGE_LOOP ( 'NONE', ( #57981, #95307, #41446, #41450, #79128 ) ) ;
#63305 = B_SPLINE_CURVE_WITH_KNOTS ( 'NONE', 3,
 ( #34242, #81906, #58575, #12384 ),
 .UNSPECIFIED., .F., .F.,
 ( 4, 4 ),
 ( 0.06880487856767243671, 0.06980562560843792119 ),
 .UNSPECIFIED. ) ;
#63306 = CARTESIAN_POINT ( 'NONE',  ( -17.14199295335891904, -15.44578658782692671, 11.49999999999998934 ) ) ;
#63307 = CARTESIAN_POINT ( 'NONE',  ( -112.5228709571500616, -23.96177878511310055, 10.65340807706329507 ) ) ;
#63308 = CARTESIAN_POINT ( 'NONE',  ( -3.898967980886277829, 19.90457959416237088, -1.500000000000002220 ) ) ;
#63309 = ORIENTED_EDGE ( 'NONE', *, *, #38589, .F. ) ;
#63310 = EDGE_CURVE ( 'NONE', #66922, #94858, #6076, .T. ) ;
#63311 = DIRECTION ( 'NONE',  ( -1.000000000000000000, -0.000000000000000000, 0.000000000000000000 ) ) ;
#63312 = EDGE_CURVE ( 'NONE', #87273, #43589, #70461, .T. ) ;
#63313 = CARTESIAN_POINT ( 'NONE',  ( -92.54656292449074328, -24.51314013834316796, 0.6176544820404240577 ) ) ;
#63314 = EDGE_CURVE ( 'NONE', #15357, #3028, #92781, .T. ) ;
#63315 = CARTESIAN_POINT ( 'NONE',  ( -6.499999999999992895, 4.999999999999999112, 2.100000000000000089 ) ) ;
#63316 = CARTESIAN_POINT ( 'NONE',  ( 4.653515142448186204, -5.876774720514414518, 19.86181745814487343 ) ) ;
#63318 = ORIENTED_EDGE ( 'NONE', *, *, #48249, .F. ) ;
#63317 = CARTESIAN_POINT ( 'NONE',  ( 10.13398631766115443, 18.95262098133242290, 11.49999999999999645 ) ) ;
#63319 = CARTESIAN_POINT ( 'NONE',  ( -75.55895860488308813, -23.85016227208580730, -0.8807180028928284221 ) ) ;
#63320 = CARTESIAN_POINT ( 'NONE',  ( -104.6228709571500985, -24.50216790748100237, 0.6166512839513698108 ) ) ;
#63321 = ADVANCED_FACE ( 'NONE', ( #23263 ), #99396, .F. ) ;
#63322 = ORIENTED_EDGE ( 'NONE', *, *, #46793, .F. ) ;
#63323 = CARTESIAN_POINT ( 'NONE',  ( 15.70846742882596025, 13.54617332914617478, -1.500000000000002220 ) ) ;
#63324 = VECTOR ( 'NONE', #84009, 1000.000000000000000 ) ;
#63325 = ORIENTED_EDGE ( 'NONE', *, *, #49228, .T. ) ;
#63327 = ORIENTED_EDGE ( 'NONE', *, *, #18637, .T. ) ;
#63326 = DIRECTION ( 'NONE',  ( -3.773278334453079030E-23, 0.9999999999976377785, 2.173523156925979128E-06 ) ) ;
#63328 = CARTESIAN_POINT ( 'NONE',  ( -41.64787139066377364, -23.96169478059712432, 10.65365249895718591 ) ) ;
#63329 = CARTESIAN_POINT ( 'NONE',  ( -76.62287095715007013, -29.50247984919015209, -1.443849546365053582 ) ) ;
#63330 = VERTEX_POINT ( 'NONE', #946 ) ;
#63331 = VERTEX_POINT ( 'NONE', #61360 ) ;
#63332 = CARTESIAN_POINT ( 'NONE',  ( -28.62287095715004526, -24.50732993938405357, 8.947790418389013567 ) ) ;
#63333 = CARTESIAN_POINT ( 'NONE',  ( -116.9228709571500389, -23.47596703998600276, 11.44779298504227860 ) ) ;
#63335 = EDGE_CURVE ( 'NONE', #25620, #14844, #38774, .T. ) ;
#63334 = CARTESIAN_POINT ( 'NONE',  ( -52.62287095715005592, -29.50250786944525672, 11.44777988621624054 ) ) ;
#63336 = EDGE_CURVE ( 'NONE', #53781, #26222, #83526, .T. ) ;
#63337 = CARTESIAN_POINT ( 'NONE',  ( 20.22059317821533853, 8.664326447042464352, 11.49999999999999645 ) ) ;
#63338 = CARTESIAN_POINT ( 'NONE',  ( 0.000000000000000000, -5.876774720514426953, 0.000000000000000000 ) ) ;
#63339 = CARTESIAN_POINT ( 'NONE',  ( -20.69567741759225399, -9.018594580484563750, 11.49999999999998934 ) ) ;
#63340 = CARTESIAN_POINT ( 'NONE',  ( 16.30764028314251846, 13.22082560946828522, -1.500000000000002220 ) ) ;
#63342 = VERTEX_POINT ( 'NONE', #31896 ) ;
#63341 = DIRECTION ( 'NONE',  ( -0.9951627101165076983, 0.000000000000000000, 0.09824042138329588947 ) ) ;
#63343 = AXIS2_PLACEMENT_3D ( 'NONE', #55610, #54111, #54599 ) ;
#63344 = ORIENTED_EDGE ( 'NONE', *, *, #34820, .T. ) ;
#63345 = AXIS2_PLACEMENT_3D ( 'NONE', #20966, #89493, #13352 ) ;
#63346 = DIRECTION ( 'NONE',  ( -0.000000000000000000, 1.000000000000000000, -0.000000000000000000 ) ) ;
#63347 = ADVANCED_FACE ( 'NONE', ( #14662 ), #27161, .T. ) ;
#63348 = LINE ( 'NONE', #46105, #47336 ) ;
#63349 = ORIENTED_EDGE ( 'NONE', *, *, #44619, .F. ) ;
#63350 = CARTESIAN_POINT ( 'NONE',  ( 17.87031378931267867, -11.31994873005049129, 11.49999999999998934 ) ) ;
#63351 = FACE_OUTER_BOUND ( 'NONE', #55174, .T. ) ;
#63352 = B_SPLINE_CURVE_WITH_KNOTS ( 'NONE', 3,
 ( #62749, #93666, #38385, #16040 ),
 .UNSPECIFIED., .F., .F.,
 ( 4, 4 ),
 ( 0.000000000000000000, 1.000000000000000000 ),
 .UNSPECIFIED. ) ;
#63353 = CARTESIAN_POINT ( 'NONE',  ( -50.40895856474225667, -25.03148742036013630, 7.563174219458152159 ) ) ;
#63354 = CARTESIAN_POINT ( 'NONE',  ( -121.6234957139205193, -24.65952944569305316, 1.056160979905707897 ) ) ;
#63355 = CARTESIAN_POINT ( 'NONE',  ( -120.5228709571500616, -24.99156044556120904, 7.747789690856173195 ) ) ;
#63356 = LINE ( 'NONE', #47119, #8123 ) ;
#63357 = CARTESIAN_POINT ( 'NONE',  ( 20.70802603420765564, 8.137917507125113303, -1.500000000000002220 ) ) ;
#63358 = CARTESIAN_POINT ( 'NONE',  ( -114.5542499131790777, -24.15543982623907837, -0.2315651400026444429 ) ) ;
#63359 = ADVANCED_FACE ( 'NONE', ( #6557 ), #38006, .T. ) ;
#63360 = B_SPLINE_CURVE_WITH_KNOTS ( 'NONE', 3,
 ( #1077, #22878, #15786, #53368, #23899, #53866 ),
 .UNSPECIFIED., .F., .F.,
 ( 4, 2, 4 ),
 ( 1.571603873469763250E-05, 0.001396933878470195617, 0.002778151718205693673 ),
 .UNSPECIFIED. ) ;
#63361 = ORIENTED_EDGE ( 'NONE', *, *, #6468, .T. ) ;
#63362 = CARTESIAN_POINT ( 'NONE',  ( -6.741682653110981249, 0.3587747205144265483, 30.62569541381301619 ) ) ;
#63363 = CARTESIAN_POINT ( 'NONE',  ( 32.85081302853804885, -3.622774720514426949, -13.10817780685210643 ) ) ;
#63364 = CARTESIAN_POINT ( 'NONE',  ( -126.6245542812432774, -23.96119346886880663, -0.6495511937832031402 ) ) ;
#63365 = ADVANCED_FACE ( 'NONE', ( #53744 ), #8053, .T. ) ;
#63366 = CYLINDRICAL_SURFACE ( 'NONE', #91649, 1.149999999999999911 ) ;
#63367 = DIRECTION ( 'NONE',  ( -7.960204194457801640E-17, -1.000000000000000000, 0.000000000000000000 ) ) ;
#63368 = ADVANCED_FACE ( 'NONE', ( #1958 ), #55250, .F. ) ;
#63369 = CARTESIAN_POINT ( 'NONE',  ( 16.53150372360616771, 10.32350692489952593, -1.500000000000002220 ) ) ;
#63370 = CARTESIAN_POINT ( 'NONE',  ( 13.27131465344908001, -16.79725507166503462, 11.49999999999998934 ) ) ;
#63371 = CARTESIAN_POINT ( 'NONE',  ( -29.49875734969025842, 5.965225279485572685, 17.86602280011862476 ) ) ;
#63372 = CARTESIAN_POINT ( 'NONE',  ( -60.63669123105633219, -24.52399227489755518, 9.353111116819372128 ) ) ;
#63373 = PLANE ( 'NONE',  #30870 ) ;
#63374 = DIRECTION ( 'NONE',  ( 0.000000000000000000, -1.000000000000000000, 0.000000000000000000 ) ) ;
#63375 = CARTESIAN_POINT ( 'NONE',  ( -4.239441843796335263, -22.36999388947090139, -1.500000000000002220 ) ) ;
#63376 = EDGE_CURVE ( 'NONE', #85295, #89124, #25275, .T. ) ;
#63377 = CARTESIAN_POINT ( 'NONE',  ( -98.52218359600611564, -23.48783264082476663, -1.443836473390090136 ) ) ;
#63378 = DIRECTION ( 'NONE',  ( -3.773278334444167608E-23, 1.000000000000000000, 0.000000000000000000 ) ) ;
#63379 = CARTESIAN_POINT ( 'NONE',  ( -13.97081141688431138, 14.13901428111770819, 11.49999999999999645 ) ) ;
#63380 = CARTESIAN_POINT ( 'NONE',  ( -84.52287095715007581, -23.48783264082477018, -1.443836473390090802 ) ) ;
#63381 = CARTESIAN_POINT ( 'NONE',  ( -89.81226385320383088, -25.05712135967894838, 7.447789548357302891 ) ) ;
#63382 = LINE ( 'NONE', #49155, #3549 ) ;
#63383 = ORIENTED_EDGE ( 'NONE', *, *, #63603, .T. ) ;
#63384 = LINE ( 'NONE', #17682, #21783 ) ;
#63385 = CARTESIAN_POINT ( 'NONE',  ( -50.62287095715005592, -29.50247984919015209, -1.443849546365058689 ) ) ;
#63386 = DIRECTION ( 'NONE',  ( 0.000000000000000000, -1.000000000000000000, 0.000000000000000000 ) ) ;
#63387 = CARTESIAN_POINT ( 'NONE',  ( 2.186256072416925544, -21.55203199515037582, 11.49999999999998934 ) ) ;
#63388 = LINE ( 'NONE', #9073, #49652 ) ;
#63389 = CARTESIAN_POINT ( 'NONE',  ( -19.46337940159461866, -0.4807646128305608779, -1.500000000000002220 ) ) ;
#63390 = CARTESIAN_POINT ( 'NONE',  ( -123.6228709571500559, -23.48786465467241769, 11.44779295918253759 ) ) ;
#63391 = ORIENTED_EDGE ( 'NONE', *, *, #45427, .T. ) ;
#63392 = CARTESIAN_POINT ( 'NONE',  ( 19.51578053514377586, 5.923290232019536639, 11.49999999999999645 ) ) ;
#63393 = DIRECTION ( 'NONE',  ( 1.000000000000000000, 3.773278334444167608E-23, 8.201307833595939069E-29 ) ) ;
#63394 = VECTOR ( 'NONE', #65124, 1000.000000000000114 ) ;
#63395 = FACE_OUTER_BOUND ( 'NONE', #70018, .T. ) ;
#63396 = ORIENTED_EDGE ( 'NONE', *, *, #32578, .F. ) ;
#63397 = CARTESIAN_POINT ( 'NONE',  ( -79.12743195124619433, -25.17601835801890076, 6.783621481769894324 ) ) ;
#63398 = CARTESIAN_POINT ( 'NONE',  ( -29.62287095715003105, -23.66062849325336259, -1.053491143263840746 ) ) ;
#63399 = CARTESIAN_POINT ( 'NONE',  ( 7.311104923646705167, -6.376774720514415407, 20.13320233724603980 ) ) ;
#63400 = CARTESIAN_POINT ( 'NONE',  ( -125.6228709571500559, -23.48786465467241769, 11.44779295918253403 ) ) ;
#63401 = DIRECTION ( 'NONE',  ( 0.000000000000000000, 0.000000000000000000, 1.000000000000000000 ) ) ;
#63402 = CARTESIAN_POINT ( 'NONE',  ( 14.11618873683251252, 14.29484301466228047, -1.500000000000002220 ) ) ;
#63403 = PLANE ( 'NONE',  #66260 ) ;
#63404 = ORIENTED_EDGE ( 'NONE', *, *, #15552, .F. ) ;
#63405 = CARTESIAN_POINT ( 'NONE',  ( 13.91401389203221406, -3.316774720514426456, 158.0376437107427137 ) ) ;
#63406 = B_SPLINE_CURVE_WITH_KNOTS ( 'NONE', 3,
 ( #13635, #60346, #21247, #21743 ),
 .UNSPECIFIED., .F., .F.,
 ( 4, 4 ),
 ( 0.6459941988912109023, 0.6543842573219610381 ),
 .UNSPECIFIED. ) ;
#63407 = VECTOR ( 'NONE', #81197, 1000.000000000000000 ) ;
#63408 = CARTESIAN_POINT ( 'NONE',  ( -15.63304604236160067, -16.83380969201049382, 11.49999999999999645 ) ) ;
#63409 = CARTESIAN_POINT ( 'NONE',  ( 16.28376985728763415, 15.88423345705086298, -1.500000000000002220 ) ) ;
#63410 = ORIENTED_EDGE ( 'NONE', *, *, #14237, .T. ) ;
#63411 = CARTESIAN_POINT ( 'NONE',  ( -31.52287095715006160, -23.47596703998600631, 11.44779298504229459 ) ) ;
#63412 = CARTESIAN_POINT ( 'NONE',  ( -75.62287095715009855, -24.83620972994592435, 8.398175272781363887 ) ) ;
#63413 = CARTESIAN_POINT ( 'NONE',  ( -81.52287095715007581, -24.33927499327856125, 9.819080762295815390 ) ) ;
#63414 = CARTESIAN_POINT ( 'NONE',  ( -61.47555918000787756, -25.07008561068857588, 7.435194656350822662 ) ) ;
#63415 = PLANE ( 'NONE',  #18700 ) ;
#63416 = EDGE_CURVE ( 'NONE', #67214, #5889, #16662, .T. ) ;
#63417 = CARTESIAN_POINT ( 'NONE',  ( -7.160000000000000142, -0.4583917923827245389, 5.886156785137588443 ) ) ;
#63418 = CARTESIAN_POINT ( 'NONE',  ( -76.62287095715007013, -24.66019654487199730, 8.947790411086128159 ) ) ;
#63419 = CARTESIAN_POINT ( 'NONE',  ( -58.52207422368198309, -23.48783264082477018, -1.443836473390093689 ) ) ;
#63420 = VERTEX_POINT ( 'NONE', #55751 ) ;
#63421 = EDGE_CURVE ( 'NONE', #871, #92857, #40520, .T. ) ;
#63422 = CARTESIAN_POINT ( 'NONE',  ( -18.82316870354832616, 7.800066519331792847, 11.49999999999998934 ) ) ;
#63424 = ADVANCED_FACE ( 'NONE', ( #94285 ), #2960, .F. ) ;
#63423 = ORIENTED_EDGE ( 'NONE', *, *, #27493, .T. ) ;
#63425 = CARTESIAN_POINT ( 'NONE',  ( -12.88233675513024856, -19.01995677650982230, 11.49999999999998934 ) ) ;
#63426 = CARTESIAN_POINT ( 'NONE',  ( -1.540913562699879114, -5.876774720514409189, 19.44316438561912008 ) ) ;
#63427 = EDGE_CURVE ( 'NONE', #54139, #100298, #19371, .T. ) ;
#63428 = ORIENTED_EDGE ( 'NONE', *, *, #84339, .F. ) ;
#63429 = CARTESIAN_POINT ( 'NONE',  ( -101.6228709571500559, -24.65952944569304606, 1.056160979905702790 ) ) ;
#63430 = EDGE_CURVE ( 'NONE', #80664, #30045, #70965, .T. ) ;
#63431 = LINE ( 'NONE', #94348, #36889 ) ;
#63432 = EDGE_CURVE ( 'NONE', #31584, #22977, #9552, .T. ) ;
#63433 = CARTESIAN_POINT ( 'NONE',  ( -117.2171617987493448, -25.23514715042687229, 6.311476322788518445 ) ) ;
#63435 = ORIENTED_EDGE ( 'NONE', *, *, #40335, .F. ) ;
#63434 = CARTESIAN_POINT ( 'NONE',  ( -13.37813101364405100, 16.61575060780308277, 11.49999999999999645 ) ) ;
#63436 = VERTEX_POINT ( 'NONE', #1456 ) ;
#63437 = CARTESIAN_POINT ( 'NONE',  ( -8.951960448472247478, 20.35530821588910300, 11.49999999999998934 ) ) ;
#63438 = CARTESIAN_POINT ( 'NONE',  ( 17.27521350410721368, -11.31798593588896829, -1.500000000000002220 ) ) ;
#63439 = PERSON ( 'NAUO-PER1', 'UNSPECIFIED', 'UNSPECIFIED', ('UNSPECIFIED'), ('UNSPECIFIED'), ('UNSPECIFIED') ) ;
#63440 = VERTEX_POINT ( 'NONE', #80068 ) ;
#63441 = CARTESIAN_POINT ( 'NONE',  ( 0.3627416911114360598, -6.376774720514411854, 19.59793130852656873 ) ) ;
#63442 = CARTESIAN_POINT ( 'NONE',  ( -95.58393028260560698, -24.92592662359561473, 8.075495903017998245 ) ) ;
#63443 = ORIENTED_EDGE ( 'NONE', *, *, #93919, .T. ) ;
#63444 = CARTESIAN_POINT ( 'NONE',  ( -87.62287095715004170, -24.64898659630528854, 1.056161002820827921 ) ) ;
#63445 = ORIENTED_EDGE ( 'NONE', *, *, #24275, .F. ) ;
#63446 = CARTESIAN_POINT ( 'NONE',  ( -58.64320803498131340, -23.96169478059713143, 10.65365249895718058 ) ) ;
#63447 = DIRECTION ( 'NONE',  ( 0.000000000000000000, 0.000000000000000000, 1.000000000000000000 ) ) ;
#63448 = CARTESIAN_POINT ( 'NONE',  ( 18.69404101259207707, 9.334567778723176446, -1.500000000000002220 ) ) ;
#63449 = EDGE_CURVE ( 'NONE', #78408, #29710, #16761, .T. ) ;
#63450 = CARTESIAN_POINT ( 'NONE',  ( -4.983756199382824548, -21.29032736245130053, 11.49999999999999645 ) ) ;
#63451 = CARTESIAN_POINT ( 'NONE',  ( 25.06178640545682867, -4.997093759973374461, -9.841412737801366717 ) ) ;
#63452 = FACE_OUTER_BOUND ( 'NONE', #30097, .T. ) ;
#63453 = CARTESIAN_POINT ( 'NONE',  ( 14.28312119630281174, -17.39864199977734671, -1.500000000000002220 ) ) ;
#63454 = CARTESIAN_POINT ( 'NONE',  ( -118.5181897846719181, -24.35071581493543746, 9.817618358456021710 ) ) ;
#63455 = CARTESIAN_POINT ( 'NONE',  ( -72.52287095715010423, -24.51387760970725083, 9.387446482453427166 ) ) ;
#63456 = LINE ( 'NONE', #70545, #54015 ) ;
#63458 = ORIENTED_EDGE ( 'NONE', *, *, #59500, .F. ) ;
#63457 = EDGE_CURVE ( 'NONE', #50697, #15254, #94787, .T. ) ;
#63459 = ORIENTED_EDGE ( 'NONE', *, *, #82458, .F. ) ;
#63460 = ORIENTED_EDGE ( 'NONE', *, *, #76059, .F. ) ;
#63461 = VECTOR ( 'NONE', #75441, 1000.000000000000000 ) ;
#63462 = CARTESIAN_POINT ( 'NONE',  ( -99.41830603981939873, -25.12215564308212024, 6.591151844143220195 ) ) ;
#63463 = VERTEX_POINT ( 'NONE', #18168 ) ;
#63464 = CARTESIAN_POINT ( 'NONE',  ( -21.42254595866439004, -0.3319015934494286557, -1.500000000000002220 ) ) ;
#63465 = CARTESIAN_POINT ( 'NONE',  ( 17.53502452033532677, 13.85421504792973479, 11.49999999999999645 ) ) ;
#63466 = ORIENTED_EDGE ( 'NONE', *, *, #51188, .F. ) ;
#63467 = CARTESIAN_POINT ( 'NONE',  ( 32.56681547219513817, -5.361656835957732348, -1.802091617189489403 ) ) ;
#63468 = CARTESIAN_POINT ( 'NONE',  ( -17.44821286160079410, -11.81026508430653088, -1.500000000000002220 ) ) ;
#63469 = CARTESIAN_POINT ( 'NONE',  ( -30.49971861685504138, -24.27034544923275661, 9.960304333224314632 ) ) ;
#63470 = CARTESIAN_POINT ( 'NONE',  ( 13.89251353435424363, -14.32104260081073832, -1.500000000000002220 ) ) ;
#63471 = DIRECTION ( 'NONE',  ( -3.773278334453079030E-23, 0.9999999999976377785, 2.173523156925979128E-06 ) ) ;
#63472 = CARTESIAN_POINT ( 'NONE',  ( 2.955024617976266033, -5.876774720514415407, 20.58370193283586858 ) ) ;
#63473 = CARTESIAN_POINT ( 'NONE',  ( -1.213202359833694732, 22.00568734548514627, -1.500000000000002220 ) ) ;
#63474 = CARTESIAN_POINT ( 'NONE',  ( -52.62287095715005592, -23.47593901973091235, -1.443836447539009749 ) ) ;
#63475 = ORIENTED_EDGE ( 'NONE', *, *, #97033, .F. ) ;
#63476 = CARTESIAN_POINT ( 'NONE',  ( -65.58909869047282371, -24.52399227489126687, 9.353111116836526406 ) ) ;
#63477 = B_SPLINE_CURVE_WITH_KNOTS ( 'NONE', 3,
 ( #95513, #55461, #55968, #86398 ),
 .UNSPECIFIED., .F., .F.,
 ( 4, 4 ),
 ( 0.000000000000000000, 9.999999999998897304E-05 ),
 .UNSPECIFIED. ) ;
#63478 = CARTESIAN_POINT ( 'NONE',  ( -20.77875734969026311, -5.356774720514425603, 27.31649921512899937 ) ) ;
#63479 = CARTESIAN_POINT ( 'NONE',  ( -14.93763623016880082, -14.57113377498261997, 11.49999999999999645 ) ) ;
#63480 = EDGE_CURVE ( 'NONE', #24375, #33030, #50835, .T. ) ;
#63481 = VECTOR ( 'NONE', #95813, 1000.000000000000000 ) ;
#63482 = CARTESIAN_POINT ( 'NONE',  ( 3.252401863874215593, -0.3587747205143964613, -29.35688408629929214 ) ) ;
#63483 = LOCAL_TIME ( 0, 54, 15.00000000000000000, #93159 ) ;
#63484 = CARTESIAN_POINT ( 'NONE',  ( -61.55620429048339304, -24.65952944569304606, 1.056160979905697461 ) ) ;
#63485 = CARTESIAN_POINT ( 'NONE',  ( -3.453506354162970915, -21.03206338698385736, -1.500000000000002220 ) ) ;
#63486 = CARTESIAN_POINT ( 'NONE',  ( -71.62287095715005592, -23.47596703998600631, 11.44779298504227683 ) ) ;
#63487 = CARTESIAN_POINT ( 'NONE',  ( -50.91374622504534386, -25.21061005848796555, 3.406474964634027103 ) ) ;
#63488 = EDGE_CURVE ( 'NONE', #60161, #82250, #8602, .T. ) ;
#63489 = CARTESIAN_POINT ( 'NONE',  ( -71.55620429048339304, -24.65952944569304606, 1.056160979905697461 ) ) ;
#63490 = DIRECTION ( 'NONE',  ( 0.000000000000000000, -1.000000000000000000, 0.000000000000000000 ) ) ;
#63491 = CARTESIAN_POINT ( 'NONE',  ( 22.48772827135616126, 0.8316936486096353498, -1.500000000000002220 ) ) ;
#63492 = CARTESIAN_POINT ( 'NONE',  ( 33.61456970919604714, -5.965225279485572685, -11.35828564741647462 ) ) ;
#63493 = ORIENTED_EDGE ( 'NONE', *, *, #10631, .F. ) ;
#63494 = CARTESIAN_POINT ( 'NONE',  ( -79.10665409224128553, -25.30355450193266975, 5.239253019725047089 ) ) ;
#63495 = CARTESIAN_POINT ( 'NONE',  ( -1.358974358974355257, -5.876774720514426953, 21.75000000000000711 ) ) ;
#63496 = CARTESIAN_POINT ( 'NONE',  ( 19.18734209777730015, 4.435579877058994036, 11.49999999999999645 ) ) ;
#63497 = CARTESIAN_POINT ( 'NONE',  ( -32.07722060962682775, -25.12026506542016335, 2.831122744435439209 ) ) ;
#63498 = CARTESIAN_POINT ( 'NONE',  ( -39.52287095715006870, -24.64898659630528144, 1.056161002820819261 ) ) ;
#63499 = B_SPLINE_CURVE_WITH_KNOTS ( 'NONE', 3,
 ( #29576, #60553, #61041, #75251 ),
 .UNSPECIFIED., .F., .F.,
 ( 4, 4 ),
 ( 0.4708362126144793325, 0.4798426438865949217 ),
 .UNSPECIFIED. ) ;
#63500 = ORIENTED_EDGE ( 'NONE', *, *, #36502, .T. ) ;
#63501 = CARTESIAN_POINT ( 'NONE',  ( 23.60872659128563811, 0.000000000000000000, -2.097483029078132777 ) ) ;
#63502 = LINE ( 'NONE', #78184, #67537 ) ;
#63503 = CARTESIAN_POINT ( 'NONE',  ( -124.5553377431336486, -24.15620529776629510, 10.23563542870659404 ) ) ;
#63504 = B_SPLINE_CURVE_WITH_KNOTS ( 'NONE', 3,
 ( #35214, #27604, #13351, #58553 ),
 .UNSPECIFIED., .F., .F.,
 ( 4, 4 ),
 ( 0.05053608658242522006, 0.05954251785454105911 ),
 .UNSPECIFIED. ) ;
#63505 = DIRECTION ( 'NONE',  ( -0.000000000000000000, 1.000000000000000000, -0.000000000000000000 ) ) ;
#63506 = CARTESIAN_POINT ( 'NONE',  ( -8.281543130087330340, -17.94227898472161797, 11.49999999999998934 ) ) ;
#63507 = ORIENTED_EDGE ( 'NONE', *, *, #64010, .F. ) ;
#63508 = CARTESIAN_POINT ( 'NONE',  ( 0.4983251850863967269, 20.17815531296474418, 11.49999999999999645 ) ) ;
#63509 = CARTESIAN_POINT ( 'NONE',  ( 6.404294203292168142, -5.876774720514416295, 20.09052689972686423 ) ) ;
#63510 = ORIENTED_EDGE ( 'NONE', *, *, #58380, .F. ) ;
#63511 = CARTESIAN_POINT ( 'NONE',  ( 22.02124265030973760, -5.356774720514425603, 16.20402280011862217 ) ) ;
#63512 = PLANE ( 'NONE',  #8621 ) ;
#63513 = CARTESIAN_POINT ( 'NONE',  ( -19.80875734969026425, 0.3587747205144265483, 30.51402280011862089 ) ) ;
#63514 = CARTESIAN_POINT ( 'NONE',  ( -82.92287095715010992, -23.47593901973090524, -1.443836447538997536 ) ) ;
#63515 = DIRECTION ( 'NONE',  ( -3.773278334453079030E-23, 0.9999999999976377785, 2.173523156925979128E-06 ) ) ;
#63516 = CARTESIAN_POINT ( 'NONE',  ( -61.52287095715007581, -23.48783264082476308, -1.443836473390092356 ) ) ;
#63517 = CARTESIAN_POINT ( 'NONE',  ( 10.17626895549074817, -17.22257424524772418, 11.49999999999998934 ) ) ;
#63518 = DIRECTION ( 'NONE',  ( -3.773278334453079030E-23, 0.9999999999976377785, 2.173523156925979128E-06 ) ) ;
#63519 = CARTESIAN_POINT ( 'NONE',  ( -116.6262418075701817, -24.15620529776629155, 10.23563542870659759 ) ) ;
#63520 = ORIENTED_EDGE ( 'NONE', *, *, #99905, .T. ) ;
#63521 = CARTESIAN_POINT ( 'NONE',  ( -104.6228709571500559, -24.51387760970723306, 9.387446482453396968 ) ) ;
#63522 = LINE ( 'NONE', #92936, #34612 ) ;
#63523 = CARTESIAN_POINT ( 'NONE',  ( -118.5228709571500758, -23.48786465467241769, 11.44779295918253759 ) ) ;
#63524 = DIRECTION ( 'NONE',  ( -0.9994733861282923959, -0.000000000000000000, -0.03244919754393515293 ) ) ;
#63525 = VECTOR ( 'NONE', #45657, 1000.000000000000114 ) ;
#63526 = CARTESIAN_POINT ( 'NONE',  ( -124.5562042904833930, -24.65952944569305316, 1.056160979905708119 ) ) ;
#63527 = CARTESIAN_POINT ( 'NONE',  ( -83.50336294561820694, -24.51314013834315375, 0.6176544820404104019 ) ) ;
#63528 = DIRECTION ( 'NONE',  ( 0.000000000000000000, 0.000000000000000000, 1.000000000000000000 ) ) ;
#63529 = ADVANCED_FACE ( 'NONE', ( #47446 ), #86499, .T. ) ;
#63530 = FACE_OUTER_BOUND ( 'NONE', #33042, .T. ) ;
#63531 = VERTEX_POINT ( 'NONE', #92603 ) ;
#63532 = EDGE_CURVE ( 'NONE', #93020, #47315, #68975, .T. ) ;
#63533 = B_SPLINE_CURVE_WITH_KNOTS ( 'NONE', 3,
 ( #37128, #27153, #21881, #52859, #45250, #76175 ),
 .UNSPECIFIED., .F., .F.,
 ( 4, 2, 4 ),
 ( 6.391158118964603462E-06, 0.001387004593080780942, 0.002767618028042597225 ),
 .UNSPECIFIED. ) ;
#63534 = CARTESIAN_POINT ( 'NONE',  ( 6.837353022973060135, 19.10023500134885310, 11.49999999999998934 ) ) ;
#63536 = DIRECTION ( 'NONE',  ( -0.000000000000000000, 1.000000000000000000, -0.000000000000000000 ) ) ;
#63535 = B_SPLINE_CURVE_WITH_KNOTS ( 'NONE', 3,
 ( #34268, #73329, #41377, #26651, #26142, #88052, #89052, #88551, #80432, #25642, #87546, #79421, #10923, #40869, #96162, #95158, #41887, #57115, #71829, #42883, #96651, #65241, #95661, #48995, #2322, #19026, #48497, #87039, #33761, #18527, #72834, #27149, #73815, #56617, #10415, #50001, #33251, #80934, #3822, #25131, #11421, #58115, #64744, #42396, #64233, #19523, #72329, #50487, #11918, #32752, #18028, #79924, #12907, #60111 ),
 .UNSPECIFIED., .F., .F.,
 ( 4, 1, 1, 1, 1, 2, 2, 1, 2, 2, 1, 1, 2, 2, 1, 2, 2, 2, 1, 2, 2, 1, 1, 1, 2, 2, 1, 2, 2, 1, 1, 1, 2, 2, 4 ),
 ( 0.000000000000000000, 0.06250000000000152656, 0.09375000000000245637, 0.1093750000000030947, 0.1171875000000032474, 0.1210937500000031780, 0.1250000000000031086, 0.1562500000000031364, 0.1718750000000030254, 0.1875000000000029143, 0.2187500000000029421, 0.2343750000000028311, 0.2421875000000027478, 0.2500000000000026645, 0.3125000000000017764, 0.3437500000000013323, 0.3750000000000008882, 0.4999999999999987232, 0.5624999999999977796, 0.5937499999999972244, 0.6249999999999965583, 0.6874999999999955591, 0.7187499999999950040, 0.7343749999999950040, 0.7421874999999950040, 0.7499999999999951150, 0.7812499999999951150, 0.7968749999999953371, 0.8124999999999956701, 0.8437499999999961142, 0.8593749999999962252, 0.8671874999999961142, 0.8710937499999964473, 0.8749999999999966693, 1.000000000000000000 ),
 .UNSPECIFIED. ) ;
#63537 = EDGE_CURVE ( 'NONE', #99976, #80, #53136, .T. ) ;
#63538 = CARTESIAN_POINT ( 'NONE',  ( -34.59403392823487167, -24.15543982623907127, -0.2315651400026574880 ) ) ;
#63539 = APPROVAL_PERSON_ORGANIZATION ( #10450, #19617, #3860 ) ;
#63540 = PLANE ( 'NONE',  #65483 ) ;
#63541 = EDGE_CURVE ( 'NONE', #27095, #31243, #31716, .T. ) ;
#63542 = ORIENTED_EDGE ( 'NONE', *, *, #44876, .F. ) ;
#63543 = CARTESIAN_POINT ( 'NONE',  ( -81.62287095715004170, -23.96127896941632685, -0.6493128931037849272 ) ) ;
#63544 = VECTOR ( 'NONE', #6923, 1000.000000000000114 ) ;
#63545 = CARTESIAN_POINT ( 'NONE',  ( 19.32837167043147986, -5.866312143582237404, -1.500000000000002220 ) ) ;
#63546 = ADVANCED_FACE ( 'NONE', ( #93599 ), #46442, .F. ) ;
#63547 = CARTESIAN_POINT ( 'NONE',  ( -19.39432879369159224, 8.380699159679657839, 11.49999999999999645 ) ) ;
#63548 = LOCAL_TIME ( 0, 54, 15.00000000000000000, #62118 ) ;
#63549 = CARTESIAN_POINT ( 'NONE',  ( -10.67647856527443473, 19.39090429279614369, -1.500000000000002220 ) ) ;
#63550 = EDGE_CURVE ( 'NONE', #10358, #34532, #764, .T. ) ;
#63551 = CARTESIAN_POINT ( 'NONE',  ( 16.43461662053371697, -12.34185696772103391, 11.49999999999998934 ) ) ;
#63552 = CARTESIAN_POINT ( 'NONE',  ( -79.52287095715006160, -23.47596703998600631, 11.44779298504228571 ) ) ;
#63553 = VERTEX_POINT ( 'NONE', #99703 ) ;
#63554 = CARTESIAN_POINT ( 'NONE',  ( -94.62287095715005592, -24.66019654487199730, 8.947790411086126383 ) ) ;
#63555 = VERTEX_POINT ( 'NONE', #63181 ) ;
#63556 = DIRECTION ( 'NONE',  ( -6.267148949376405333E-16, -1.000000000000000000, 5.583826031377241668E-16 ) ) ;
#63557 = CARTESIAN_POINT ( 'NONE',  ( -104.6228709571500559, -24.65952944569304961, 1.056160979905701236 ) ) ;
#63558 = ORIENTED_EDGE ( 'NONE', *, *, #44533, .T. ) ;
#63559 = ORIENTED_EDGE ( 'NONE', *, *, #35178, .T. ) ;
#63560 = EDGE_LOOP ( 'NONE', ( #17608, #14709, #6777, #2894, #5894 ) ) ;
#63561 = CARTESIAN_POINT ( 'NONE',  ( -111.6379088208709760, -25.24256088085423499, 3.668351635140509881 ) ) ;
#63562 = PLANE ( 'NONE',  #40564 ) ;
#63563 = CARTESIAN_POINT ( 'NONE',  ( 5.786755829966409692, -6.376774720514413630, 19.89762986309224857 ) ) ;
#63564 = CARTESIAN_POINT ( 'NONE',  ( -17.53982812869053731, -11.02811673548155902, -1.500000000000002220 ) ) ;
#63565 = CARTESIAN_POINT ( 'NONE',  ( 10.55456386191721663, 18.89434267519128596, 11.49999999999999645 ) ) ;
#63566 = VERTEX_POINT ( 'NONE', #15480 ) ;
#63567 = CARTESIAN_POINT ( 'NONE',  ( -13.89275734969026388, 0.3587747205144262708, 31.02402280011862246 ) ) ;
#63568 = CARTESIAN_POINT ( 'NONE',  ( -109.6228709571500417, -23.48786465467242124, 11.44779295918253936 ) ) ;
#63569 = CARTESIAN_POINT ( 'NONE',  ( 17.95543856985664277, -13.40637504462900331, -1.500000000000002220 ) ) ;
#63570 = CARTESIAN_POINT ( 'NONE',  ( -47.59344166597622916, -24.15620529776627379, 10.23563542870660825 ) ) ;
#63571 = DIRECTION ( 'NONE',  ( -0.000000000000000000, -1.000000000000000000, 0.000000000000000000 ) ) ;
#63572 = ORIENTED_EDGE ( 'NONE', *, *, #91723, .T. ) ;
#63573 = DIRECTION ( 'NONE',  ( -0.000000000000000000, -1.000000000000000000, 0.000000000000000000 ) ) ;
#63574 = CARTESIAN_POINT ( 'NONE',  ( -120.6228709571501128, -24.63345952396256422, 9.038047939301506517 ) ) ;
#63575 = ORIENTED_EDGE ( 'NONE', *, *, #46217, .T. ) ;
#63576 = VERTEX_POINT ( 'NONE', #86001 ) ;
#63577 = CARTESIAN_POINT ( 'NONE',  ( -39.58953762381673158, -24.66019654487199375, 8.947790411086133489 ) ) ;
#63578 = EDGE_LOOP ( 'NONE', ( #82520, #45990, #61671, #78920 ) ) ;
#63579 = AXIS2_PLACEMENT_3D ( 'NONE', #79922, #57113, #48494 ) ;
#63580 = CARTESIAN_POINT ( 'NONE',  ( -107.6228709571500701, -23.47593901973091235, -1.443836447538999312 ) ) ;
#63581 = CARTESIAN_POINT ( 'NONE',  ( -19.96038302963917488, -7.207760892512529161, -1.500000000000002220 ) ) ;
#63582 = ORIENTED_EDGE ( 'NONE', *, *, #93522, .F. ) ;
#63583 = CARTESIAN_POINT ( 'NONE',  ( -50.59279366430950375, -24.40034930558991277, 0.3402023900116070698 ) ) ;
#63584 = PRODUCT ( 'Hook Pin_Varsay\X2\0131\X0\lan', 'Hook Pin_Varsay\X2\0131\X0\lan', '', ( #58621 ) ) ;
#63585 = CARTESIAN_POINT ( 'NONE',  ( 18.38516380405726736, -11.72527425286322611, -1.500000000000002220 ) ) ;
#63586 = CARTESIAN_POINT ( 'NONE',  ( -103.6288238165831075, -24.15620529776628445, 10.23563542870660292 ) ) ;
#63587 = CARTESIAN_POINT ( 'NONE',  ( 6.955725288069978696, -6.376774720514426065, 21.70430095680336890 ) ) ;
#63588 = CARTESIAN_POINT ( 'NONE',  ( -109.5228709571500616, -24.65952944569305316, 1.056160979905704123 ) ) ;
#63589 = CARTESIAN_POINT ( 'NONE',  ( -20.50126671893153940, -7.481214725051755110, -1.500000000000002220 ) ) ;
#63590 = CARTESIAN_POINT ( 'NONE',  ( 1.542438661763949392, 0.000000000000000000, 0.000000000000000000 ) ) ;
#63591 = ORIENTED_EDGE ( 'NONE', *, *, #6192, .T. ) ;
#63592 = CARTESIAN_POINT ( 'NONE',  ( -20.27875734969026311, 6.143225279485574397, 24.00402280011862288 ) ) ;
#63593 = CARTESIAN_POINT ( 'NONE',  ( -85.52211221999672830, -23.48786465467240703, 11.44779295918254647 ) ) ;
#63594 = ORIENTED_EDGE ( 'NONE', *, *, #47375, .F. ) ;
#63595 = ORIENTED_EDGE ( 'NONE', *, *, #95872, .T. ) ;
#63596 = ORIENTED_EDGE ( 'NONE', *, *, #2700, .T. ) ;
#63597 = DIRECTION ( 'NONE',  ( 3.773278334444167608E-23, -1.000000000000000000, 0.000000000000000000 ) ) ;
#63598 = CARTESIAN_POINT ( 'NONE',  ( -82.50296107429853976, -24.51314013834315375, 0.6176544820404155089 ) ) ;
#63599 = CARTESIAN_POINT ( 'NONE',  ( -7.948041996521916452, 19.69052605537007850, -1.500000000000002220 ) ) ;
#63600 = AXIS2_PLACEMENT_3D ( 'NONE', #40291, #78334, #55022 ) ;
#63601 = CARTESIAN_POINT ( 'NONE',  ( -94.54705908665695802, -24.51314013834316086, 0.6176544820404165081 ) ) ;
#63602 = CARTESIAN_POINT ( 'NONE',  ( -30.60464735295150263, -24.58764167366260622, 9.439037205594624780 ) ) ;
#63603 = EDGE_CURVE ( 'NONE', #97853, #58206, #38822, .T. ) ;
#63604 = CARTESIAN_POINT ( 'NONE',  ( -44.58953762381671737, -23.48786465467240347, 11.44779295918255180 ) ) ;
#63605 = DIRECTION ( 'NONE',  ( 1.000000000000000000, -0.000000000000000000, 0.000000000000000000 ) ) ;
#63606 = CARTESIAN_POINT ( 'NONE',  ( 19.37663158793545293, -0.8356294931911363300, 11.49999999999998934 ) ) ;
#63607 = EDGE_CURVE ( 'NONE', #19596, #35854, #13247, .T. ) ;
#63608 = CARTESIAN_POINT ( 'NONE',  ( -45.47736248591412078, -24.83618233451449697, 1.606449574219536158 ) ) ;
#63609 = ORIENTED_EDGE ( 'NONE', *, *, #43528, .F. ) ;
#63610 = CARTESIAN_POINT ( 'NONE',  ( 7.694069055508638399, 17.95645395709951941, 11.49999999999999645 ) ) ;
#63611 = FACE_OUTER_BOUND ( 'NONE', #68108, .T. ) ;
#63612 = CARTESIAN_POINT ( 'NONE',  ( -68.52287095715006160, -24.64898659630528854, 1.056161002820824368 ) ) ;
#63613 = VERTEX_POINT ( 'NONE', #32206 ) ;
#63614 = CARTESIAN_POINT ( 'NONE',  ( 4.819673832743241348, -6.376774720514422512, 21.07066438048017076 ) ) ;
#63615 = CARTESIAN_POINT ( 'NONE',  ( -51.52764846858840997, -25.24768739062223943, 6.187572788000800017 ) ) ;
#63616 = LINE ( 'NONE', #92532, #50408 ) ;
#63617 = CIRCLE ( 'NONE', #27957, 21.89999999999999858 ) ;
#63618 = CARTESIAN_POINT ( 'NONE',  ( -101.1977347980315329, -25.23200539837010936, 3.666257912286023490 ) ) ;
#63619 = CARTESIAN_POINT ( 'NONE',  ( -19.67010641940559168, 0.002901314006966619011, 11.49999999999998934 ) ) ;
#63620 = B_SPLINE_CURVE_WITH_KNOTS ( 'NONE', 3,
 ( #25236, #93745, #15620, #77512, #56212, #38962 ),
 .UNSPECIFIED., .F., .F.,
 ( 4, 2, 4 ),
 ( 6.384118696083428989E-06, 0.001386860460837108884, 0.002767336802978134086 ),
 .UNSPECIFIED. ) ;
#63622 = ORIENTED_EDGE ( 'NONE', *, *, #81511, .T. ) ;
#63621 = PRODUCT_DEFINITION_FORMATION_WITH_SPECIFIED_SOURCE ( 'ANY', '', #27178, .NOT_KNOWN. ) ;
#63623 = CARTESIAN_POINT ( 'NONE',  ( -90.52287095715001897, -24.15516710230294350, 10.28746687063725851 ) ) ;
#63624 = CARTESIAN_POINT ( 'NONE',  ( -43.58953762381671737, -24.64898659630367206, 1.056161002820379169 ) ) ;
#63625 = ADVANCED_FACE ( 'NONE', ( #262 ), #55566, .F. ) ;
#63626 = VECTOR ( 'NONE', #91782, 1000.000000000000114 ) ;
#63627 = CALENDAR_DATE ( 2026, 9, 10 ) ;
#63628 = CARTESIAN_POINT ( 'NONE',  ( 3.036358173076929123, -5.876774720514419847, 20.87990785256409865 ) ) ;
#63629 = CARTESIAN_POINT ( 'NONE',  ( 4.628547153713393314, -6.376774720514418959, 20.50654586986123817 ) ) ;
#63630 = CARTESIAN_POINT ( 'NONE',  ( -97.51358029338079803, -24.15620529776628800, 10.23563542870660115 ) ) ;
#63631 = CARTESIAN_POINT ( 'NONE',  ( 27.53860345374771867, -2.682774720514426559, -9.482392034746242260 ) ) ;
#63632 = CARTESIAN_POINT ( 'NONE',  ( 5.920986267150416538, -6.376774720514422512, 21.32549308339960348 ) ) ;
#63633 = CARTESIAN_POINT ( 'NONE',  ( -129.5557419245657513, -24.51314013834316796, 0.6176544820404223923 ) ) ;
#63634 = CIRCLE ( 'NONE', #86284, 2.399999999999999911 ) ;
#63635 = CARTESIAN_POINT ( 'NONE',  ( -114.5930451687649168, -23.73791477778912551, 11.05961554403169878 ) ) ;
#63636 = CARTESIAN_POINT ( 'NONE',  ( -12.53609265798794681, -15.47265773855268378, 11.49999999999998934 ) ) ;
#63637 = CARTESIAN_POINT ( 'NONE',  ( -75.62719797981144154, -24.83644354573578994, 8.397322867130100121 ) ) ;
#63638 = CARTESIAN_POINT ( 'NONE',  ( -19.78623529325263775, -1.157695164950638844, -1.500000000000002220 ) ) ;
#63639 = ORIENTED_EDGE ( 'NONE', *, *, #76912, .F. ) ;
#63640 = CARTESIAN_POINT ( 'NONE',  ( -90.25931493494785229, -25.32787839792626627, 4.644810655877241956 ) ) ;
#63641 = CARTESIAN_POINT ( 'NONE',  ( -104.6228709571500417, -23.72773821059535848, 11.05748984161097503 ) ) ;
#63642 = CARTESIAN_POINT ( 'NONE',  ( -95.52287095715004739, -23.47593901973090169, -1.443836447538996648 ) ) ;
#63643 = CARTESIAN_POINT ( 'NONE',  ( -4.968023186724614959, -20.10795263665959709, 11.49999999999999645 ) ) ;
#63644 = DIRECTION ( 'NONE',  ( 1.000000000000000000, 3.773278334444167608E-23, 8.201307816334959825E-29 ) ) ;
#63645 = CARTESIAN_POINT ( 'NONE',  ( -126.5228709571500616, -24.64898659630368627, 1.056161002820834804 ) ) ;
#63646 = CARTESIAN_POINT ( 'NONE',  ( 4.306090731860143350, 22.38281141545218844, 11.49999999999999645 ) ) ;
#63647 = AXIS2_PLACEMENT_3D ( 'NONE', #62987, #16786, #64504 ) ;
#63648 = B_SPLINE_CURVE_WITH_KNOTS ( 'NONE', 3,
 ( #85999, #9369, #62178, #63690 ),
 .UNSPECIFIED., .F., .F.,
 ( 4, 4 ),
 ( 0.3089841683514000792, 0.3099849153921654943 ),
 .UNSPECIFIED. ) ;
#63649 = ORIENTED_EDGE ( 'NONE', *, *, #13469, .T. ) ;
#63650 = B_SPLINE_SURFACE_WITH_KNOTS ( 'NONE', 3, 3, ( 
 ( #45931, #44937, #60168, #61660 ),
 ( #5859, #36816, #75859, #6854 ),
 ( #30183, #77349, #7343, #38298 ),
 ( #69254, #91090, #13961, #13461 ),
 ( #92578, #6362, #38798, #100173 ),
 ( #37319, #52538, #31182, #93079 ),
 ( #23564, #82971, #44435, #87478 ) ),
 .UNSPECIFIED., .F., .F., .F.,
 ( 4, 3, 4 ),
 ( 4, 4 ),
 ( 0.0004766839783823623123, 0.1029713700210900668, 0.2054660560637977806 ),
 ( 0.06951167983181827381, 0.07055647694920491597 ),
 .UNSPECIFIED. ) ;
#63651 = CARTESIAN_POINT ( 'NONE',  ( -69.59246360937903830, -24.15543982623907127, -0.2315651400026648155 ) ) ;
#63652 = FACE_OUTER_BOUND ( 'NONE', #48094, .T. ) ;
#63653 = EDGE_LOOP ( 'NONE', ( #84986, #95287, #79094, #50544 ) ) ;
#63654 = CARTESIAN_POINT ( 'NONE',  ( -20.14672940031187665, -1.731937678239350298, -1.500000000000002220 ) ) ;
#63655 = B_SPLINE_CURVE_WITH_KNOTS ( 'NONE', 3,
 ( #52882, #37148, #68111, #77191 ),
 .UNSPECIFIED., .F., .F.,
 ( 4, 4 ),
 ( 0.000000000000000000, 9.999999999997510880E-05 ),
 .UNSPECIFIED. ) ;
#63656 = LINE ( 'NONE', #40795, #22526 ) ;
#63657 = DIRECTION ( 'NONE',  ( -0.000000000000000000, -1.000000000000000000, -0.000000000000000000 ) ) ;
#63658 = EDGE_CURVE ( 'NONE', #28945, #58432, #23585, .T. ) ;
#63659 = ADVANCED_FACE ( 'NONE', ( #94105 ), #77373, .F. ) ;
#63660 = VERTEX_POINT ( 'NONE', #30716 ) ;
#63661 = DIRECTION ( 'NONE',  ( -1.000000000000000000, -3.773278334444167608E-23, -8.201307833595939069E-29 ) ) ;
#63662 = CARTESIAN_POINT ( 'NONE',  ( -14.98413761715186077, 17.36544542080599740, -1.500000000000002220 ) ) ;
#63663 = CARTESIAN_POINT ( 'NONE',  ( -10.21560369921944833, 5.622950887248190810, 29.47514638292475553 ) ) ;
#63664 = CARTESIAN_POINT ( 'NONE',  ( 11.47056939498152950, -16.38825109899074661, -1.500000000000002220 ) ) ;
#63665 = CARTESIAN_POINT ( 'NONE',  ( -41.26959558397307148, -25.08918874615346439, 7.338714959427068862 ) ) ;
#63666 = AXIS2_PLACEMENT_3D ( 'NONE', #35785, #57140, #26675 ) ;
#63667 = EDGE_CURVE ( 'NONE', #38147, #68993, #23081, .T. ) ;
#63668 = CARTESIAN_POINT ( 'NONE',  ( 10.03794737889396771, 18.37758748099471973, 11.49999999999999645 ) ) ;
#63669 = CARTESIAN_POINT ( 'NONE',  ( -28.89996118126751767, -24.85249319229149023, 7.829856784274641157 ) ) ;
#63670 = FACE_OUTER_BOUND ( 'NONE', #8509, .T. ) ;
#63671 = CARTESIAN_POINT ( 'NONE',  ( -5.561696574893697509, -21.35426480686918538, 11.49999999999998934 ) ) ;
#63672 = EDGE_CURVE ( 'NONE', #65405, #47332, #7874, .T. ) ;
#63673 = B_SPLINE_CURVE_WITH_KNOTS ( 'NONE', 3,
 ( #14853, #7241, #85367, #38192 ),
 .UNSPECIFIED., .F., .F.,
 ( 4, 4 ),
 ( 2.775557561562891351E-17, 9.999999999998898659E-05 ),
 .UNSPECIFIED. ) ;
#63674 = CARTESIAN_POINT ( 'NONE',  ( -19.69812919673063689, -5.965225279485592225, -22.00173861453435720 ) ) ;
#63675 = ORIENTED_EDGE ( 'NONE', *, *, #533, .F. ) ;
#63676 = CARTESIAN_POINT ( 'NONE',  ( -60.52287095715006870, -24.62226745350439217, 0.9660975649728013037 ) ) ;
#63677 = CARTESIAN_POINT ( 'NONE',  ( -49.73776537321236901, -25.27344806511582576, 3.509878174495147274 ) ) ;
#63678 = DIRECTION ( 'NONE',  ( 0.000000000000000000, 0.000000000000000000, 1.000000000000000000 ) ) ;
#63679 = ORIENTED_EDGE ( 'NONE', *, *, #53856, .T. ) ;
#63680 = CARTESIAN_POINT ( 'NONE',  ( 33.96422015159436114, 5.965225279485572685, -7.233236000911337449 ) ) ;
#63681 = ORIENTED_EDGE ( 'NONE', *, *, #89345, .T. ) ;
#63682 = VERTEX_POINT ( 'NONE', #85494 ) ;
#63683 = CARTESIAN_POINT ( 'NONE',  ( 6.660000000000001030, -10.98394470431085601, -0.7905513910579705650 ) ) ;
#63684 = CARTESIAN_POINT ( 'NONE',  ( -100.4784170818037552, -25.10935802628761948, 2.833156094507327083 ) ) ;
#63686 = EDGE_CURVE ( 'NONE', #53182, #77233, #16841, .T. ) ;
#63685 = CARTESIAN_POINT ( 'NONE',  ( -90.70643023311484399, -25.31959457942835456, 5.296252855621696121 ) ) ;
#63687 = CARTESIAN_POINT ( 'NONE',  ( 3.262959013008915665, -20.29835246810489835, -1.500000000000002220 ) ) ;
#63688 = B_SPLINE_CURVE_WITH_KNOTS ( 'NONE', 3,
 ( #43560, #26831, #89733, #33948, #74497, #4504, #4991, #88740 ),
 .UNSPECIFIED., .F., .F.,
 ( 4, 2, 2, 4 ),
 ( 0.000000000000000000, 0.002001098010032801612, 0.003001647015049202418, 0.004002196020065603224 ),
 .UNSPECIFIED. ) ;
#63689 = ORIENTED_EDGE ( 'NONE', *, *, #100021, .T. ) ;
#63690 = CARTESIAN_POINT ( 'NONE',  ( -61.62287095715004881, -23.47596703998600631, 11.44779298504227505 ) ) ;
#63691 = CARTESIAN_POINT ( 'NONE',  ( -44.48280314835779592, -24.65952944569304606, 1.056160979905693909 ) ) ;
#63692 = CARTESIAN_POINT ( 'NONE',  ( 21.57151214508649772, -9.529487854913506695, -1.500000000000000666 ) ) ;
#63693 = CARTESIAN_POINT ( 'NONE',  ( -20.85237562250380350, -7.973873963886685345, -1.500000000000002220 ) ) ;
#63694 = B_SPLINE_CURVE_WITH_KNOTS ( 'NONE', 3,
 ( #12042, #43012, #87680, #4450 ),
 .UNSPECIFIED., .F., .F.,
 ( 4, 4 ),
 ( 0.8511077552149090009, 0.8601141864870244236 ),
 .UNSPECIFIED. ) ;
#63696 = CARTESIAN_POINT ( 'NONE',  ( -0.008164624327092535883, -22.94430252198347020, 6.147794833475638043 ) ) ;
#63695 = AXIS2_PLACEMENT_3D ( 'NONE', #33662, #85065, #38394 ) ;
#63697 = PLANE ( 'NONE',  #25308 ) ;
#63698 = EDGE_LOOP ( 'NONE', ( #52109, #46814 ) ) ;
#63699 = LINE ( 'NONE', #69790, #77569 ) ;
#63700 = CARTESIAN_POINT ( 'NONE',  ( -124.6228709571500559, -24.64898659630368627, 1.056161002820833028 ) ) ;
#63701 = APPROVAL_PERSON_ORGANIZATION ( #49537, #61786, #64273 ) ;
#63702 = CARTESIAN_POINT ( 'NONE',  ( 3.748101851616784774, 20.49759516964078188, -1.500000000000002220 ) ) ;
#63703 = ORIENTED_EDGE ( 'NONE', *, *, #10083, .F. ) ;
#63705 = EDGE_LOOP ( 'NONE', ( #77860, #29954, #10983 ) ) ;
#63704 = CARTESIAN_POINT ( 'NONE',  ( -52.52287095715004739, -23.73907113217698495, -1.053371485780741024 ) ) ;
#63706 = ORIENTED_EDGE ( 'NONE', *, *, #11451, .F. ) ;
#63707 = VECTOR ( 'NONE', #98288, 1000.000000000000114 ) ;
#63708 = CARTESIAN_POINT ( 'NONE',  ( -69.33560399441930144, -25.03149286552998376, 7.166139700104196208 ) ) ;
#63709 = CARTESIAN_POINT ( 'NONE',  ( -13.06023916655064276, -16.53025015627232719, -1.500000000000002220 ) ) ;
#63710 = ORIENTED_EDGE ( 'NONE', *, *, #91528, .F. ) ;
#63711 = CARTESIAN_POINT ( 'NONE',  ( -37.58953762381673158, -24.64965694238406968, 8.947790433994661896 ) ) ;
#63712 = CARTESIAN_POINT ( 'NONE',  ( -37.52287095715009713, -23.95044443724992789, 10.65354141964649237 ) ) ;
#63713 = PLANE ( 'NONE',  #93446 ) ;
#63714 = VECTOR ( 'NONE', #99838, 1000.000000000000000 ) ;
#63715 = CARTESIAN_POINT ( 'NONE',  ( -86.50735162477467100, -24.35071581493543391, 9.817618358456027039 ) ) ;
#63716 = DIRECTION ( 'NONE',  ( -3.773278334444166432E-23, 1.000000000000000000, 0.000000000000000000 ) ) ;
#63717 = DIRECTION ( 'NONE',  ( -3.773278334453079030E-23, 0.9999999999976377785, 2.173523156925979128E-06 ) ) ;
#63718 = DIRECTION ( 'NONE',  ( 0.000000000000000000, 0.000000000000000000, -1.000000000000000000 ) ) ;
#63720 = ORIENTED_EDGE ( 'NONE', *, *, #20454, .T. ) ;
#63719 = CARTESIAN_POINT ( 'NONE',  ( 13.39142644571787422, -17.71860720625715757, 11.49999999999999645 ) ) ;
#63721 = DIRECTION ( 'NONE',  ( 0.000000000000000000, -0.000000000000000000, -1.000000000000000000 ) ) ;
#63722 = DIRECTION ( 'NONE',  ( -1.226388327005079762E-16, 0.000000000000000000, 1.000000000000000000 ) ) ;
#63723 = ORIENTED_EDGE ( 'NONE', *, *, #67809, .F. ) ;
#63724 = CARTESIAN_POINT ( 'NONE',  ( -12.60694655700363143, 18.86142483545513926, -1.500000000000002220 ) ) ;
#63726 = EDGE_LOOP ( 'NONE', ( #90403, #5034, #28699, #81005 ) ) ;
#63725 = CARTESIAN_POINT ( 'NONE',  ( -118.6228709571500275, -23.72773821059536559, 11.05748984161097681 ) ) ;
#63727 = EDGE_CURVE ( 'NONE', #34154, #48223, #35011, .T. ) ;
#63728 = EDGE_LOOP ( 'NONE', ( #29617, #99179, #45810, #86426 ) ) ;
#63729 = CARTESIAN_POINT ( 'NONE',  ( 32.33217928425156629, 6.475225279485573360, -12.20610769812808982 ) ) ;
#63730 = ADVANCED_FACE ( 'NONE', ( #93181 ), #53647, .F. ) ;
#63731 = CARTESIAN_POINT ( 'NONE',  ( 13.66866334921533799, -14.80927461459226890, -1.500000000000002220 ) ) ;
#63732 = B_SPLINE_CURVE_WITH_KNOTS ( 'NONE', 3,
 ( #37007, #98896, #29390, #91293 ),
 .UNSPECIFIED., .F., .F.,
 ( 4, 4 ),
 ( 0.000000000000000000, 9.999999999996123101E-05 ),
 .UNSPECIFIED. ) ;
#63733 = CARTESIAN_POINT ( 'NONE',  ( -83.62287095715007013, -23.47596703998600631, 11.44779298504227860 ) ) ;
#63734 = ORIENTED_EDGE ( 'NONE', *, *, #34691, .T. ) ;
#63735 = CARTESIAN_POINT ( 'NONE',  ( -0.02075734969026423599, -5.965225279485572685, -0.08597719988137648983 ) ) ;
#63736 = CARTESIAN_POINT ( 'NONE',  ( -22.41777205227948855, 0.6913007675000180097, -1.500000000000002220 ) ) ;
#63737 = ORIENTED_EDGE ( 'NONE', *, *, #44083, .F. ) ;
#63738 = EDGE_LOOP ( 'NONE', ( #26734, #21698, #49571, #55385 ) ) ;
#63739 = FACE_OUTER_BOUND ( 'NONE', #86030, .T. ) ;
#63741 = CARTESIAN_POINT ( 'NONE',  ( -48.58953762381672448, -24.66019654487199375, 8.947790411086138818 ) ) ;
#63740 = AXIS2_PLACEMENT_3D ( 'NONE', #57840, #89271, #82154 ) ;
#63742 = LINE ( 'NONE', #40876, #58750 ) ;
#63743 = DIRECTION ( 'NONE',  ( -3.773278334453079030E-23, 0.9999999999976377785, 2.173523156925979128E-06 ) ) ;
#63744 = CARTESIAN_POINT ( 'NONE',  ( 18.72495633783376334, -0.5000000000000000000, 2.346898003627108320 ) ) ;
#63745 = CARTESIAN_POINT ( 'NONE',  ( -16.13938233076020268, 11.07636124087057183, -1.500000000000002220 ) ) ;
#63746 = VECTOR ( 'NONE', #5460, 1000.000000000000000 ) ;
#63747 = DIRECTION ( 'NONE',  ( 0.000000000000000000, -2.173523156925980399E-06, 0.9999999999976378895 ) ) ;
#63748 = ORIENTED_EDGE ( 'NONE', *, *, #62866, .F. ) ;
#63749 = CARTESIAN_POINT ( 'NONE',  ( 11.78165356204951131, -17.99452314462042324, 11.49999999999998934 ) ) ;
#63750 = CARTESIAN_POINT ( 'NONE',  ( -94.62287095715005592, -29.50248528299804818, 1.056150453629040253 ) ) ;
#63751 = CARTESIAN_POINT ( 'NONE',  ( 9.071512145086499501, -1.000000000000000000, 7.567128810856562637 ) ) ;
#63752 = CARTESIAN_POINT ( 'NONE',  ( -26.91814428177455909, -0.3587747205144265483, 29.98490496616818746 ) ) ;
#63753 = CARTESIAN_POINT ( 'NONE',  ( -80.62287095715001328, -24.14406661707769075, 10.28769366152060627 ) ) ;
#63754 = CARTESIAN_POINT ( 'NONE',  ( 22.43992371924722917, 4.826111843257130829, -1.500000000000002220 ) ) ;
#63755 = CC_DESIGN_PERSON_AND_ORGANIZATION_ASSIGNMENT ( #75435, #70846, ( #42576 ) ) ;
#63756 = APPROVAL_ROLE ( '' ) ;
#63757 = CARTESIAN_POINT ( 'NONE',  ( -27.25988310792305214, 5.965225279485572685, 30.32664379231667695 ) ) ;
#63758 = DIRECTION ( 'NONE',  ( 0.000000000000000000, -2.173523156925980399E-06, 0.9999999999976378895 ) ) ;
#63759 = CARTESIAN_POINT ( 'NONE',  ( 17.67427751897593069, 9.450557017276361549, 11.49999999999999645 ) ) ;
#63760 = CARTESIAN_POINT ( 'NONE',  ( 27.53860345374808105, -4.772774720514425972, -6.982392034746241372 ) ) ;
#63761 = CARTESIAN_POINT ( 'NONE',  ( -113.5895376238167245, -24.64965694238408034, 8.947790433994653014 ) ) ;
#63762 = CARTESIAN_POINT ( 'NONE',  ( -46.52287095715004028, -23.73907113216989373, -1.053371485793254125 ) ) ;
#63763 = FACE_OUTER_BOUND ( 'NONE', #33953, .T. ) ;
#63764 = CARTESIAN_POINT ( 'NONE',  ( -85.62287095715011276, -24.82558206586144323, 1.605769216559442158 ) ) ;
#63765 = CARTESIAN_POINT ( 'NONE',  ( 19.41305359857673096, 4.112862643401165919, -1.500000000000002220 ) ) ;
#63766 = CARTESIAN_POINT ( 'NONE',  ( -17.16505717403991227, -13.39166244882208012, 11.49999999999998934 ) ) ;
#63767 = EDGE_CURVE ( 'NONE', #44470, #84523, #85858, .T. ) ;
#63768 = LINE ( 'NONE', #17564, #72318 ) ;
#63769 = CARTESIAN_POINT ( 'NONE',  ( -15.16444148636751521, -12.51942901160708921, -1.500000000000002220 ) ) ;
#63770 = CARTESIAN_POINT ( 'NONE',  ( 11.05000000000000426, -2.000000000000000888, 19.19609335255483629 ) ) ;
#63771 = AXIS2_PLACEMENT_3D ( 'NONE', #79290, #15890, #63597 ) ;
#63772 = CARTESIAN_POINT ( 'NONE',  ( -32.52287095715004739, -23.47593901973090169, -1.443836447538997092 ) ) ;
#63773 = CONTEXT_DEPENDENT_SHAPE_REPRESENTATION ( #53091, #74173 ) ;
#63774 = CARTESIAN_POINT ( 'NONE',  ( 14.43441820105630136, 3.540887625665272598, -28.36222020492957796 ) ) ;
#63775 = CARTESIAN_POINT ( 'NONE',  ( 2.649863049427662709, -6.376774720514420736, 20.71861240329949538 ) ) ;
#63776 = CARTESIAN_POINT ( 'NONE',  ( 20.53815866822273861, -0.6333348845813139283, 11.49999999999999645 ) ) ;
#63777 = CARTESIAN_POINT ( 'NONE',  ( 32.45853543194704116, -0.3587747205144265483, 9.169203677920338080 ) ) ;
#63778 = CARTESIAN_POINT ( 'NONE',  ( -120.6279586782334405, -23.85016227208581441, -0.8807180028928249804 ) ) ;
#63779 = VECTOR ( 'NONE', #21415, 1000.000000000000000 ) ;
#63780 = CARTESIAN_POINT ( 'NONE',  ( -21.70561270324154179, 6.225854807558039994, 11.49999999999999645 ) ) ;
#63781 = ORIENTED_EDGE ( 'NONE', *, *, #91916, .F. ) ;
#63782 = CARTESIAN_POINT ( 'NONE',  ( -70.32380231474228083, -25.25639601488367703, 7.101635269074562551 ) ) ;
#63783 = DIRECTION ( 'NONE',  ( -1.000000000000000000, -0.000000000000000000, 0.000000000000000000 ) ) ;
#63784 = DIRECTION ( 'NONE',  ( -0.1254312216594016538, -0.000000000000000000, -0.9921023176230513441 ) ) ;
#63785 = CARTESIAN_POINT ( 'NONE',  ( -72.62287095715007013, -24.33927499327854704, 9.819080762295818943 ) ) ;
#63786 = AXIS2_PLACEMENT_3D ( 'NONE', #69580, #63, #96913 ) ;
#63787 = ADVANCED_FACE ( 'NONE', ( #76951 ), #70866, .F. ) ;
#63788 = CARTESIAN_POINT ( 'NONE',  ( -25.68888630310901178, -24.61459721658222222, 6.447530656637062485 ) ) ;
#63789 = DIRECTION ( 'NONE',  ( 0.5646109999446368155, 0.000000000000000000, -0.8253571461746226356 ) ) ;
#63790 = VERTEX_POINT ( 'NONE', #55145 ) ;
#63791 = CARTESIAN_POINT ( 'NONE',  ( 22.67273400128462058, 4.441195646929153362, 11.49999999999999645 ) ) ;
#63792 = CARTESIAN_POINT ( 'NONE',  ( 9.452765381649220089, 20.79790602042944414, -1.500000000000002220 ) ) ;
#63793 = CARTESIAN_POINT ( 'NONE',  ( -41.32836283488544638, 5.356774720514427379, 39.26872235229541985 ) ) ;
#63794 = DIRECTION ( 'NONE',  ( 0.000000000000000000, 2.173523156925980399E-06, -0.9999999999976378895 ) ) ;
#63795 = CARTESIAN_POINT ( 'NONE',  ( -82.62360247695944793, -24.66019654487199730, 8.947790411086122830 ) ) ;
#63796 = ADVANCED_FACE ( 'NONE', ( #8455 ), #6977, .T. ) ;
#63797 = CARTESIAN_POINT ( 'NONE',  ( -18.88510386880526326, 12.19974334031638641, 11.49999999999999645 ) ) ;
#63798 = ORIENTED_EDGE ( 'NONE', *, *, #51458, .T. ) ;
#63799 = LINE ( 'NONE', #25198, #23840 ) ;
#63800 = CARTESIAN_POINT ( 'NONE',  ( 21.92589416912191069, -1.073809401359021143, 11.49999999999998934 ) ) ;
#63801 = ADVANCED_FACE ( 'NONE', ( #9454 ), #40411, .F. ) ;
#63802 = CARTESIAN_POINT ( 'NONE',  ( -124.4728709571500360, -25.40558663563427189, 5.000950442582704270 ) ) ;
#63803 = CARTESIAN_POINT ( 'NONE',  ( -34.64252832595930442, -24.15620529776627379, 10.23563542870661003 ) ) ;
#63804 = DIRECTION ( 'NONE',  ( -0.9890158633619159367, -0.1478094111296165969, 0.000000000000000000 ) ) ;
#63805 = VERTEX_POINT ( 'NONE', #43782 ) ;
#63806 = CARTESIAN_POINT ( 'NONE',  ( -64.62287095715005592, -24.64898659630528499, 1.056161002820822592 ) ) ;
#63807 = DIRECTION ( 'NONE',  ( -0.000000000000000000, -1.000000000000000000, -0.000000000000000000 ) ) ;
#63808 = ORIENTED_EDGE ( 'NONE', *, *, #10142, .T. ) ;
#63809 = CARTESIAN_POINT ( 'NONE',  ( -18.82070947631147106, 8.064391923812276985, -1.500000000000002220 ) ) ;
#63810 = ORIENTED_EDGE ( 'NONE', *, *, #30203, .T. ) ;
#63811 = EDGE_LOOP ( 'NONE', ( #42595, #76507, #12383, #74169 ) ) ;
#63812 = ORIENTED_EDGE ( 'NONE', *, *, #53240, .F. ) ;
#63813 = EDGE_LOOP ( 'NONE', ( #3295, #67689, #94384, #95005 ) ) ;
#63814 = CARTESIAN_POINT ( 'NONE',  ( 13.31140876108729998, -18.89465134148960956, 11.49999999999998934 ) ) ;
#63816 = EDGE_CURVE ( 'NONE', #69079, #44339, #28056, .T. ) ;
#63815 = PLANE ( 'NONE',  #3369 ) ;
#63817 = CARTESIAN_POINT ( 'NONE',  ( 15.76184642470745700, 12.85868457875834103, -1.500000000000002220 ) ) ;
#63818 = VECTOR ( 'NONE', #58585, 1000.000000000000000 ) ;
#63819 = ORIENTED_EDGE ( 'NONE', *, *, #8693, .F. ) ;
#63820 = CARTESIAN_POINT ( 'NONE',  ( -103.6228709571500559, -29.50250243563736774, 8.947779886222138046 ) ) ;
#63821 = CARTESIAN_POINT ( 'NONE',  ( -24.90875734969025501, -5.965225279485572685, 30.00402280011862288 ) ) ;
#63822 = CARTESIAN_POINT ( 'NONE',  ( -44.52287095715007581, -24.66019654487199730, 8.947790411086117501 ) ) ;
#63823 = CARTESIAN_POINT ( 'NONE',  ( 4.547289707988324103, -6.376774720514410077, 19.12266226838056582 ) ) ;
#63825 = ORIENTED_EDGE ( 'NONE', *, *, #71348, .F. ) ;
#63824 = CARTESIAN_POINT ( 'NONE',  ( 2.564635614221720594, -21.35862533600356983, 11.49999999999999645 ) ) ;
#63826 = CARTESIAN_POINT ( 'NONE',  ( -75.54455309653219786, -24.52300882791530157, 0.6510814631126414787 ) ) ;
#63827 = B_SPLINE_CURVE_WITH_KNOTS ( 'NONE', 3,
 ( #46303, #77230, #7738, #62039, #92965, #23440, #626, #2646 ),
 .UNSPECIFIED., .F., .F.,
 ( 4, 2, 2, 4 ),
 ( -0.001224554619866348015, -0.0002241820295893657503, 0.0007761905606876165140, 0.002776935741241576706 ),
 .UNSPECIFIED. ) ;
#63829 = CIRCLE ( 'NONE', #20040, 0.3000000000000016542 ) ;
#63828 = LINE ( 'NONE', #48595, #36120 ) ;
#63830 = EDGE_LOOP ( 'NONE', ( #7627, #71400, #57011, #70498 ) ) ;
#63831 = CARTESIAN_POINT ( 'NONE',  ( 12.20387445076365296, 16.77033177596414504, -1.500000000000002220 ) ) ;
#63832 = ORIENTED_EDGE ( 'NONE', *, *, #55520, .T. ) ;
#63834 = ORIENTED_EDGE ( 'NONE', *, *, #80825, .T. ) ;
#63833 = CARTESIAN_POINT ( 'NONE',  ( 29.70220533433691301, 3.316774720514426456, 28.20564067601639735 ) ) ;
#63835 = DIRECTION ( 'NONE',  ( 0.000000000000000000, -1.000000000000000000, 0.000000000000000000 ) ) ;
#63836 = CARTESIAN_POINT ( 'NONE',  ( -129.6228709571500417, -23.47596703998600631, 11.44779298504227683 ) ) ;
#63837 = VERTEX_POINT ( 'NONE', #95194 ) ;
#63838 = ORIENTED_EDGE ( 'NONE', *, *, #53083, .F. ) ;
#63839 = CARTESIAN_POINT ( 'NONE',  ( -28.55620429048338949, -24.50218025470241301, 8.947790429581973015 ) ) ;
#63840 = CARTESIAN_POINT ( 'NONE',  ( -42.48186235109157138, -24.66019654487198665, 8.947790411086131712 ) ) ;
#63841 = CARTESIAN_POINT ( 'NONE',  ( -65.62287095715005592, -24.99132157543084176, 2.256160258750667502 ) ) ;
#63843 = ORIENTED_EDGE ( 'NONE', *, *, #56096, .F. ) ;
#63842 = CARTESIAN_POINT ( 'NONE',  ( 21.52718982488130450, -4.553922534329950089, 11.49999999999999645 ) ) ;
#63844 = CARTESIAN_POINT ( 'NONE',  ( -103.5888980205460257, -24.34968618360933945, 0.1864209137778842229 ) ) ;
#63845 = CARTESIAN_POINT ( 'NONE',  ( -16.99934442671578694, -14.85117937636706031, -1.500000000000002220 ) ) ;
#63846 = CARTESIAN_POINT ( 'NONE',  ( 17.27681320446407298, 11.92757687370068886, 11.49999999999998934 ) ) ;
#63848 = VERTEX_POINT ( 'NONE', #74709 ) ;
#63847 = FACE_OUTER_BOUND ( 'NONE', #47298, .T. ) ;
#63849 = EDGE_LOOP ( 'NONE', ( #56583, #4506, #89198, #70628 ) ) ;
#63850 = DIRECTION ( 'NONE',  ( -0.000000000000000000, -1.000000000000000000, -0.000000000000000000 ) ) ;
#63851 = CIRCLE ( 'NONE', #18409, 4.080000000000000071 ) ;
#63852 = EDGE_CURVE ( 'NONE', #29304, #92190, #14280, .T. ) ;
#63853 = CARTESIAN_POINT ( 'NONE',  ( -57.62367090558025495, -24.66019654487199375, 8.947790411086119278 ) ) ;
#63854 = ORIENTED_EDGE ( 'NONE', *, *, #20908, .F. ) ;
#63855 = CARTESIAN_POINT ( 'NONE',  ( 16.66693084842116335, 13.01107939256401913, 11.49999999999998934 ) ) ;
#63856 = CARTESIAN_POINT ( 'NONE',  ( -82.62287095715005592, -24.65952944569304606, 1.056160979905699016 ) ) ;
#63857 = CARTESIAN_POINT ( 'NONE',  ( -59.79157152756309301, -25.29489609436097552, 6.057563354383566967 ) ) ;
#63858 = CARTESIAN_POINT ( 'NONE',  ( -75.62287095715008434, -24.62226745350437440, 0.9660975649728090753 ) ) ;
#63859 = CARTESIAN_POINT ( 'NONE',  ( -6.752792875861700850, -6.376774720514411854, 19.46247113826586528 ) ) ;
#63860 = CARTESIAN_POINT ( 'NONE',  ( -101.5228709571500900, -23.48783264082477018, -1.443836473390087249 ) ) ;
#63861 = CARTESIAN_POINT ( 'NONE',  ( 17.07819277939130842, -14.19623557145530057, -1.500000000000002220 ) ) ;
#63862 = VECTOR ( 'NONE', #64379, 1000.000000000000114 ) ;
#63863 = CARTESIAN_POINT ( 'NONE',  ( -114.5930436926616949, -23.73766607897672287, -1.055555164236428700 ) ) ;
#63864 = B_SPLINE_CURVE_WITH_KNOTS ( 'NONE', 3,
 ( #97906, #66993, #20778, #7067, #67984, #99408 ),
 .UNSPECIFIED., .F., .F.,
 ( 4, 2, 4 ),
 ( 0.000000000000000000, 0.001380764517854763014, 0.002761529035709526028 ),
 .UNSPECIFIED. ) ;
#63865 = ORIENTED_EDGE ( 'NONE', *, *, #80626, .T. ) ;
#63866 = CARTESIAN_POINT ( 'NONE',  ( -2.749999999999999112, 26.59999999999999432, 2.100000000000000089 ) ) ;
#63867 = CARTESIAN_POINT ( 'NONE',  ( -58.52287095715006160, -23.47596703998600631, 11.44779298504228926 ) ) ;
#63868 = CARTESIAN_POINT ( 'NONE',  ( -126.5218661376151488, -23.73766607897670511, -1.055555164236450238 ) ) ;
#63869 = CARTESIAN_POINT ( 'NONE',  ( -36.62372838562182409, -24.66019654487199730, 8.947790411086113949 ) ) ;
#63870 = CARTESIAN_POINT ( 'NONE',  ( 0.2958748881272694198, 19.47992435465491212, 11.49999999999998934 ) ) ;
#63871 = CARTESIAN_POINT ( 'NONE',  ( -16.30254408640404051, -13.89340296626662230, -1.500000000000002220 ) ) ;
#63872 = CARTESIAN_POINT ( 'NONE',  ( -85.52287095715006160, -23.47596703998600631, 11.44779298504228393 ) ) ;
#63873 = DIRECTION ( 'NONE',  ( -1.000000000000000000, -3.773278334444167608E-23, -8.201307833595939069E-29 ) ) ;
#63874 = CARTESIAN_POINT ( 'NONE',  ( -51.60611487679543785, -23.73766607897669445, -1.055555164236457788 ) ) ;
#63875 = CARTESIAN_POINT ( 'NONE',  ( -77.60072041985134206, -23.73766607897670156, -1.055555164236459564 ) ) ;
#63876 = CARTESIAN_POINT ( 'NONE',  ( 22.69831151501224298, -1.600861625767590724, -1.500000000000002220 ) ) ;
#63877 = B_SPLINE_CURVE_WITH_KNOTS ( 'NONE', 3,
 ( #45577, #7496, #66924, #97843 ),
 .UNSPECIFIED., .F., .F.,
 ( 4, 4 ),
 ( 0.000000000000000000, 9.999999999998897304E-05 ),
 .UNSPECIFIED. ) ;
#63878 = EDGE_CURVE ( 'NONE', #12512, #41731, #72581, .T. ) ;
#63879 = CARTESIAN_POINT ( 'NONE',  ( -106.5486680884517199, -24.66019654487200441, 8.947790411086108620 ) ) ;
#63880 = DIRECTION ( 'NONE',  ( 0.000000000000000000, 0.000000000000000000, -1.000000000000000000 ) ) ;
#63881 = CARTESIAN_POINT ( 'NONE',  ( 3.337697395173636394, -19.57427954046807983, 11.49999999999999645 ) ) ;
#63882 = CARTESIAN_POINT ( 'NONE',  ( 5.557675543255346184, -6.376774720514415407, 20.10561748372801461 ) ) ;
#63883 = EDGE_CURVE ( 'NONE', #92103, #5494, #92075, .T. ) ;
#63884 = CARTESIAN_POINT ( 'NONE',  ( -103.5228709571500758, -24.64898659630367916, 1.056161002820829697 ) ) ;
#63885 = CARTESIAN_POINT ( 'NONE',  ( 0.000000000000000000, -5.876774720514426953, 0.000000000000000000 ) ) ;
#63886 = EDGE_LOOP ( 'NONE', ( #72256, #17365, #16022, #80883 ) ) ;
#63887 = CARTESIAN_POINT ( 'NONE',  ( -49.40445554211785151, -25.19972462862641294, 6.604535875143222157 ) ) ;
#63888 = CARTESIAN_POINT ( 'NONE',  ( 11.05000000000000426, -14.50000000000000178, 11.24599928863593767 ) ) ;
#63889 = VECTOR ( 'NONE', #66418, 1000.000000000000114 ) ;
#63890 = CARTESIAN_POINT ( 'NONE',  ( -63.52287095715006160, -23.48786465467241058, 11.44779295918254824 ) ) ;
#63891 = CARTESIAN_POINT ( 'NONE',  ( -20.76051858633888259, -6.224802954461835292, 11.49999999999998934 ) ) ;
#63892 = EDGE_CURVE ( 'NONE', #57483, #88037, #25172, .T. ) ;
#63893 = CARTESIAN_POINT ( 'NONE',  ( -50.88999612354844970, -25.05389627988721202, 7.512545578324246520 ) ) ;
#63894 = CARTESIAN_POINT ( 'NONE',  ( -19.16120753946698585, -3.443109951913609024, -1.500000000000002220 ) ) ;
#63895 = EDGE_CURVE ( 'NONE', #78402, #24307, #35670, .T. ) ;
#63896 = CARTESIAN_POINT ( 'NONE',  ( -55.57991466617167475, -24.83644354573578283, 8.397322867130093016 ) ) ;
#63897 = B_SPLINE_CURVE_WITH_KNOTS ( 'NONE', 3,
 ( #63400, #65408, #72004, #95327 ),
 .UNSPECIFIED., .F., .F.,
 ( 4, 4 ),
 ( 0.000000000000000000, 9.999999999998897304E-05 ),
 .UNSPECIFIED. ) ;
#63898 = VERTEX_POINT ( 'NONE', #17567 ) ;
#63899 = VECTOR ( 'NONE', #15962, 1000.000000000000000 ) ;
#63900 = EDGE_CURVE ( 'NONE', #36274, #73980, #59014, .T. ) ;
#63901 = CARTESIAN_POINT ( 'NONE',  ( -0.9335293527496063559, -20.33857301660709638, 11.49999999999999645 ) ) ;
#63902 = CARTESIAN_POINT ( 'NONE',  ( -35.62287095715005592, -24.99156045073392463, 7.747789690856161648 ) ) ;
#63903 = DIRECTION ( 'NONE',  ( 0.000000000000000000, 0.000000000000000000, 1.000000000000000000 ) ) ;
#63904 = VERTEX_POINT ( 'NONE', #12808 ) ;
#63905 = LINE ( 'NONE', #70996, #23235 ) ;
#63906 = CARTESIAN_POINT ( 'NONE',  ( 33.63305001869471056, 3.481148584080995700, -11.52139411009015291 ) ) ;
#63907 = CARTESIAN_POINT ( 'NONE',  ( 30.57170936966216601, -5.053692695095620913, 25.34935773471745790 ) ) ;
#63908 = DIRECTION ( 'NONE',  ( -0.000000000000000000, 2.173523156925979552E-06, -0.9999999999976378895 ) ) ;
#63909 = CARTESIAN_POINT ( 'NONE',  ( -86.52287095715004739, -24.34917612407046761, 0.1852690917481102650 ) ) ;
#63910 = EDGE_CURVE ( 'NONE', #68524, #57335, #81023, .T. ) ;
#63911 = LINE ( 'NONE', #41049, #72759 ) ;
#63912 = ORIENTED_EDGE ( 'NONE', *, *, #40256, .T. ) ;
#63913 = DIRECTION ( 'NONE',  ( 0.000000000000000000, -1.000000000000000000, 0.000000000000000000 ) ) ;
#63914 = CARTESIAN_POINT ( 'NONE',  ( 16.23347398924790497, -16.23827457187686463, 11.49999999999999645 ) ) ;
#63915 = CARTESIAN_POINT ( 'NONE',  ( 12.47407908559008760, -19.03963781694049473, 11.49999999999998934 ) ) ;
#63916 = VERTEX_POINT ( 'NONE', #48537 ) ;
#63917 = CARTESIAN_POINT ( 'NONE',  ( -30.47287095715006799, -24.98489225261240065, 7.794711013822600343 ) ) ;
#63918 = LINE ( 'NONE', #72015, #18782 ) ;
#63919 = CARTESIAN_POINT ( 'NONE',  ( -81.52287095715006160, -23.95044443724992789, 10.65354141964649415 ) ) ;
#63920 = CARTESIAN_POINT ( 'NONE',  ( -31.52287095715006160, -29.50250243563736774, 8.947779886222150481 ) ) ;
#63921 = EDGE_CURVE ( 'NONE', #55695, #18015, #51896, .T. ) ;
#63922 = CARTESIAN_POINT ( 'NONE',  ( -69.65142986114982193, -23.48786465467240703, 11.44779295918255002 ) ) ;
#63923 = EDGE_CURVE ( 'NONE', #28525, #73391, #38594, .T. ) ;
#63924 = B_SPLINE_CURVE_WITH_KNOTS ( 'NONE', 3,
 ( #71873, #58150, #65777, #3373, #11461, #42926 ),
 .UNSPECIFIED., .F., .F.,
 ( 4, 2, 4 ),
 ( 1.570755371634494188E-05, 0.001396183895866093174, 0.002776660238015841650 ),
 .UNSPECIFIED. ) ;
#63925 = DIRECTION ( 'NONE',  ( -0.000000000000000000, -1.000000000000000000, -0.000000000000000000 ) ) ;
#63926 = CARTESIAN_POINT ( 'NONE',  ( 32.33217928425143839, -1.682774720514426114, -12.20610769812824437 ) ) ;
#63927 = CARTESIAN_POINT ( 'NONE',  ( -99.14000973721185517, -25.25460558555856494, 5.341016530524719919 ) ) ;
#63928 = EDGE_LOOP ( 'NONE', ( #46083, #61090, #83072, #79411 ) ) ;
#63929 = B_SPLINE_CURVE_WITH_KNOTS ( 'NONE', 3,
 ( #87312, #66011, #87822, #42664 ),
 .UNSPECIFIED., .F., .F.,
 ( 4, 4 ),
 ( 0.000000000000000000, 9.999999999998900014E-05 ),
 .UNSPECIFIED. ) ;
#63930 = CARTESIAN_POINT ( 'NONE',  ( 7.100489274569507181, 19.11111018586187527, 11.49999999999998934 ) ) ;
#63931 = ORIENTED_EDGE ( 'NONE', *, *, #89143, .F. ) ;
#63932 = B_SPLINE_CURVE_WITH_KNOTS ( 'NONE', 3,
 ( #18259, #19740, #50713, #81662 ),
 .UNSPECIFIED., .F., .F.,
 ( 4, 4 ),
 ( 0.000000000000000000, 0.001261718750000001554 ),
 .UNSPECIFIED. ) ;
#63933 = ORIENTED_EDGE ( 'NONE', *, *, #25723, .T. ) ;
#63934 = CARTESIAN_POINT ( 'NONE',  ( 10.47623847176155820, -20.49086732513842080, -1.500000000000002220 ) ) ;
#63936 = EDGE_CURVE ( 'NONE', #27060, #68434, #71867, .T. ) ;
#63935 = DIRECTION ( 'NONE',  ( -3.773278334453079618E-23, 0.9999999999976377785, 2.173523156925979975E-06 ) ) ;
#63937 = ORIENTED_EDGE ( 'NONE', *, *, #5, .F. ) ;
#63938 = CARTESIAN_POINT ( 'NONE',  ( -108.5181428159692558, -23.96169478059714564, 10.65365249895716993 ) ) ;
#63939 = LINE ( 'NONE', #45309, #9283 ) ;
#63940 = EDGE_CURVE ( 'NONE', #10349, #26640, #82271, .T. ) ;
#63941 = EDGE_CURVE ( 'NONE', #27148, #30482, #41133, .T. ) ;
#63942 = CARTESIAN_POINT ( 'NONE',  ( -78.62287095715005592, -24.64965695001468404, 8.947790433994182280 ) ) ;
#63943 = CARTESIAN_POINT ( 'NONE',  ( -53.62368185415960653, -24.66019654487199375, 8.947790411086122830 ) ) ;
#63945 = ORIENTED_EDGE ( 'NONE', *, *, #87373, .F. ) ;
#63944 = CARTESIAN_POINT ( 'NONE',  ( -19.36244235409943926, 8.944087295975924334, 11.49999999999999645 ) ) ;
#63946 = EDGE_LOOP ( 'NONE', ( #16231, #30320, #32833, #33552 ) ) ;
#63947 = CARTESIAN_POINT ( 'NONE',  ( 1.019757120859956512, 22.21710203930399175, 11.49999999999998934 ) ) ;
#63948 = CARTESIAN_POINT ( 'NONE',  ( -17.42616458466809704, -11.11377323884725321, -1.500000000000002220 ) ) ;
#63949 = VECTOR ( 'NONE', #76687, 1000.000000000000227 ) ;
#63950 = VERTEX_POINT ( 'NONE', #2863 ) ;
#63951 = CARTESIAN_POINT ( 'NONE',  ( -6.128026245051341192, -6.376774720514410077, 19.39236848396478763 ) ) ;
#63952 = CARTESIAN_POINT ( 'NONE',  ( -95.58514779555582663, -24.83644354573579349, 8.397322867130096569 ) ) ;
#63953 = ORIENTED_EDGE ( 'NONE', *, *, #55091, .T. ) ;
#63954 = CARTESIAN_POINT ( 'NONE',  ( -127.5895376238167245, -24.64898659630368627, 1.056161002820394046 ) ) ;
#63955 = ORIENTED_EDGE ( 'NONE', *, *, #56483, .F. ) ;
#63956 = CARTESIAN_POINT ( 'NONE',  ( -58.50332490849174150, -24.15620529776628089, 10.23563542870660470 ) ) ;
#63957 = CARTESIAN_POINT ( 'NONE',  ( -70.90965497510502757, -25.15133953616122398, 6.934644986962871904 ) ) ;
#63958 = CARTESIAN_POINT ( 'NONE',  ( -7.158894406585330827, 19.61798520005962487, -1.500000000000002220 ) ) ;
#63959 = CARTESIAN_POINT ( 'NONE',  ( -19.11951126197014261, -10.51958540666066533, 11.49999999999999645 ) ) ;
#63960 = VECTOR ( 'NONE', #73523, 1000.000000000000114 ) ;
#63961 = CARTESIAN_POINT ( 'NONE',  ( -26.80323004365396145, -24.77993723737401766, 7.264871099892241446 ) ) ;
#63962 = CARTESIAN_POINT ( 'NONE',  ( 15.29947330337540556, 3.405372460181236960, -27.16854002387011491 ) ) ;
#63963 = CARTESIAN_POINT ( 'NONE',  ( -15.60622653811170402, 16.18669697583415967, -1.500000000000002220 ) ) ;
#63964 = CARTESIAN_POINT ( 'NONE',  ( -26.12923826827997686, -24.97066931972152304, 5.595194356714370265 ) ) ;
#63965 = CARTESIAN_POINT ( 'NONE',  ( -72.52287095715010423, -23.96177878511308634, 10.65340807706330395 ) ) ;
#63966 = CARTESIAN_POINT ( 'NONE',  ( 3.879810481058463711, -5.876774720514427841, 21.83835767234735670 ) ) ;
#63967 = ORIENTED_EDGE ( 'NONE', *, *, #72697, .T. ) ;
#63968 = VERTEX_POINT ( 'NONE', #41412 ) ;
#63969 = ORIENTED_EDGE ( 'NONE', *, *, #59871, .F. ) ;
#63970 = B_SPLINE_CURVE_WITH_KNOTS ( 'NONE', 3,
 ( #9860, #48436, #71267, #33705 ),
 .UNSPECIFIED., .F., .F.,
 ( 4, 4 ),
 ( 0.000000000000000000, 9.999999999998897304E-05 ),
 .UNSPECIFIED. ) ;
#63971 = CARTESIAN_POINT ( 'NONE',  ( -0.02075734969026145696, 5.866774720514426278, -22.78097719988138081 ) ) ;
#63972 = ORIENTED_EDGE ( 'NONE', *, *, #17995, .T. ) ;
#63973 = CARTESIAN_POINT ( 'NONE',  ( 1.185105815240312888, -21.37944065014308848, -1.500000000000002220 ) ) ;
#63974 = CARTESIAN_POINT ( 'NONE',  ( -15.27869365379592281, -16.34152646814254339, 11.49999999999999645 ) ) ;
#63975 = EDGE_LOOP ( 'NONE', ( #76014, #78636, #63221, #29027 ) ) ;
#63976 = CARTESIAN_POINT ( 'NONE',  ( -82.52287095715006160, -23.47596703998600631, 11.44779298504228571 ) ) ;
#63977 = CARTESIAN_POINT ( 'NONE',  ( 21.04674311342985860, -0.3259866984596996864, 11.49999999999998934 ) ) ;
#63978 = CARTESIAN_POINT ( 'NONE',  ( -30.57662579376099288, -23.78795187145987100, 10.97490056816818971 ) ) ;
#63979 = CARTESIAN_POINT ( 'NONE',  ( -18.69216024341242743, -6.879743215651725308, -1.500000000000002220 ) ) ;
#63980 = CARTESIAN_POINT ( 'NONE',  ( -50.58553729207245908, -24.63419186844610564, 9.035850630976916875 ) ) ;
#63981 = CARTESIAN_POINT ( 'NONE',  ( -80.48373552459977986, -25.30877073647739905, 4.508937044470972211 ) ) ;
#63982 = CARTESIAN_POINT ( 'NONE',  ( 13.62230711432095553, -17.35066874027886286, -1.500000000000002220 ) ) ;
#63983 = ORIENTED_EDGE ( 'NONE', *, *, #25349, .T. ) ;
#63984 = CARTESIAN_POINT ( 'NONE',  ( -65.49890678549689937, -24.40133493613049964, 9.663955038902802386 ) ) ;
#63985 = B_SPLINE_CURVE_WITH_KNOTS ( 'NONE', 3,
 ( #66259, #26169, #79954, #56640, #97183, #65267 ),
 .UNSPECIFIED., .F., .F.,
 ( 4, 2, 4 ),
 ( 6.384118695039489680E-06, 0.001386860460836586732, 0.002767336802978133652 ),
 .UNSPECIFIED. ) ;
#63986 = DIRECTION ( 'NONE',  ( 1.000000000000000000, -0.000000000000000000, 0.000000000000000000 ) ) ;
#63987 = CARTESIAN_POINT ( 'NONE',  ( 20.25184064777635484, 4.944226511633750043, 11.49999999999999645 ) ) ;
#63988 = CARTESIAN_POINT ( 'NONE',  ( 29.65417061107837071, -5.752153662292248448, 28.02209566695815823 ) ) ;
#63989 = FACE_OUTER_BOUND ( 'NONE', #15866, .T. ) ;
#63990 = AXIS2_PLACEMENT_3D ( 'NONE', #53002, #83933, #90546 ) ;
#63991 = CARTESIAN_POINT ( 'NONE',  ( -56.62287095715005592, -23.48783264082478084, -1.443836473390068820 ) ) ;
#63992 = CARTESIAN_POINT ( 'NONE',  ( -20.89022842043660688, 4.291957016416017900, 11.49999999999998934 ) ) ;
#63993 = CARTESIAN_POINT ( 'NONE',  ( -97.62287095715009855, -23.96177878511308634, 10.65340807706329862 ) ) ;
#63994 = CARTESIAN_POINT ( 'NONE',  ( -50.50967068900678925, -25.19546160786025979, 3.296984410641363716 ) ) ;
#63995 = CARTESIAN_POINT ( 'NONE',  ( -71.58953762381673869, -24.65952944569304961, 1.056160979905698571 ) ) ;
#63996 = CARTESIAN_POINT ( 'NONE',  ( -70.65510521343826156, -25.22594453560301631, 6.517383687127669134 ) ) ;
#63997 = CARTESIAN_POINT ( 'NONE',  ( 7.090404290683943067, 21.45231405096426514, -1.500000000000002220 ) ) ;
#63998 = ADVANCED_FACE ( 'NONE', ( #26181 ), #33795, .F. ) ;
#63999 = DIRECTION ( 'NONE',  ( 1.000000000000000000, 3.773278334444167608E-23, 8.201307833595939069E-29 ) ) ;
#64000 = EDGE_LOOP ( 'NONE', ( #58347, #2325, #76104, #22936, #35536, #21836, #65598, #39335, #28447, #13807, #8908, #85019, #16386, #35672, #9236, #53057, #308, #86271, #24555, #77732 ) ) ;
#64001 = CARTESIAN_POINT ( 'NONE',  ( -51.51942953060336805, -25.27075631336522221, 6.048200114948329542 ) ) ;
#64002 = CARTESIAN_POINT ( 'NONE',  ( -31.55268919091492563, -23.96169478059712432, 10.65365249895719124 ) ) ;
#64003 = CARTESIAN_POINT ( 'NONE',  ( 5.252985061998082017, 18.97096265210048571, 11.49999999999999645 ) ) ;
#64004 = DIRECTION ( 'NONE',  ( 1.000000000000000000, 3.773278334444167608E-23, 8.201307833595939069E-29 ) ) ;
#64005 = DIRECTION ( 'NONE',  ( -1.000000000000000000, -0.000000000000000000, 0.000000000000000000 ) ) ;
#64006 = EDGE_LOOP ( 'NONE', ( #93088, #12885 ) ) ;
#64007 = CARTESIAN_POINT ( 'NONE',  ( -99.62961886916561127, -24.15543982623907837, -0.2315651400026449425 ) ) ;
#64008 = CARTESIAN_POINT ( 'NONE',  ( -55.62287095715002749, -24.14321612903111358, -0.2833117244521575206 ) ) ;
#64010 = EDGE_CURVE ( 'NONE', #17025, #75293, #59654, .T. ) ;
#64009 = CARTESIAN_POINT ( 'NONE',  ( -124.6246528789468755, -24.15620529776629510, 10.23563542870659404 ) ) ;
#64011 = B_SPLINE_CURVE_WITH_KNOTS ( 'NONE', 3,
 ( #40803, #88988, #96102, #95095, #3265, #11852, #87480, #65175 ),
 .UNSPECIFIED., .F., .F.,
 ( 4, 2, 2, 4 ),
 ( 0.0001293435094372204610, 0.002876179024813956854, 0.004249596782502322069, 0.005623014540190688151 ),
 .UNSPECIFIED. ) ;
#64012 = EDGE_CURVE ( 'NONE', #59693, #82244, #6203, .T. ) ;
#64013 = DIRECTION ( 'NONE',  ( -1.000000000000000000, -0.000000000000000000, 0.000000000000000000 ) ) ;
#64014 = LINE ( 'NONE', #93035, #18790 ) ;
#64015 = EDGE_CURVE ( 'NONE', #95575, #5456, #45983, .T. ) ;
#64016 = CARTESIAN_POINT ( 'NONE',  ( -19.06493894060550787, -22.58126814178390518, 11.44779298504228038 ) ) ;
#64017 = CARTESIAN_POINT ( 'NONE',  ( 18.87426695099163254, 5.791883100666666451, -1.500000000000002220 ) ) ;
#64018 = ORIENTED_EDGE ( 'NONE', *, *, #89778, .F. ) ;
#64019 = EDGE_CURVE ( 'NONE', #77908, #90963, #76205, .T. ) ;
#64020 = CARTESIAN_POINT ( 'NONE',  ( -9.806399893892750796, 17.69452640759178408, 11.49999999999999645 ) ) ;
#64021 = CARTESIAN_POINT ( 'NONE',  ( 5.671814302646631667, -5.876774720514418959, 20.58085404595000512 ) ) ;
#64022 = VECTOR ( 'NONE', #75222, 1000.000000000000000 ) ;
#64023 = VERTEX_POINT ( 'NONE', #62001 ) ;
#64024 = CARTESIAN_POINT ( 'NONE',  ( -52.55620429048339304, -24.65952944569303895, 1.056160979905694575 ) ) ;
#64025 = DIRECTION ( 'NONE',  ( -0.000000000000000000, -1.000000000000000000, -0.000000000000000000 ) ) ;
#64026 = CARTESIAN_POINT ( 'NONE',  ( -100.3784397666924804, -25.03145178421234007, 7.561117244693161155 ) ) ;
#64027 = CARTESIAN_POINT ( 'NONE',  ( -82.62287095715004170, -24.50216790748204332, 0.6166512839542541702 ) ) ;
#64028 = FACE_OUTER_BOUND ( 'NONE', #29827, .T. ) ;
#64029 = DIRECTION ( 'NONE',  ( 0.000000000000000000, -1.000000000000000000, 0.000000000000000000 ) ) ;
#64030 = CARTESIAN_POINT ( 'NONE',  ( -3.121018476474317183, -19.76494895549465980, -1.500000000000002220 ) ) ;
#64031 = EDGE_CURVE ( 'NONE', #39944, #5284, #7139, .T. ) ;
#64032 = AXIS2_PLACEMENT_3D ( 'NONE', #57334, #56831, #18246 ) ;
#64033 = CARTESIAN_POINT ( 'NONE',  ( -58.62287095715005592, -24.50216790748098461, 0.6166512839513552668 ) ) ;
#64034 = CARTESIAN_POINT ( 'NONE',  ( -116.6285126153758682, -23.73791477778912551, 11.05961554403170055 ) ) ;
#64035 = VERTEX_POINT ( 'NONE', #96 ) ;
#64036 = EDGE_CURVE ( 'NONE', #36448, #40304, #94306, .T. ) ;
#64037 = CARTESIAN_POINT ( 'NONE',  ( -79.50498077729714907, -24.35071581493543036, 9.817618358456028815 ) ) ;
#64038 = CARTESIAN_POINT ( 'NONE',  ( -35.47955930521835910, -24.63355581998385091, 0.9682620441944008727 ) ) ;
#64039 = CARTESIAN_POINT ( 'NONE',  ( -83.52287095715006160, -24.64898659630367916, 1.056161002820826145 ) ) ;
#64040 = DIRECTION ( 'NONE',  ( 3.773278334444167608E-23, -1.000000000000000000, 0.000000000000000000 ) ) ;
#64041 = CARTESIAN_POINT ( 'NONE',  ( -73.49934423242160619, -24.51314013834315375, 0.6176544820404108460 ) ) ;
#64042 = EDGE_CURVE ( 'NONE', #43797, #69058, #74265, .T. ) ;
#64043 = CARTESIAN_POINT ( 'NONE',  ( -20.77875734969026311, -6.143225279485574397, 27.31649921512899937 ) ) ;
#64044 = CARTESIAN_POINT ( 'NONE',  ( -84.52287095715006160, -24.64898659630528854, 1.056161002820826145 ) ) ;
#64045 = VERTEX_POINT ( 'NONE', #22410 ) ;
#64046 = CARTESIAN_POINT ( 'NONE',  ( 11.02309159617336221, -17.05227643984133934, 11.49999999999998934 ) ) ;
#64047 = B_SPLINE_CURVE_WITH_KNOTS ( 'NONE', 3,
 ( #46365, #40259, #46871, #79307, #39246, #70704 ),
 .UNSPECIFIED., .F., .F.,
 ( 4, 2, 4 ),
 ( 0.000000000000000000, 0.001380764517853250335, 0.002761529035706500670 ),
 .UNSPECIFIED. ) ;
#64048 = DIRECTION ( 'NONE',  ( 0.000000000000000000, -0.9999999999976377785, -2.173523156925978705E-06 ) ) ;
#64049 = FACE_OUTER_BOUND ( 'NONE', #44991, .T. ) ;
#64050 = CARTESIAN_POINT ( 'NONE',  ( -59.51515945767989280, -23.73791477778911840, 11.05961554403171299 ) ) ;
#64052 = EDGE_LOOP ( 'NONE', ( #77176, #29410, #28582, #80298 ) ) ;
#64051 = EDGE_CURVE ( 'NONE', #5942, #19180, #52389, .T. ) ;
#64053 = DIRECTION ( 'NONE',  ( -3.773278334453079618E-23, 0.9999999999976377785, 2.173523156925979975E-06 ) ) ;
#64054 = CARTESIAN_POINT ( 'NONE',  ( -3.482456173223098528, 20.84670800329844198, 11.49999999999999645 ) ) ;
#64055 = CIRCLE ( 'NONE', #96409, 28.96799999999999642 ) ;
#64056 = CARTESIAN_POINT ( 'NONE',  ( 14.67205787815721862, 16.58792043909384262, 11.49999999999998934 ) ) ;
#64057 = EDGE_CURVE ( 'NONE', #27910, #64814, #89459, .T. ) ;
#64058 = CARTESIAN_POINT ( 'NONE',  ( -20.17529555308526668, -4.016306826964139098, -1.500000000000002220 ) ) ;
#64059 = EDGE_LOOP ( 'NONE', ( #29799, #59681, #54593, #9008 ) ) ;
#64060 = CARTESIAN_POINT ( 'NONE',  ( -88.52287095715006160, -29.50250243563736774, 8.947779886222139822 ) ) ;
#64061 = ORIENTED_EDGE ( 'NONE', *, *, #82964, .T. ) ;
#64062 = CARTESIAN_POINT ( 'NONE',  ( -54.62799017530142009, -24.51314013834315020, 0.6176544820404069602 ) ) ;
#64063 = LINE ( 'NONE', #94975, #8049 ) ;
#64064 = VERTEX_POINT ( 'NONE', #99039 ) ;
#64065 = VERTEX_POINT ( 'NONE', #29536 ) ;
#64066 = ORIENTED_EDGE ( 'NONE', *, *, #75635, .T. ) ;
#64067 = CARTESIAN_POINT ( 'NONE',  ( -100.5228709571500900, -23.84047902841603417, -0.8780736468305739839 ) ) ;
#64068 = CARTESIAN_POINT ( 'NONE',  ( 7.139069293134643779, -6.376774720514422512, 20.58118917620081945 ) ) ;
#64069 = CARTESIAN_POINT ( 'NONE',  ( 5.326923076923078426, -6.376774720514420736, 20.76772836538461320 ) ) ;
#64070 = CARTESIAN_POINT ( 'NONE',  ( -1.843323519027639357, -20.62917239659568835, -1.500000000000002220 ) ) ;
#64071 = CARTESIAN_POINT ( 'NONE',  ( 19.51036611237648088, 9.378288983258578071, 11.49999999999999645 ) ) ;
#64072 = ORIENTED_EDGE ( 'NONE', *, *, #81154, .T. ) ;
#64073 = LINE ( 'NONE', #63567, #98509 ) ;
#64074 = CARTESIAN_POINT ( 'NONE',  ( -111.7766968413051671, -25.28171427076103583, 4.234743059359621142 ) ) ;
#64075 = CARTESIAN_POINT ( 'NONE',  ( 22.22467975111640470, 2.813832150844377100, -1.500000000000002220 ) ) ;
#64076 = CARTESIAN_POINT ( 'NONE',  ( -79.42863770186421846, -25.27874940277076732, 6.408999251374608797 ) ) ;
#64077 = DIRECTION ( 'NONE',  ( -0.9496245541219264785, -0.000000000000000000, -0.3133898629642195011 ) ) ;
#64078 = ORIENTED_EDGE ( 'NONE', *, *, #66061, .T. ) ;
#64079 = DIRECTION ( 'NONE',  ( -1.000000000000000000, 0.000000000000000000, 0.000000000000000000 ) ) ;
#64080 = CARTESIAN_POINT ( 'NONE',  ( -83.62287095715005592, -24.64898659630528854, 1.056161002820826145 ) ) ;
#64081 = ORIENTED_EDGE ( 'NONE', *, *, #4372, .T. ) ;
#64082 = ORIENTED_EDGE ( 'NONE', *, *, #88205, .T. ) ;
#64083 = VECTOR ( 'NONE', #8106, 1000.000000000000000 ) ;
#64084 = CARTESIAN_POINT ( 'NONE',  ( -45.52287095715006160, -23.47596703998600631, 11.44779298504229104 ) ) ;
#64085 = ORIENTED_EDGE ( 'NONE', *, *, #71779, .F. ) ;
#64086 = DIRECTION ( 'NONE',  ( 0.000000000000000000, 2.173523156925980399E-06, -0.9999999999976378895 ) ) ;
#64087 = CARTESIAN_POINT ( 'NONE',  ( 19.37530031839547107, -8.734557088507903799, -1.500000000000002220 ) ) ;
#64088 = EDGE_LOOP ( 'NONE', ( #1581, #94517, #4411, #49568 ) ) ;
#64089 = DIRECTION ( 'NONE',  ( 0.000000000000000000, -2.173523156925980399E-06, 0.9999999999976378895 ) ) ;
#64090 = CARTESIAN_POINT ( 'NONE',  ( -17.41291239988371231, 13.16847401419012975, 11.49999999999998934 ) ) ;
#64091 = CARTESIAN_POINT ( 'NONE',  ( -52.64485392522220053, -23.96169478059712787, 10.65365249895718591 ) ) ;
#64092 = DIRECTION ( 'NONE',  ( 0.000000000000000000, 2.173523156925980399E-06, -0.9999999999976378895 ) ) ;
#64093 = CARTESIAN_POINT ( 'NONE',  ( -116.6228709571500985, -23.73907113216991860, -1.053371485793224371 ) ) ;
#64094 = CARTESIAN_POINT ( 'NONE',  ( 13.92123049006271707, -16.85212209846622855, -1.500000000000002220 ) ) ;
#64095 = CARTESIAN_POINT ( 'NONE',  ( -30.57287095715006942, -24.05021112939445871, -0.4555005541943638048 ) ) ;
#64096 = ORIENTED_EDGE ( 'NONE', *, *, #6213, .F. ) ;
#64097 = LINE ( 'NONE', #73192, #2 ) ;
#64098 = CARTESIAN_POINT ( 'NONE',  ( -85.58560456462899424, -24.73531770709095312, 8.716586749053508498 ) ) ;
#64099 = ORIENTED_EDGE ( 'NONE', *, *, #89394, .F. ) ;
#64100 = AXIS2_PLACEMENT_3D ( 'NONE', #67821, #28744, #22597 ) ;
#64101 = VECTOR ( 'NONE', #69267, 1000.000000000000114 ) ;
#64102 = ORIENTED_EDGE ( 'NONE', *, *, #94165, .T. ) ;
#64103 = VERTEX_POINT ( 'NONE', #99534 ) ;
#64104 = DIRECTION ( 'NONE',  ( -0.000000000000000000, -1.000000000000000000, -0.000000000000000000 ) ) ;
#64105 = CARTESIAN_POINT ( 'NONE',  ( -82.52213984707648819, -23.48783264082478439, -1.443836473390069486 ) ) ;
#64106 = CARTESIAN_POINT ( 'NONE',  ( 15.87343765641381665, 14.11872912734625274, -1.500000000000002220 ) ) ;
#64107 = LINE ( 'NONE', #41248, #10971 ) ;
#64108 = DIRECTION ( 'NONE',  ( 0.000000000000000000, 2.173523156925980399E-06, -0.9999999999976378895 ) ) ;
#64109 = CARTESIAN_POINT ( 'NONE',  ( 14.76093561896378148, -3.316774720514426456, -26.55548769130088971 ) ) ;
#64110 = CARTESIAN_POINT ( 'NONE',  ( -48.58953762381672448, -23.47596703998600276, 11.44779298504227505 ) ) ;
#64111 = CARTESIAN_POINT ( 'NONE',  ( 8.513215801882951794, -17.43586836189350819, -1.500000000000002220 ) ) ;
#64112 = CARTESIAN_POINT ( 'NONE',  ( -45.53132931798297989, -24.73486907724918282, 1.287355809206962576 ) ) ;
#64113 = VERTEX_POINT ( 'NONE', #14803 ) ;
#64114 = ADVANCED_FACE ( 'NONE', ( #21911 ), #69614, .T. ) ;
#64115 = CARTESIAN_POINT ( 'NONE',  ( 0.2958748881272694198, 19.47992435465491212, 11.49999999999999645 ) ) ;
#64116 = CARTESIAN_POINT ( 'NONE',  ( -5.514838905578028694, -5.876774720514408301, 19.81240905262003338 ) ) ;
#64117 = ADVANCED_FACE ( 'NONE', ( #22900 ), #6701, .F. ) ;
#64118 = B_SPLINE_CURVE_WITH_KNOTS ( 'NONE', 3,
 ( #86765, #79150, #17253, #78632 ),
 .UNSPECIFIED., .F., .F.,
 ( 4, 4 ),
 ( 0.2889692275360895013, 0.2899699745768550274 ),
 .UNSPECIFIED. ) ;
#64119 = DIRECTION ( 'NONE',  ( -2.464095846557964090E-17, -1.000000000000000000, 0.000000000000000000 ) ) ;
#64120 = ORIENTED_EDGE ( 'NONE', *, *, #30425, .T. ) ;
#64121 = EDGE_CURVE ( 'NONE', #86101, #55690, #27273, .T. ) ;
#64122 = CARTESIAN_POINT ( 'NONE',  ( 4.819673832743241348, -5.876774720514421624, 21.07066438048017076 ) ) ;
#64123 = CYLINDRICAL_SURFACE ( 'NONE', #18818, 0.8160000000000007248 ) ;
#64124 = ADVANCED_FACE ( 'NONE', ( #54391 ), #50663, .T. ) ;
#64125 = CARTESIAN_POINT ( 'NONE',  ( -111.5228709571500616, -24.64965694238407323, 8.947790433994192938 ) ) ;
#64126 = CARTESIAN_POINT ( 'NONE',  ( -81.87824661256287584, -25.03155794964914094, 6.339755953538114497 ) ) ;
#64127 = CARTESIAN_POINT ( 'NONE',  ( 13.10555085358618221, -14.64361678476065087, -1.500000000000002220 ) ) ;
#64128 = ORIENTED_EDGE ( 'NONE', *, *, #78076, .T. ) ;
#64129 = VECTOR ( 'NONE', #14816, 1000.000000000000114 ) ;
#64130 = FACE_OUTER_BOUND ( 'NONE', #75601, .T. ) ;
#64131 = CARTESIAN_POINT ( 'NONE',  ( -46.58953762381672448, -23.47593901973091235, -1.443836447539009749 ) ) ;
#64133 = EDGE_CURVE ( 'NONE', #71901, #70309, #90714, .T. ) ;
#64132 = DATE_AND_TIME ( #33148, #58686 ) ;
#64134 = CARTESIAN_POINT ( 'NONE',  ( 3.671066620544169101, -5.876774720514423400, 21.47597918715562670 ) ) ;
#64135 = CARTESIAN_POINT ( 'NONE',  ( 30.93860345374796594, 6.376774720514426953, 28.83647319851474933 ) ) ;
#64136 = DIRECTION ( 'NONE',  ( 0.000000000000000000, -1.000000000000000000, 0.000000000000000000 ) ) ;
#64137 = DIRECTION ( 'NONE',  ( 1.000000000000000000, 0.000000000000000000, 0.000000000000000000 ) ) ;
#64138 = CARTESIAN_POINT ( 'NONE',  ( -81.90174979306682701, -25.31249729222309597, 5.276660411446114196 ) ) ;
#64140 = B_SPLINE_CURVE_WITH_KNOTS ( 'NONE', 3,
 ( #37632, #22882, #99514, #91914, #74, #22389, #53373, #14785, #84298, #7684, #45750, #76671, #7177, #100006, #38126, #39131, #53870, #84802 ),
 .UNSPECIFIED., .F., .F.,
 ( 4, 2, 2, 2, 2, 2, 2, 2, 4 ),
 ( 0.004711262329854449225, 0.005300180574508829220, 0.005889098819163209216, 0.006478017063817618701, 0.007066935308472027319, 0.007655853553126437672, 0.008244771797780846290, 0.008833690042435254908, 0.009422608287089665260 ),
 .UNSPECIFIED. ) ;
#64139 = CARTESIAN_POINT ( 'NONE',  ( -43.62287095715007013, -24.35013146730203459, 9.818937971375111928 ) ) ;
#64141 = CARTESIAN_POINT ( 'NONE',  ( -76.52287095715007581, -23.47596703998600631, 11.44779298504228571 ) ) ;
#64142 = LINE ( 'NONE', #25550, #12159 ) ;
#64143 = CARTESIAN_POINT ( 'NONE',  ( -13.68957358570155769, -14.46295258127404892, -1.500000000000002220 ) ) ;
#64144 = CARTESIAN_POINT ( 'NONE',  ( -75.58253123086370806, -24.83644354573578994, 8.397322867130100121 ) ) ;
#64145 = CARTESIAN_POINT ( 'NONE',  ( -1.214729172165279092, -19.82145330704504360, -1.500000000000002220 ) ) ;
#64146 = ORIENTED_EDGE ( 'NONE', *, *, #90211, .F. ) ;
#64147 = DIRECTION ( 'NONE',  ( -0.7512896232465786639, -0.000000000000000000, -0.6599726524652470561 ) ) ;
#64148 = CARTESIAN_POINT ( 'NONE',  ( -125.5228709571500900, -24.91544648472620693, 1.928969306349231028 ) ) ;
#64149 = DIRECTION ( 'NONE',  ( -3.773278334453079618E-23, 0.9999999999976377785, 2.173523156925979975E-06 ) ) ;
#64150 = CARTESIAN_POINT ( 'NONE',  ( 9.628234360240019996, 18.42577530400075858, 11.49999999999999645 ) ) ;
#64151 = CARTESIAN_POINT ( 'NONE',  ( -81.60465383657505356, -23.48783264082478084, -1.443836473390067043 ) ) ;
#64152 = CARTESIAN_POINT ( 'NONE',  ( -106.5198659666137644, -23.73766607897671221, -1.055555164236449572 ) ) ;
#64153 = CARTESIAN_POINT ( 'NONE',  ( -12.29745307268338195, -19.16510367807413218, 11.49999999999999645 ) ) ;
#64154 = VECTOR ( 'NONE', #82622, 1000.000000000000114 ) ;
#64155 = ORIENTED_EDGE ( 'NONE', *, *, #51906, .F. ) ;
#64156 = CARTESIAN_POINT ( 'NONE',  ( -91.62287095715004170, -24.33832256527047733, 0.1851278514138617048 ) ) ;
#64158 = AXIS2_PLACEMENT_3D ( 'NONE', #83901, #21486, #67204 ) ;
#64157 = CARTESIAN_POINT ( 'NONE',  ( -10.79305683637731406, 5.965225279485594001, -27.49869550653260930 ) ) ;
#64159 = ORIENTED_EDGE ( 'NONE', *, *, #27772, .F. ) ;
#64160 = VECTOR ( 'NONE', #43886, 1000.000000000000114 ) ;
#64161 = CARTESIAN_POINT ( 'NONE',  ( -20.01257119864951051, 2.908879540851186274, 11.49999999999998934 ) ) ;
#64162 = CARTESIAN_POINT ( 'NONE',  ( -55.62287095715004881, -25.00158670708909625, 2.256160236439165967 ) ) ;
#64163 = AXIS2_PLACEMENT_3D ( 'NONE', #13031, #36381, #44501 ) ;
#64164 = CARTESIAN_POINT ( 'NONE',  ( -49.55620429048340014, -24.65952944569304606, 1.056160979905693909 ) ) ;
#64165 = AXIS2_PLACEMENT_3D ( 'NONE', #99433, #76589, #45663 ) ;
#64166 = DIRECTION ( 'NONE',  ( -0.000000000000000000, 1.000000000000000000, -0.000000000000000000 ) ) ;
#64167 = VERTEX_POINT ( 'NONE', #56909 ) ;
#64168 = CARTESIAN_POINT ( 'NONE',  ( 29.80070917940689412, 5.965225279485572685, 27.39560796525321607 ) ) ;
#64169 = CARTESIAN_POINT ( 'NONE',  ( -84.52287095715004739, -24.50321055353805377, 9.387540953477524042 ) ) ;
#64170 = CARTESIAN_POINT ( 'NONE',  ( -15.86121933104946535, 12.22609501325904624, -1.500000000000002220 ) ) ;
#64171 = PLANE ( 'NONE',  #75556 ) ;
#64172 = CARTESIAN_POINT ( 'NONE',  ( -8.441512789788195192, 19.21024974253229800, 11.49999999999999645 ) ) ;
#64173 = CARTESIAN_POINT ( 'NONE',  ( -29.58433278696464797, -25.11104544706328667, 6.768552479589499349 ) ) ;
#64174 = CARTESIAN_POINT ( 'NONE',  ( -6.660000000000001030, -10.15233964170348457, 0.003711184059992174607 ) ) ;
#64175 = CARTESIAN_POINT ( 'NONE',  ( -8.753671783739276790, -20.25744411100385634, 11.49999999999998934 ) ) ;
#64176 = ADVANCED_FACE ( 'NONE', ( #78203 ), #85832, .F. ) ;
#64177 = CARTESIAN_POINT ( 'NONE',  ( 14.76093561896379214, -6.475225279485574248, -26.55548769130089681 ) ) ;
#64178 = VERTEX_POINT ( 'NONE', #9713 ) ;
#64179 = CARTESIAN_POINT ( 'NONE',  ( -86.52287095715006160, -23.47593901973090169, -1.443836447538996648 ) ) ;
#64180 = CARTESIAN_POINT ( 'NONE',  ( 16.00000000000000000, 0.000000000000000000, 24.00000000000000000 ) ) ;
#64181 = CARTESIAN_POINT ( 'NONE',  ( -72.53830702939148978, -24.65952944569304250, 1.056160979905695463 ) ) ;
#64182 = EDGE_LOOP ( 'NONE', ( #49284, #54114, #80915, #66323 ) ) ;
#64183 = CARTESIAN_POINT ( 'NONE',  ( 2.747717285871495108, -6.376774720514404748, 18.94713297040818034 ) ) ;
#64184 = EDGE_LOOP ( 'NONE', ( #36251, #46101, #253, #34237 ) ) ;
#64185 = ORIENTED_EDGE ( 'NONE', *, *, #45604, .T. ) ;
#64186 = LINE ( 'NONE', #17984, #82566 ) ;
#64187 = CARTESIAN_POINT ( 'NONE',  ( -101.1996739087839075, -25.27404679889542294, 3.060140427661463214 ) ) ;
#64188 = DIRECTION ( 'NONE',  ( 0.000000000000000000, 0.9999999999976377785, 2.173523156925979975E-06 ) ) ;
#64189 = CARTESIAN_POINT ( 'NONE',  ( 8.954683214801249846, 18.48387022957959047, -1.500000000000002220 ) ) ;
#64190 = ORIENTED_EDGE ( 'NONE', *, *, #99360, .F. ) ;
#64191 = LINE ( 'NONE', #65195, #83404 ) ;
#64192 = CYLINDRICAL_SURFACE ( 'NONE', #46676, 1.150000000000003464 ) ;
#64193 = LINE ( 'NONE', #57572, #73992 ) ;
#64194 = CARTESIAN_POINT ( 'NONE',  ( 3.885606641962014329, -21.97303888676646721, -1.500000000000002220 ) ) ;
#64195 = CARTESIAN_POINT ( 'NONE',  ( -81.62287095715008434, -23.72747288104441665, -1.053458166803661555 ) ) ;
#64196 = CARTESIAN_POINT ( 'NONE',  ( -26.35650876483003557, -24.67614927925039936, 7.701557122907957798 ) ) ;
#64197 = ORIENTED_EDGE ( 'NONE', *, *, #37967, .F. ) ;
#64198 = CARTESIAN_POINT ( 'NONE',  ( -50.52287095715007581, -25.00182538069144655, 7.747789668545104647 ) ) ;
#64199 = FACE_OUTER_BOUND ( 'NONE', #47431, .T. ) ;
#64200 = B_SPLINE_CURVE_WITH_KNOTS ( 'NONE', 3,
 ( #26924, #65514, #43158, #97430, #89816, #36521, #52260, #35042, #50267, #81208, #51261, #5075, #73107, #82200, #66013, #3596 ),
 .UNSPECIFIED., .F., .F.,
 ( 4, 2, 2, 2, 2, 2, 2, 4 ),
 ( -2.132270449955935040E-05, 0.0007770955584725032679, 0.001176304689958539498, 0.001575513821444575729, 0.001974722952930611959, 0.002373932084416648623, 0.002773141215902684420, 0.003172350347388721084 ),
 .UNSPECIFIED. ) ;
#64201 = CARTESIAN_POINT ( 'NONE',  ( -14.93763623016880082, -14.57113377498261997, -1.500000000000002220 ) ) ;
#64202 = ORIENTED_EDGE ( 'NONE', *, *, #36699, .F. ) ;
#64204 = VERTEX_POINT ( 'NONE', #2615 ) ;
#64203 = CARTESIAN_POINT ( 'NONE',  ( -52.52287095715007581, -23.96127896942151025, -0.6493128930935695431 ) ) ;
#64205 = VERTEX_POINT ( 'NONE', #48795 ) ;
#64206 = CARTESIAN_POINT ( 'NONE',  ( -70.34543693012690824, -25.03149372849369669, 7.563174219444441349 ) ) ;
#64207 = CARTESIAN_POINT ( 'NONE',  ( -1.165634184549018126, -21.02984315360824752, -1.500000000000002220 ) ) ;
#64208 = VERTEX_POINT ( 'NONE', #33055 ) ;
#64209 = CARTESIAN_POINT ( 'NONE',  ( -93.62287095715009855, -23.73934037231757799, 11.05740245334328975 ) ) ;
#64210 = PLANE ( 'NONE',  #61218 ) ;
#64211 = CARTESIAN_POINT ( 'NONE',  ( -105.6228709571500417, -29.50248789122583659, 2.256150453626215580 ) ) ;
#64212 = CARTESIAN_POINT ( 'NONE',  ( -86.60313800047151744, -23.48786465467240703, 11.44779295918254647 ) ) ;
#64213 = CARTESIAN_POINT ( 'NONE',  ( -59.64292777622080877, -23.96119346886879597, -0.6495511937832131322 ) ) ;
#64214 = CARTESIAN_POINT ( 'NONE',  ( -14.64807036877012258, -15.96857234361563904, -1.500000000000002220 ) ) ;
#64215 = DIRECTION ( 'NONE',  ( 0.000000000000000000, 0.000000000000000000, -1.000000000000000000 ) ) ;
#64217 = ORIENTED_EDGE ( 'NONE', *, *, #35751, .F. ) ;
#64216 = CARTESIAN_POINT ( 'NONE',  ( -14.60993195340527251, 16.82711592829100411, 11.49999999999999645 ) ) ;
#64218 = CARTESIAN_POINT ( 'NONE',  ( -51.48368152949297638, -25.31441875625928972, 5.903371675124650331 ) ) ;
#64219 = CARTESIAN_POINT ( 'NONE',  ( -70.59960031398057367, -25.30103364020432011, 5.335303155633611460 ) ) ;
#64220 = ORIENTED_EDGE ( 'NONE', *, *, #22599, .F. ) ;
#64221 = AXIS2_PLACEMENT_3D ( 'NONE', #10955, #95690, #88584 ) ;
#64222 = EDGE_CURVE ( 'NONE', #28254, #35481, #87329, .T. ) ;
#64224 = ORIENTED_EDGE ( 'NONE', *, *, #97108, .F. ) ;
#64223 = DIRECTION ( 'NONE',  ( -0.000000000000000000, 1.000000000000000000, -0.000000000000000000 ) ) ;
#64225 = ORIENTED_EDGE ( 'NONE', *, *, #53937, .T. ) ;
#64226 = CARTESIAN_POINT ( 'NONE',  ( 31.62034159138967837, -4.397688677367943555, -2.670054032269225885 ) ) ;
#64227 = AXIS2_PLACEMENT_3D ( 'NONE', #77844, #16452, #70757 ) ;
#64228 = CARTESIAN_POINT ( 'NONE',  ( 19.96388892861992659, -2.714421270036905032, -1.500000000000002220 ) ) ;
#64229 = CARTESIAN_POINT ( 'NONE',  ( -126.5228709571500616, -23.72773821059536914, 11.05748984161097326 ) ) ;
#64230 = VERTEX_POINT ( 'NONE', #591 ) ;
#64231 = VECTOR ( 'NONE', #89248, 1000.000000000000000 ) ;
#64232 = EDGE_CURVE ( 'NONE', #3436, #25180, #48305, .T. ) ;
#64233 = CARTESIAN_POINT ( 'NONE',  ( -130.5728709571500588, -24.61658504062384978, 9.350733115928049344 ) ) ;
#64234 = CARTESIAN_POINT ( 'NONE',  ( -21.67104271438225638, 5.786422744429515319, -1.500000000000002220 ) ) ;
#64235 = VECTOR ( 'NONE', #11257, 1000.000000000000227 ) ;
#64236 = EDGE_LOOP ( 'NONE', ( #17391, #93559, #58062, #88382 ) ) ;
#64237 = VERTEX_POINT ( 'NONE', #15811 ) ;
#64238 = CARTESIAN_POINT ( 'NONE',  ( -112.5139873076401074, -24.66019654487200086, 8.947790411086112172 ) ) ;
#64239 = CARTESIAN_POINT ( 'NONE',  ( -101.5528284347318930, -24.15620529776628800, 10.23563542870660292 ) ) ;
#64240 = EDGE_CURVE ( 'NONE', #86154, #74525, #32546, .T. ) ;
#64241 = CARTESIAN_POINT ( 'NONE',  ( -40.41683116089613748, -25.31532428806244539, 5.082404371757057504 ) ) ;
#64242 = CARTESIAN_POINT ( 'NONE',  ( -53.01255352321339842, 5.356774720514425603, 35.59556822165056644 ) ) ;
#64243 = AXIS2_PLACEMENT_3D ( 'NONE', #67269, #98188, #59657 ) ;
#64244 = EDGE_CURVE ( 'NONE', #60701, #53473, #3571, .T. ) ;
#64245 = CARTESIAN_POINT ( 'NONE',  ( -130.5728709571501440, -25.14064729901805961, 2.712351064733618422 ) ) ;
#64246 = CARTESIAN_POINT ( 'NONE',  ( -18.05301863641116000, -7.546005365994440162, 11.49999999999998934 ) ) ;
#64247 = EDGE_CURVE ( 'NONE', #76987, #4757, #55397, .T. ) ;
#64248 = CARTESIAN_POINT ( 'NONE',  ( -46.64014652896692326, -24.15543982623906416, -0.2315651400026683127 ) ) ;
#64249 = VERTEX_POINT ( 'NONE', #16818 ) ;
#64250 = CARTESIAN_POINT ( 'NONE',  ( -17.63906703526961550, 12.34593017946836291, 11.49999999999998934 ) ) ;
#64251 = DIRECTION ( 'NONE',  ( -3.773278334453079618E-23, 0.9999999999976377785, 2.173523156925979975E-06 ) ) ;
#64252 = EDGE_CURVE ( 'NONE', #62581, #31857, #56410, .T. ) ;
#64253 = DIRECTION ( 'NONE',  ( -0.9952638024365005887, -0.000000000000000000, -0.09721092304694052555 ) ) ;
#64254 = CARTESIAN_POINT ( 'NONE',  ( -53.62287095715005592, -23.47596703998600276, 11.44779298504227683 ) ) ;
#64255 = DIRECTION ( 'NONE',  ( -0.000000000000000000, -0.000000000000000000, -1.000000000000000000 ) ) ;
#64256 = CARTESIAN_POINT ( 'NONE',  ( -20.69623851537618364, -9.862649113751288610, -1.500000000000002220 ) ) ;
#64257 = DATE_AND_TIME ( #64765, #26238 ) ;
#64258 = DIRECTION ( 'NONE',  ( 1.000000000000000000, 0.000000000000000000, 0.000000000000000000 ) ) ;
#64259 = CARTESIAN_POINT ( 'NONE',  ( -71.30457154551150722, -25.25559839591754496, 6.209207386190694677 ) ) ;
#64260 = CARTESIAN_POINT ( 'NONE',  ( -19.81368827760683260, -3.497637702615509880, 11.49999999999999645 ) ) ;
#64261 = CARTESIAN_POINT ( 'NONE',  ( -110.1676456071266870, -25.28814069637450146, 2.835829433892736340 ) ) ;
#64262 = PLANE ( 'NONE',  #53288 ) ;
#64263 = FACE_OUTER_BOUND ( 'NONE', #45720, .T. ) ;
#64264 = CARTESIAN_POINT ( 'NONE',  ( 24.50000000000000000, -0.9000000000000000222, -2.000000000000000000 ) ) ;
#64265 = EDGE_CURVE ( 'NONE', #2529, #55213, #74889, .T. ) ;
#64266 = CARTESIAN_POINT ( 'NONE',  ( -53.52287095715008292, -23.47593901973090169, -1.443836447538997092 ) ) ;
#64267 = CARTESIAN_POINT ( 'NONE',  ( 12.34629653512297409, 15.52844579862587437, -1.500000000000002220 ) ) ;
#64268 = CARTESIAN_POINT ( 'NONE',  ( -65.05438548721848235, 3.316774720514426456, 27.45402280011862572 ) ) ;
#64269 = CARTESIAN_POINT ( 'NONE',  ( 0.7808950796103379943, -19.64173473864696717, -1.500000000000002220 ) ) ;
#64270 = AXIS2_PLACEMENT_3D ( 'NONE', #32413, #71989, #93295 ) ;
#64271 = CARTESIAN_POINT ( 'NONE',  ( -42.49914285597344588, -24.15543982623907127, -0.2315651400026575435 ) ) ;
#64272 = CARTESIAN_POINT ( 'NONE',  ( -71.58953762381672448, -23.47593901973091235, -1.443836447539006196 ) ) ;
#64273 = APPROVAL_ROLE ( '' ) ;
#64274 = CARTESIAN_POINT ( 'NONE',  ( -60.52287095715006160, -24.91570333826269490, 8.075032458230454679 ) ) ;
#64275 = CARTESIAN_POINT ( 'NONE',  ( -39.04717358288242934, -25.28743336242031958, 4.335731970569660199 ) ) ;
#64276 = CARTESIAN_POINT ( 'NONE',  ( -16.38011734009650411, 12.53836025512309149, 11.49999999999999645 ) ) ;
#64277 = CARTESIAN_POINT ( 'NONE',  ( 4.329581153495547063, -6.376774720514422512, 21.24220543808225869 ) ) ;
#64278 = DIRECTION ( 'NONE',  ( -3.773278334453079618E-23, 0.9999999999976377785, 2.173523156925979975E-06 ) ) ;
#64279 = CARTESIAN_POINT ( 'NONE',  ( -8.190886813464794969, 21.05079722441571732, 11.49999999999999645 ) ) ;
#64280 = ORIENTED_EDGE ( 'NONE', *, *, #84067, .T. ) ;
#64281 = CARTESIAN_POINT ( 'NONE',  ( -69.41396772704672458, -25.12219025450763255, 6.552775786966387628 ) ) ;
#64282 = FACE_OUTER_BOUND ( 'NONE', #91996, .T. ) ;
#64283 = CARTESIAN_POINT ( 'NONE',  ( -97.50711219967668342, -24.65952944569304606, 1.056160979905701680 ) ) ;
#64284 = CARTESIAN_POINT ( 'NONE',  ( -126.5228709571500616, -23.47593901973090524, -1.443836447538996204 ) ) ;
#64285 = EDGE_CURVE ( 'NONE', #29436, #41575, #93671, .T. ) ;
#64286 = CARTESIAN_POINT ( 'NONE',  ( -27.70544111104076990, -24.61460113826161944, 8.251826784989919616 ) ) ;
#64287 = DIRECTION ( 'NONE',  ( 1.000000000000000000, 3.773278334444166432E-23, 8.201307841325785021E-29 ) ) ;
#64288 = VECTOR ( 'NONE', #3105, 1000.000000000000000 ) ;
#64289 = ADVANCED_FACE ( 'NONE', ( #27936 ), #65033, .F. ) ;
#64290 = ORIENTED_EDGE ( 'NONE', *, *, #78866, .F. ) ;
#64291 = CARTESIAN_POINT ( 'NONE',  ( 22.28998074345494729, -6.091270044117925053, 11.49999999999999645 ) ) ;
#64292 = CARTESIAN_POINT ( 'NONE',  ( -21.74551633039419585, 6.958787177381512201, -1.500000000000002220 ) ) ;
#64293 = CARTESIAN_POINT ( 'NONE',  ( -100.4326965455115044, -25.18492896333868103, 3.293943116708551777 ) ) ;
#64294 = CARTESIAN_POINT ( 'NONE',  ( -115.5228709571500190, -24.62285846331437966, 9.038163153548229189 ) ) ;
#64295 = CARTESIAN_POINT ( 'NONE',  ( -82.59550797413433543, -23.96169478059713143, 10.65365249895718414 ) ) ;
#64296 = CARTESIAN_POINT ( 'NONE',  ( 20.54305097139451064, 9.177977666691313985, 11.49999999999999645 ) ) ;
#64297 = ORIENTED_EDGE ( 'NONE', *, *, #3918, .F. ) ;
#64298 = CARTESIAN_POINT ( 'NONE',  ( -43.58705352746476791, -24.34968618360933590, 0.1864209137778851388 ) ) ;
#64299 = CARTESIAN_POINT ( 'NONE',  ( 10.99670386783381737, -19.00842362925918749, -1.500000000000002220 ) ) ;
#64300 = CARTESIAN_POINT ( 'NONE',  ( -81.62287095715005592, -29.50250243563736774, 8.947779886222141599 ) ) ;
#64301 = CARTESIAN_POINT ( 'NONE',  ( -34.57521954910300366, -24.66019654487199730, 8.947790411086117501 ) ) ;
#64302 = CARTESIAN_POINT ( 'NONE',  ( -69.63426884387564542, -25.06829995203217720, 7.393698517222913935 ) ) ;
#64303 = ORIENTED_EDGE ( 'NONE', *, *, #16101, .T. ) ;
#64304 = DIRECTION ( 'NONE',  ( -0.000000000000000000, -1.000000000000000000, -0.000000000000000000 ) ) ;
#64305 = ADVANCED_FACE ( 'NONE', ( #50285 ), #41681, .T. ) ;
#64306 = PLANE ( 'NONE',  #13786 ) ;
#64307 = ORIENTED_EDGE ( 'NONE', *, *, #44864, .F. ) ;
#64308 = VECTOR ( 'NONE', #66077, 1000.000000000000000 ) ;
#64309 = CARTESIAN_POINT ( 'NONE',  ( -19.72667040167412722, -5.651925516699977337, 11.49999999999998934 ) ) ;
#64310 = ORIENTED_EDGE ( 'NONE', *, *, #98670, .T. ) ;
#64311 = AXIS2_PLACEMENT_3D ( 'NONE', #26492, #9754, #17368 ) ;
#64312 = ORIENTED_EDGE ( 'NONE', *, *, #89211, .T. ) ;
#64313 = ORIENTED_EDGE ( 'NONE', *, *, #79555, .F. ) ;
#64314 = B_SPLINE_CURVE_WITH_KNOTS ( 'NONE', 3,
 ( #20114, #42972, #73908, #82019 ),
 .UNSPECIFIED., .F., .F.,
 ( 4, 4 ),
 ( 0.000000000000000000, 9.999999999998897304E-05 ),
 .UNSPECIFIED. ) ;
#64315 = ORIENTED_EDGE ( 'NONE', *, *, #50633, .F. ) ;
#64316 = CARTESIAN_POINT ( 'NONE',  ( -50.37830952628071657, -25.31401921878212136, 5.197788989978542773 ) ) ;
#64317 = CARTESIAN_POINT ( 'NONE',  ( 1.767912858038628965, -23.04938964843747584, -1.500000000000002220 ) ) ;
#64318 = CARTESIAN_POINT ( 'NONE',  ( -116.6228709571500559, -29.50250786944525672, 11.44777988621622811 ) ) ;
#64319 = CARTESIAN_POINT ( 'NONE',  ( 6.737473828552405841, -19.20966278261563076, -1.500000000000002220 ) ) ;
#64320 = ADVANCED_FACE ( 'NONE', ( #88343 ), #96948, .T. ) ;
#64321 = ORIENTED_EDGE ( 'NONE', *, *, #84929, .F. ) ;
#64322 = DIRECTION ( 'NONE',  ( 0.06283980576413537855, 0.000000000000000000, 0.9980236263794188822 ) ) ;
#64323 = CARTESIAN_POINT ( 'NONE',  ( -29.63599055435521024, -24.27518589826293649, 9.817618405055078767 ) ) ;
#64324 = CIRCLE ( 'NONE', #9162, 1.000000000000000000 ) ;
#64325 = CARTESIAN_POINT ( 'NONE',  ( -114.6228709571500701, -23.73934037231757799, 11.05740245334328442 ) ) ;
#64326 = CARTESIAN_POINT ( 'NONE',  ( 4.547289707988324103, -5.876774720514410966, 19.12266226838056582 ) ) ;
#64328 = ORIENTED_EDGE ( 'NONE', *, *, #28018, .F. ) ;
#64327 = CARTESIAN_POINT ( 'NONE',  ( -10.32266838563235467, 18.89866041204108527, 11.49999999999999645 ) ) ;
#64329 = CARTESIAN_POINT ( 'NONE',  ( -29.24616400714660003, -25.21532219221842652, 4.855716927727858234 ) ) ;
#64330 = PLANE ( 'NONE',  #10253 ) ;
#64331 = ORIENTED_EDGE ( 'NONE', *, *, #53424, .T. ) ;
#64332 = CARTESIAN_POINT ( 'NONE',  ( -20.73834036848188234, 1.213307192923735345, 11.49999999999998934 ) ) ;
#64333 = ORIENTED_EDGE ( 'NONE', *, *, #23925, .T. ) ;
#64334 = CC_DESIGN_PERSON_AND_ORGANIZATION_ASSIGNMENT ( #31149, #38757, ( #78135 ) ) ;
#64336 = ORIENTED_EDGE ( 'NONE', *, *, #45124, .F. ) ;
#64335 = CARTESIAN_POINT ( 'NONE',  ( -125.6241961315440534, -24.63355581998386512, 0.9682620441944075340 ) ) ;
#64337 = CARTESIAN_POINT ( 'NONE',  ( -47.62287095715004881, -23.48783264082478084, -1.443836473390070596 ) ) ;
#64338 = PLANE ( 'NONE',  #92416 ) ;
#64339 = ORIENTED_EDGE ( 'NONE', *, *, #4539, .T. ) ;
#64340 = VERTEX_POINT ( 'NONE', #89835 ) ;
#64341 = CARTESIAN_POINT ( 'NONE',  ( -5.970505764849975527, -5.876774720514411854, 19.55848054040323802 ) ) ;
#64342 = CARTESIAN_POINT ( 'NONE',  ( -129.5228709571500758, -29.50248528299804818, 1.056150453629047137 ) ) ;
#64343 = CARTESIAN_POINT ( 'NONE',  ( -78.52287095715001897, -24.33832256527049154, 0.1851278514138635367 ) ) ;
#64345 = ORIENTED_EDGE ( 'NONE', *, *, #68246, .F. ) ;
#64344 = CARTESIAN_POINT ( 'NONE',  ( 21.30657626330824783, 5.479626006175059239, 11.49999999999999645 ) ) ;
#64346 = CARTESIAN_POINT ( 'NONE',  ( -103.5530519847491178, -24.15543982623907482, -0.2315651400026619011 ) ) ;
#64347 = CARTESIAN_POINT ( 'NONE',  ( 10.27952223434480494, 20.12118371629609470, -1.500000000000002220 ) ) ;
#64348 = AXIS2_PLACEMENT_3D ( 'NONE', #6750, #98097, #61561 ) ;
#64350 = ORIENTED_EDGE ( 'NONE', *, *, #7060, .T. ) ;
#64349 = LINE ( 'NONE', #1930, #84683 ) ;
#64351 = VERTEX_POINT ( 'NONE', #34557 ) ;
#64352 = VECTOR ( 'NONE', #75791, 1000.000000000000000 ) ;
#64353 = CARTESIAN_POINT ( 'NONE',  ( -88.52287095715006160, -23.48786465467241769, 11.44779295918254292 ) ) ;
#64354 = B_SPLINE_CURVE_WITH_KNOTS ( 'NONE', 3,
 ( #83006, #50091, #20121, #66324, #12507, #43472, #34856, #13496, #97744, #72925, #74411, #4904, #35850, #3426, #34359, #96257 ),
 .UNSPECIFIED., .F., .F.,
 ( 4, 2, 2, 2, 2, 2, 2, 4 ),
 ( 0.000000000000000000, 0.0001832628685938118200, 0.0003665257371876236400, 0.0005497886057814354872, 0.0007330514743752472801, 0.001099577211562870974, 0.001282840080156677455, 0.001466102948750484152 ),
 .UNSPECIFIED. ) ;
#64355 = CARTESIAN_POINT ( 'NONE',  ( -36.58953762381673158, -24.64965694238406613, 8.947790433994660120 ) ) ;
#64356 = ORIENTED_EDGE ( 'NONE', *, *, #67108, .F. ) ;
#64357 = CARTESIAN_POINT ( 'NONE',  ( -17.86006801910157193, 11.38285951858322242, 11.49999999999998934 ) ) ;
#64358 = FACE_OUTER_BOUND ( 'NONE', #53880, .T. ) ;
#64359 = CARTESIAN_POINT ( 'NONE',  ( 29.70909950603835625, -4.224653874731083114, 27.99670097642948008 ) ) ;
#64360 = CARTESIAN_POINT ( 'NONE',  ( -6.815415664272417295, -5.876774720514410077, 19.46427715384223234 ) ) ;
#64361 = DIRECTION ( 'NONE',  ( 3.773278334444167608E-23, -1.000000000000000000, 0.000000000000000000 ) ) ;
#64362 = CARTESIAN_POINT ( 'NONE',  ( 21.18294168759468832, 6.642818831845659133, -1.500000000000002220 ) ) ;
#64363 = CARTESIAN_POINT ( 'NONE',  ( -114.5882204601105059, -24.51314013834316086, 0.6176544820404237246 ) ) ;
#64364 = EDGE_CURVE ( 'NONE', #32410, #65068, #36045, .T. ) ;
#64365 = VERTEX_POINT ( 'NONE', #43175 ) ;
#64366 = CARTESIAN_POINT ( 'NONE',  ( -79.92287095715005307, -23.47596703998600631, 11.44779298504227860 ) ) ;
#64367 = CARTESIAN_POINT ( 'NONE',  ( -19.80875734969026425, -0.3587747205144265483, 30.51402280011862089 ) ) ;
#64368 = CARTESIAN_POINT ( 'NONE',  ( -12.45040968399260883, -14.89389333286084671, 11.49999999999999645 ) ) ;
#64369 = AXIS2_PLACEMENT_3D ( 'NONE', #13525, #89672, #67341 ) ;
#64370 = CARTESIAN_POINT ( 'NONE',  ( -41.15367109091464215, -25.13982731016471917, 3.000623932295935159 ) ) ;
#64371 = LINE ( 'NONE', #9050, #68015 ) ;
#64372 = CARTESIAN_POINT ( 'NONE',  ( 17.91360334016800593, 7.682165803940314674, -1.500000000000002220 ) ) ;
#64373 = ADVANCED_FACE ( 'NONE', ( #11214 ), #95947, .F. ) ;
#64374 = CARTESIAN_POINT ( 'NONE',  ( 13.27131465344908001, -16.79725507166503462, -1.500000000000002220 ) ) ;
#64375 = CARTESIAN_POINT ( 'NONE',  ( -32.55620429048337172, -24.64965694238574301, 8.947790433994212478 ) ) ;
#64376 = CARTESIAN_POINT ( 'NONE',  ( -60.50379446447523435, -24.15602025861357660, 10.28564288302606933 ) ) ;
#64377 = EDGE_CURVE ( 'NONE', #47734, #41964, #20304, .T. ) ;
#64378 = LINE ( 'NONE', #17167, #66543 ) ;
#64379 = DIRECTION ( 'NONE',  ( -3.773278334453079618E-23, 0.9999999999976377785, 2.173523156925979975E-06 ) ) ;
#64380 = CARTESIAN_POINT ( 'NONE',  ( -13.93578158028743985, 17.96481793202167054, -1.500000000000002220 ) ) ;
#64381 = AXIS2_PLACEMENT_3D ( 'NONE', #90839, #5102, #99438 ) ;
#64382 = DIRECTION ( 'NONE',  ( -1.000000000000000000, 0.000000000000000000, 0.000000000000000000 ) ) ;
#64383 = AXIS2_PLACEMENT_3D ( 'NONE', #26127, #64725, #19507 ) ;
#64384 = CARTESIAN_POINT ( 'NONE',  ( -106.6264150236442134, -24.35071581493544457, 9.817618358456019934 ) ) ;
#64385 = DIRECTION ( 'NONE',  ( 0.000000000000000000, 1.000000000000000000, 0.000000000000000000 ) ) ;
#64386 = CARTESIAN_POINT ( 'NONE',  ( -19.77041435686880533, -2.435487021107205940, 11.49999999999999645 ) ) ;
#64387 = CARTESIAN_POINT ( 'NONE',  ( 5.400898774349120579, -6.376774720514417183, 20.36357656736558042 ) ) ;
#64388 = VECTOR ( 'NONE', #89898, 1000.000000000000000 ) ;
#64389 = DIRECTION ( 'NONE',  ( 0.000000000000000000, 0.000000000000000000, -1.000000000000000000 ) ) ;
#64390 = CARTESIAN_POINT ( 'NONE',  ( -51.22287095715007155, -23.47593901973090169, -1.443836447538997758 ) ) ;
#64391 = ORIENTED_EDGE ( 'NONE', *, *, #59098, .F. ) ;
#64392 = EDGE_CURVE ( 'NONE', #42928, #44309, #26448, .T. ) ;
#64393 = CARTESIAN_POINT ( 'NONE',  ( -49.58084058178877029, -25.16964401093727943, 6.816005909056730871 ) ) ;
#64394 = CARTESIAN_POINT ( 'NONE',  ( -31.80980768408297266, -25.31600595412499644, 6.101236642668423471 ) ) ;
#64395 = CARTESIAN_POINT ( 'NONE',  ( -117.6228709571500701, -24.66019654487199730, 8.947790411086121054 ) ) ;
#64396 = CARTESIAN_POINT ( 'NONE',  ( -7.614213781628100364, -20.28429660096114517, 11.49999999999998934 ) ) ;
#64397 = CARTESIAN_POINT ( 'NONE',  ( -4.700032041049139409, -6.144890974841530351, 9.000000000000000000 ) ) ;
#64398 = CARTESIAN_POINT ( 'NONE',  ( 18.23270504744370868, -6.907985942191454676, -1.500000000000002220 ) ) ;
#64399 = CARTESIAN_POINT ( 'NONE',  ( -67.62287095715008434, -23.47596703998600276, 11.44779298504227505 ) ) ;
#64400 = VERTEX_POINT ( 'NONE', #80730 ) ;
#64401 = PLANE ( 'NONE',  #88893 ) ;
#64402 = CARTESIAN_POINT ( 'NONE',  ( -19.36681041099238598, 6.328833669845586485, 11.49999999999999645 ) ) ;
#64403 = DIRECTION ( 'NONE',  ( 0.000000000000000000, -1.478457507934778393E-16, -1.000000000000000000 ) ) ;
#64404 = CARTESIAN_POINT ( 'NONE',  ( -60.91704397828815587, -25.27796947198809363, 6.054720049563738549 ) ) ;
#64405 = ORIENTED_EDGE ( 'NONE', *, *, #36640, .F. ) ;
#64406 = CARTESIAN_POINT ( 'NONE',  ( -41.46611000704998418, -25.28830591450888932, 4.188173661249235735 ) ) ;
#64407 = LINE ( 'NONE', #10087, #16902 ) ;
#64408 = CARTESIAN_POINT ( 'NONE',  ( -49.22287095715006444, -23.47596703998600276, 11.44779298504227683 ) ) ;
#64409 = CARTESIAN_POINT ( 'NONE',  ( -49.27764846858840997, -25.25138878606429671, 6.145204991494091828 ) ) ;
#64410 = CARTESIAN_POINT ( 'NONE',  ( -1.044639546681034536, -5.876774720514417183, 20.34213149456667580 ) ) ;
#64411 = CARTESIAN_POINT ( 'NONE',  ( -109.5877490058777539, -24.51314013834315730, 0.6176544820404190617 ) ) ;
#64412 = ORIENTED_EDGE ( 'NONE', *, *, #7932, .F. ) ;
#64413 = CARTESIAN_POINT ( 'NONE',  ( -66.54009212403214235, -24.51419770103157347, 9.386484678747176957 ) ) ;
#64414 = VECTOR ( 'NONE', #37090, 1000.000000000000000 ) ;
#64415 = ADVANCED_FACE ( 'NONE', ( #42187 ), #43666, .T. ) ;
#64416 = CARTESIAN_POINT ( 'NONE',  ( 19.50756536182865020, -12.10693203178887423, 11.49999999999999645 ) ) ;
#64417 = CARTESIAN_POINT ( 'NONE',  ( 0.6941480231959694658, 22.73124288027050710, -1.500000000000002220 ) ) ;
#64418 = CARTESIAN_POINT ( 'NONE',  ( 4.465438306463536122, -6.376774720514426065, 21.59631214011467293 ) ) ;
#64419 = B_SPLINE_SURFACE_WITH_KNOTS ( 'NONE', 3, 1, ( 
 ( #6041, #21253 ),
 ( #35509, #82169 ),
 ( #52227, #35992 ),
 ( #83157, #20257 ),
 ( #97878, #13142 ),
 ( #5045, #44114 ),
 ( #59335, #84157 ),
 ( #66966, #90284 ),
 ( #20755, #43616 ),
 ( #99381, #36992 ),
 ( #51225, #74557 ),
 ( #74067, #67453 ),
 ( #22247, #14142 ),
 ( #13641, #53229 ) ),
 .UNSPECIFIED., .F., .F., .F.,
 ( 4, 2, 2, 2, 2, 2, 4 ),
 ( 2, 2 ),
 ( 0.000000000000000000, 0.2499999999999996114, 0.3749999999999996669, 0.4999999999999997780, 0.6249999999999998890, 0.7499999999999998890, 1.000000000000000000 ),
 ( 0.000000000000000000, 1.000000000000000000 ),
 .UNSPECIFIED. ) ;
#64420 = CARTESIAN_POINT ( 'NONE',  ( 33.23241444531825550, 3.542570809989110447, -12.77295888271925328 ) ) ;
#64421 = CARTESIAN_POINT ( 'NONE',  ( -90.58192396404253088, -25.00158670708910691, 2.256160236439220590 ) ) ;
#64422 = AXIS2_PLACEMENT_3D ( 'NONE', #9674, #78657, #72089 ) ;
#64423 = CARTESIAN_POINT ( 'NONE',  ( -69.55365840088312268, -25.18627906957131657, 6.773493112845361708 ) ) ;
#64424 = CARTESIAN_POINT ( 'NONE',  ( -18.33957545910867282, 11.93505917737106259, 11.49999999999998934 ) ) ;
#64425 = CARTESIAN_POINT ( 'NONE',  ( -70.52287095715007581, -24.99132157543166599, 2.256160258750667502 ) ) ;
#64426 = ADVANCED_FACE ( 'NONE', ( #73124 ), #96448, .F. ) ;
#64427 = CARTESIAN_POINT ( 'NONE',  ( 2.100208336950355914, 1.530808498934186394E-16, -1.249999999999996003 ) ) ;
#64428 = CARTESIAN_POINT ( 'NONE',  ( -122.5885215633497296, -24.65952944569305316, 1.056160979905708786 ) ) ;
#64429 = CARTESIAN_POINT ( 'NONE',  ( -8.676776695296460673, 18.57322330470351091, 2.100000000000000089 ) ) ;
#64430 = ORIENTED_EDGE ( 'NONE', *, *, #15243, .F. ) ;
#64431 = PRODUCT_DEFINITION_SHAPE ( 'NONE', 'NONE',  #10919 ) ;
#64432 = CARTESIAN_POINT ( 'NONE',  ( -15.55180764702766716, 13.24544322234432414, -1.500000000000002220 ) ) ;
#64433 = VERTEX_POINT ( 'NONE', #19808 ) ;
#64434 = ORIENTED_EDGE ( 'NONE', *, *, #84192, .T. ) ;
#64435 = CARTESIAN_POINT ( 'NONE',  ( 22.64363655503811046, -4.068770074275382953, 11.49999999999998934 ) ) ;
#64436 = DIRECTION ( 'NONE',  ( -1.000000000000000000, -3.773278334444167608E-23, -8.201307833595939069E-29 ) ) ;
#64437 = B_SPLINE_CURVE_WITH_KNOTS ( 'NONE', 3,
 ( #25540, #65129, #42295, #73223, #3713, #58009 ),
 .UNSPECIFIED., .F., .F.,
 ( 4, 2, 4 ),
 ( 0.000000000000000000, 0.001380764517854765399, 0.002761529035709530799 ),
 .UNSPECIFIED. ) ;
#64438 = ORIENTED_EDGE ( 'NONE', *, *, #28127, .T. ) ;
#64439 = CARTESIAN_POINT ( 'NONE',  ( -94.52287095715006160, -29.50248528299804818, 1.056150453629040253 ) ) ;
#64440 = VECTOR ( 'NONE', #49502, 1000.000000000000114 ) ;
#64441 = CARTESIAN_POINT ( 'NONE',  ( -32.55620429048339304, -24.65952944569304606, 1.056160979905692132 ) ) ;
#64442 = CARTESIAN_POINT ( 'NONE',  ( -98.62287095715005592, -23.48786465467241769, 11.44779295918254292 ) ) ;
#64443 = PLANE ( 'NONE',  #90143 ) ;
#64445 = ORIENTED_EDGE ( 'NONE', *, *, #67524, .T. ) ;
#64444 = CARTESIAN_POINT ( 'NONE',  ( 15.78869406909177897, -14.30566568001193950, 11.49999999999999645 ) ) ;
#64446 = EDGE_LOOP ( 'NONE', ( #58439, #4051, #41293, #90878 ) ) ;
#64447 = CARTESIAN_POINT ( 'NONE',  ( 12.24756355222007898, 18.56953561607567238, 11.49999999999998934 ) ) ;
#64448 = CARTESIAN_POINT ( 'NONE',  ( 20.52162115075873672, 2.272738508513782119, 11.49999999999998934 ) ) ;
#64449 = EDGE_CURVE ( 'NONE', #18728, #38938, #38627, .T. ) ;
#64450 = AXIS2_PLACEMENT_3D ( 'NONE', #41583, #5005, #89245 ) ;
#64451 = EDGE_LOOP ( 'NONE', ( #34103, #90769, #36851, #57463 ) ) ;
#64452 = CARTESIAN_POINT ( 'NONE',  ( -6.499903988472228278, -5.876774720514408301, 19.18381548539529646 ) ) ;
#64453 = DIRECTION ( 'NONE',  ( -0.000000000000000000, 1.000000000000000000, -0.000000000000000000 ) ) ;
#64454 = ORIENTED_EDGE ( 'NONE', *, *, #76929, .T. ) ;
#64455 = CARTESIAN_POINT ( 'NONE',  ( -65.62287095715005592, -25.00158670708909270, 2.256160236439166855 ) ) ;
#64456 = VECTOR ( 'NONE', #98881, 1000.000000000000000 ) ;
#64457 = ORIENTED_EDGE ( 'NONE', *, *, #57699, .T. ) ;
#64458 = FACE_OUTER_BOUND ( 'NONE', #58200, .T. ) ;
#64459 = CARTESIAN_POINT ( 'NONE',  ( -71.30457154551152144, -25.24554880456021522, 6.209207408033732278 ) ) ;
#64460 = CARTESIAN_POINT ( 'NONE',  ( 12.78316523911058944, -16.47895720935621711, -1.500000000000002220 ) ) ;
#64461 = CARTESIAN_POINT ( 'NONE',  ( -15.20188179817220231, 15.67080601223297442, 11.49999999999999645 ) ) ;
#64462 = CARTESIAN_POINT ( 'NONE',  ( -73.58796373308013017, -24.35071581493543036, 9.817618358456027039 ) ) ;
#64463 = CARTESIAN_POINT ( 'NONE',  ( -75.62287095715005592, -29.50247984919015209, -1.443849546365053582 ) ) ;
#64464 = CARTESIAN_POINT ( 'NONE',  ( -20.52357230491503159, 9.176553703681571861, -1.500000000000002220 ) ) ;
#64465 = EDGE_CURVE ( 'NONE', #57808, #14974, #12198, .T. ) ;
#64466 = EDGE_CURVE ( 'NONE', #21027, #3669, #19179, .T. ) ;
#64467 = CARTESIAN_POINT ( 'NONE',  ( -8.531171415479239073, -19.09552649099111221, -1.500000000000002220 ) ) ;
#64468 = CARTESIAN_POINT ( 'NONE',  ( -26.15327376889522526, -24.97066975962406943, 5.797585818533663726 ) ) ;
#64469 = DIRECTION ( 'NONE',  ( -0.06975647374412549673, -0.9975640502598241977, 0.000000000000000000 ) ) ;
#64470 = DIRECTION ( 'NONE',  ( 0.000000000000000000, 0.000000000000000000, 1.000000000000000000 ) ) ;
#64471 = ORIENTED_EDGE ( 'NONE', *, *, #35955, .F. ) ;
#64472 = ORIENTED_EDGE ( 'NONE', *, *, #63936, .T. ) ;
#64473 = ORIENTED_EDGE ( 'NONE', *, *, #28695, .F. ) ;
#64474 = DIRECTION ( 'NONE',  ( 0.000000000000000000, 0.000000000000000000, 1.000000000000000000 ) ) ;
#64475 = ORIENTED_EDGE ( 'NONE', *, *, #35936, .T. ) ;
#64476 = CARTESIAN_POINT ( 'NONE',  ( 21.30238844577196389, 2.035401582669650544, -1.500000000000002220 ) ) ;
#64477 = CARTESIAN_POINT ( 'NONE',  ( -20.28323820415832657, -9.445149539555593776, 11.49999999999999645 ) ) ;
#64478 = EDGE_LOOP ( 'NONE', ( #30926, #11013, #32637, #53065 ) ) ;
#64479 = CARTESIAN_POINT ( 'NONE',  ( -28.55620429048338949, -23.31442300727656658, 11.44779301120574999 ) ) ;
#64480 = CARTESIAN_POINT ( 'NONE',  ( 8.294003578737715543, -19.35633765900385939, 11.49999999999998934 ) ) ;
#64481 = CARTESIAN_POINT ( 'NONE',  ( -30.51821509024741275, -25.31107878299565783, 5.002391647799127483 ) ) ;
#64482 = CARTESIAN_POINT ( 'NONE',  ( 10.08953278062578462, 17.19620541797624824, -1.500000000000002220 ) ) ;
#64483 = CARTESIAN_POINT ( 'NONE',  ( 1.600000000000000755, 2.363568322354391830E-15, -19.30000000000000071 ) ) ;
#64484 = CARTESIAN_POINT ( 'NONE',  ( -122.6228709571500417, -23.47596703998600631, 11.44779298504227860 ) ) ;
#64485 = CARTESIAN_POINT ( 'NONE',  ( -21.82725030464235516, 2.967780500094957308, -1.500000000000002220 ) ) ;
#64486 = ORIENTED_EDGE ( 'NONE', *, *, #21717, .T. ) ;
#64487 = CARTESIAN_POINT ( 'NONE',  ( -116.5914121302601387, -23.96119346886881729, -0.6495511937831833782 ) ) ;
#64488 = EDGE_CURVE ( 'NONE', #26504, #26877, #19315, .T. ) ;
#64489 = LINE ( 'NONE', #79170, #15721 ) ;
#64490 = CARTESIAN_POINT ( 'NONE',  ( -40.76794460738368997, -25.31624736906593043, 5.521532656993860755 ) ) ;
#64491 = AXIS2_PLACEMENT_3D ( 'NONE', #74053, #36480, #51216 ) ;
#64492 = CARTESIAN_POINT ( 'NONE',  ( -62.59791734348949177, -23.96169478059712432, 10.65365249895718414 ) ) ;
#64493 = DIRECTION ( 'NONE',  ( -0.000000000000000000, -1.000000000000000000, -0.000000000000000000 ) ) ;
#64494 = CARTESIAN_POINT ( 'NONE',  ( -48.58953762381673158, -23.47593901973091235, -1.443836447539009749 ) ) ;
#64495 = CARTESIAN_POINT ( 'NONE',  ( -4.607724273132460802, 20.83226218841027944, -1.500000000000002220 ) ) ;
#64496 = FACE_OUTER_BOUND ( 'NONE', #40452, .T. ) ;
#64497 = LINE ( 'NONE', #24890, #38182 ) ;
#64498 = EDGE_CURVE ( 'NONE', #85110, #6180, #85678, .T. ) ;
#64499 = CARTESIAN_POINT ( 'NONE',  ( -29.49875734969025842, 5.965225279485572685, 23.37402280011862743 ) ) ;
#64500 = LINE ( 'NONE', #49761, #52461 ) ;
#64501 = CARTESIAN_POINT ( 'NONE',  ( 2.010693963185784749, 22.50221635003889276, -1.500000000000002220 ) ) ;
#64502 = B_SPLINE_SURFACE_WITH_KNOTS ( 'NONE', 3, 3, ( 
 ( #98037, #20408, #74704, #28050 ),
 ( #4213, #13300, #13799, #6198 ),
 ( #90935, #68112, #99032, #21407 ),
 ( #89941, #12801, #35167, #5202 ),
 ( #52383, #19429, #50394, #73718 ),
 ( #97053, #27556, #58510, #89447 ),
 ( #50892, #28533, #81831, #12303 ) ),
 .UNSPECIFIED., .F., .F., .F.,
 ( 4, 3, 4 ),
 ( 4, 4 ),
 ( 0.0004766839783823902305, 0.1029713700210900945, 0.2054660560637978084 ),
 ( 0.1195244022139620860, 0.1205922751095607898 ),
 .UNSPECIFIED. ) ;
#64503 = EDGE_CURVE ( 'NONE', #49066, #52201, #12694, .T. ) ;
#64504 = DIRECTION ( 'NONE',  ( 0.000000000000000000, 0.000000000000000000, 1.000000000000000000 ) ) ;
#64505 = ORIENTED_EDGE ( 'NONE', *, *, #7945, .F. ) ;
#64506 = DIRECTION ( 'NONE',  ( -3.773278334453079030E-23, 0.9999999999976377785, 2.173523156925979128E-06 ) ) ;
#64507 = CARTESIAN_POINT ( 'NONE',  ( -122.6228709571500417, -24.50216790748098461, 0.6166512839513762501 ) ) ;
#64508 = CARTESIAN_POINT ( 'NONE',  ( -15.16444148636751521, -12.51942901160708921, 11.49999999999999645 ) ) ;
#64509 = PLANE ( 'NONE',  #40656 ) ;
#64510 = CARTESIAN_POINT ( 'NONE',  ( -73.52287095715011844, -23.95044443724992789, 10.65354141964649415 ) ) ;
#64511 = ORIENTED_EDGE ( 'NONE', *, *, #27441, .F. ) ;
#64512 = EDGE_CURVE ( 'NONE', #55708, #90958, #36539, .T. ) ;
#64513 = CARTESIAN_POINT ( 'NONE',  ( -79.62632635320380814, -25.21083105912962097, 3.409327675794635581 ) ) ;
#64514 = DIRECTION ( 'NONE',  ( -3.773278334453079030E-23, 0.9999999999976377785, 2.173523156925979128E-06 ) ) ;
#64515 = LINE ( 'NONE', #1082, #22059 ) ;
#64516 = DIRECTION ( 'NONE',  ( 0.000000000000000000, 0.9999999999976377785, 2.173523156925979975E-06 ) ) ;
#64517 = AXIS2_PLACEMENT_3D ( 'NONE', #23520, #24033, #15919 ) ;
#64518 = CARTESIAN_POINT ( 'NONE',  ( -120.5562042904834072, -24.99132157543166954, 2.256160258750667946 ) ) ;
#64519 = EDGE_CURVE ( 'NONE', #41620, #29468, #1037, .T. ) ;
#64520 = DIRECTION ( 'NONE',  ( 0.000000000000000000, 0.000000000000000000, 1.000000000000000000 ) ) ;
#64521 = CARTESIAN_POINT ( 'NONE',  ( -17.60924879254659459, 8.996216891746938060, 11.49999999999998934 ) ) ;
#64522 = VERTEX_POINT ( 'NONE', #37546 ) ;
#64523 = CARTESIAN_POINT ( 'NONE',  ( 8.007726535620864894, 18.53121347637897287, 11.49999999999999645 ) ) ;
#64524 = CARTESIAN_POINT ( 'NONE',  ( -7.536766146225033047, -5.876774720514412742, 19.63296556618507438 ) ) ;
#64525 = VECTOR ( 'NONE', #68540, 1000.000000000000000 ) ;
#64526 = ORIENTED_EDGE ( 'NONE', *, *, #23411, .F. ) ;
#64527 = DIRECTION ( 'NONE',  ( -0.000000000000000000, 1.000000000000000000, -0.000000000000000000 ) ) ;
#64528 = CARTESIAN_POINT ( 'NONE',  ( -80.85529437621991633, -25.30559667752245900, 5.016674165721909162 ) ) ;
#64529 = CARTESIAN_POINT ( 'NONE',  ( 27.53860345374808105, -1.682774720514426114, -1.272392034746785860 ) ) ;
#64530 = DIRECTION ( 'NONE',  ( -0.000000000000000000, 2.173523156925979552E-06, -0.9999999999976378895 ) ) ;
#64531 = AXIS2_PLACEMENT_3D ( 'NONE', #29997, #1066, #53356 ) ;
#64532 = CARTESIAN_POINT ( 'NONE',  ( -39.62287095715007723, -24.34917612406837861, 0.1852690917426592920 ) ) ;
#64533 = B_SPLINE_CURVE_WITH_KNOTS ( 'NONE', 3,
 ( #8590, #9084, #39539, #48673, #63398, #40037 ),
 .UNSPECIFIED., .F., .F.,
 ( 4, 2, 4 ),
 ( 1.571618716487580835E-05, 0.001396934050510501013, 0.002778151913856126160 ),
 .UNSPECIFIED. ) ;
#64534 = DIRECTION ( 'NONE',  ( 1.000000000000000000, 4.088963247170718308E-15, 0.000000000000000000 ) ) ;
#64535 = CARTESIAN_POINT ( 'NONE',  ( -11.57650325489309395, -16.32560983125179277, -1.500000000000002220 ) ) ;
#64536 = CARTESIAN_POINT ( 'NONE',  ( -99.16315266720698673, -25.10935227823729576, 3.707282584693533778 ) ) ;
#64537 = EDGE_LOOP ( 'NONE', ( #28766, #44332, #49121, #59675 ) ) ;
#64538 = ADVANCED_FACE ( 'NONE', ( #20806 ), #75097, .F. ) ;
#64539 = CARTESIAN_POINT ( 'NONE',  ( -103.5228709571500190, -23.73934037231756733, 11.05740245334328087 ) ) ;
#64540 = CARTESIAN_POINT ( 'NONE',  ( -24.57525087998973845, -5.965225279485572685, -15.45548830044932309 ) ) ;
#64541 = DIRECTION ( 'NONE',  ( -0.000000000000000000, -1.000000000000000000, -0.000000000000000000 ) ) ;
#64542 = DIRECTION ( 'NONE',  ( 0.000000000000000000, 0.9999999999976377785, 2.173523156925979975E-06 ) ) ;
#64543 = CARTESIAN_POINT ( 'NONE',  ( 0.4987820251299121543, -0.03487823687206274836, 9.000000000000000000 ) ) ;
#64544 = CARTESIAN_POINT ( 'NONE',  ( -45.55620429048337883, -23.47596703998600276, 11.44779298504227505 ) ) ;
#64545 = CARTESIAN_POINT ( 'NONE',  ( -101.9705984573116666, -25.11539320716599732, 2.804431449967498491 ) ) ;
#64546 = ORIENTED_EDGE ( 'NONE', *, *, #55981, .T. ) ;
#64547 = CARTESIAN_POINT ( 'NONE',  ( -20.32193514540556123, 0.06534614623005505218, -1.500000000000002220 ) ) ;
#64548 = VERTEX_POINT ( 'NONE', #90830 ) ;
#64549 = CARTESIAN_POINT ( 'NONE',  ( 29.64448763235240136, 5.625929005037784592, 28.17618604274316851 ) ) ;
#64550 = CARTESIAN_POINT ( 'NONE',  ( -127.6242802972114276, -23.96169478059713853, 10.65365249895716637 ) ) ;
#64551 = ORIENTED_EDGE ( 'NONE', *, *, #51502, .T. ) ;
#64552 = DIRECTION ( 'NONE',  ( -0.000000000000000000, 1.000000000000000000, -0.000000000000000000 ) ) ;
#64553 = CARTESIAN_POINT ( 'NONE',  ( -49.94169464672810221, -25.12215404331965019, 7.031228054708656749 ) ) ;
#64554 = CARTESIAN_POINT ( 'NONE',  ( -30.47287095715006799, -25.22866023116455381, 3.592313111342048337 ) ) ;
#64555 = CARTESIAN_POINT ( 'NONE',  ( 21.14167878903947084, -0.5806874866175276706, 11.49999999999999645 ) ) ;
#64556 = CARTESIAN_POINT ( 'NONE',  ( 21.55033589006239936, 5.121329677682045833, 11.49999999999998934 ) ) ;
#64557 = CARTESIAN_POINT ( 'NONE',  ( -1.452656003914881477, -20.50939586048694352, -1.500000000000002220 ) ) ;
#64558 = ADVANCED_FACE ( 'NONE', ( #14696 ), #28929, .F. ) ;
#64559 = VERTEX_POINT ( 'NONE', #91822 ) ;
#64560 = CARTESIAN_POINT ( 'NONE',  ( -113.6228709571500417, -23.47596703998600631, 11.44779298504227860 ) ) ;
#64561 = ORIENTED_EDGE ( 'NONE', *, *, #92157, .F. ) ;
#64562 = CARTESIAN_POINT ( 'NONE',  ( -54.60549243945573039, -23.73766607897669445, -1.055555164236461563 ) ) ;
#64563 = DIRECTION ( 'NONE',  ( -3.773278334444166432E-23, 1.000000000000000000, 0.000000000000000000 ) ) ;
#64564 = ORIENTED_EDGE ( 'NONE', *, *, #55584, .F. ) ;
#64565 = ORIENTED_EDGE ( 'NONE', *, *, #6793, .F. ) ;
#64566 = ORIENTED_EDGE ( 'NONE', *, *, #18721, .F. ) ;
#64567 = CARTESIAN_POINT ( 'NONE',  ( -103.5562042904834072, -23.48786465467241413, 11.44779295918253759 ) ) ;
#64568 = CARTESIAN_POINT ( 'NONE',  ( -29.22287093065927976, -23.36589167027821290, -1.443836447538997314 ) ) ;
#64569 = LINE ( 'NONE', #56446, #48780 ) ;
#64570 = CARTESIAN_POINT ( 'NONE',  ( -16.63904852704994042, -12.34428335884295969, -1.500000000000002220 ) ) ;
#64571 = B_SPLINE_CURVE_WITH_KNOTS ( 'NONE', 3,
 ( #92323, #46163, #15703, #85720, #46667, #39042 ),
 .UNSPECIFIED., .F., .F.,
 ( 4, 2, 4 ),
 ( 1.570887131794176733E-05, 0.001396322306279758037, 0.002776935741241574537 ),
 .UNSPECIFIED. ) ;
#64572 = CARTESIAN_POINT ( 'NONE',  ( 21.64940796807912449, -0.2623997510114038922, 11.49999999999999645 ) ) ;
#64573 = VERTEX_POINT ( 'NONE', #84206 ) ;
#64574 = EDGE_CURVE ( 'NONE', #37842, #58683, #76586, .T. ) ;
#64575 = CARTESIAN_POINT ( 'NONE',  ( 2.499999999999993783, 4.999999999999997335, 2.100000000000000089 ) ) ;
#64576 = CARTESIAN_POINT ( 'NONE',  ( -111.4314572179059866, -25.19203390433109746, 3.343237222027082289 ) ) ;
#64577 = CARTESIAN_POINT ( 'NONE',  ( 16.55124408090292576, 15.08944307983326638, -1.500000000000002220 ) ) ;
#64578 = EDGE_CURVE ( 'NONE', #41986, #26092, #24024, .T. ) ;
#64579 = VECTOR ( 'NONE', #99525, 1000.000000000000000 ) ;
#64580 = B_SPLINE_CURVE_WITH_KNOTS ( 'NONE', 3,
 ( #68045, #28966, #24237, #16618, #93244, #23731, #79018, #17123 ),
 .UNSPECIFIED., .F., .F.,
 ( 4, 2, 2, 4 ),
 ( 0.000000000000000000, 0.002001079623178221058, 0.003001619434767333321, 0.004002159246356445585 ),
 .UNSPECIFIED. ) ;
#64581 = EDGE_CURVE ( 'NONE', #45200, #30457, #6954, .T. ) ;
#64582 = DIRECTION ( 'NONE',  ( 1.000000000000000000, -0.000000000000000000, -0.000000000000000000 ) ) ;
#64583 = CARTESIAN_POINT ( 'NONE',  ( -61.62287095715004881, -24.64965695001468404, 8.947790433994185832 ) ) ;
#64584 = ORIENTED_EDGE ( 'NONE', *, *, #74077, .T. ) ;
#64585 = CARTESIAN_POINT ( 'NONE',  ( 29.67488939790761648, 5.972177877498852538, 27.69255262365155801 ) ) ;
#64586 = CARTESIAN_POINT ( 'NONE',  ( 11.94353453780502683, -5.048182838635504766, -26.89061828217040784 ) ) ;
#64587 = EDGE_CURVE ( 'NONE', #50385, #92857, #66183, .T. ) ;
#64588 = VERTEX_POINT ( 'NONE', #38040 ) ;
#64589 = EDGE_LOOP ( 'NONE', ( #19377, #43342, #91121, #82615 ) ) ;
#64590 = CARTESIAN_POINT ( 'NONE',  ( -46.63379005058555293, -24.35071581493542325, 9.817618358456032368 ) ) ;
#64591 = ORIENTED_EDGE ( 'NONE', *, *, #2709, .F. ) ;
#64592 = CARTESIAN_POINT ( 'NONE',  ( 16.26279755680689476, 5.965225279485572685, -27.67997040356619110 ) ) ;
#64593 = CARTESIAN_POINT ( 'NONE',  ( 3.248270302591931724, 20.98854991013365279, -1.500000000000002220 ) ) ;
#64594 = ORIENTED_EDGE ( 'NONE', *, *, #97424, .T. ) ;
#64595 = DIRECTION ( 'NONE',  ( 0.000000000000000000, 0.000000000000000000, 1.000000000000000000 ) ) ;
#64596 = CARTESIAN_POINT ( 'NONE',  ( -12.45635911906152771, -17.91357634596933934, -1.500000000000002220 ) ) ;
#64597 = CARTESIAN_POINT ( 'NONE',  ( -103.5151580449021509, -24.15620529776628445, 10.23563542870660292 ) ) ;
#64598 = VECTOR ( 'NONE', #51394, 1000.000000000000114 ) ;
#64599 = LINE ( 'NONE', #3184, #9655 ) ;
#64600 = CARTESIAN_POINT ( 'NONE',  ( 28.87399897812681004, 4.772774720514425972, -12.57761096169975445 ) ) ;
#64601 = CARTESIAN_POINT ( 'NONE',  ( 3.414333255021221092, 21.62243999391013105, -1.500000000000002220 ) ) ;
#64602 = CARTESIAN_POINT ( 'NONE',  ( 3.509873074917118085, -5.965225279485572685, 29.15869884040363758 ) ) ;
#64603 = EDGE_LOOP ( 'NONE', ( #44066, #91345, #4861, #93508 ) ) ;
#64604 = CARTESIAN_POINT ( 'NONE',  ( 25.26411791610096813, 5.170221718577081127, -8.437879337975932259 ) ) ;
#64605 = CARTESIAN_POINT ( 'NONE',  ( -85.56477010883600087, -23.48786465467240703, 11.44779295918254647 ) ) ;
#64606 = EDGE_CURVE ( 'NONE', #53312, #60724, #30427, .T. ) ;
#64607 = VERTEX_POINT ( 'NONE', #68992 ) ;
#64608 = EDGE_CURVE ( 'NONE', #75345, #51300, #7839, .T. ) ;
#64609 = CARTESIAN_POINT ( 'NONE',  ( -2.749999999999999112, 27.59999999999999432, 2.100000000000000089 ) ) ;
#64610 = AXIS2_PLACEMENT_3D ( 'NONE', #93059, #55525, #71745 ) ;
#64611 = ORIENTED_EDGE ( 'NONE', *, *, #71796, .F. ) ;
#64612 = DIRECTION ( 'NONE',  ( 0.000000000000000000, 1.000000000000000000, 0.000000000000000000 ) ) ;
#64613 = CARTESIAN_POINT ( 'NONE',  ( -82.59188034808971679, -24.15543982623907482, -0.2315651400026497997 ) ) ;
#64614 = CARTESIAN_POINT ( 'NONE',  ( 21.10678091372558640, -2.468637549841573797, 11.49999999999998934 ) ) ;
#64615 = DIRECTION ( 'NONE',  ( -3.773278334453080206E-23, 0.9999999999976377785, 2.173523156925979975E-06 ) ) ;
#64616 = CARTESIAN_POINT ( 'NONE',  ( -130.5728709571500588, -24.58764167366261333, 9.439037205594624780 ) ) ;
#64617 = EDGE_CURVE ( 'NONE', #49698, #623, #60364, .T. ) ;
#64618 = DIRECTION ( 'NONE',  ( -1.334402673828313093E-16, 0.000000000000000000, -1.000000000000000000 ) ) ;
#64619 = CARTESIAN_POINT ( 'NONE',  ( -68.52210156676301267, -23.48783264082477018, -1.443836473390095243 ) ) ;
#64620 = CARTESIAN_POINT ( 'NONE',  ( -15.52061920455031618, -11.66286593722069931, -1.500000000000002220 ) ) ;
#64621 = CARTESIAN_POINT ( 'NONE',  ( -45.63591179856666002, -24.63355581998384736, 0.9682620441944017609 ) ) ;
#64622 = VERTEX_POINT ( 'NONE', #68496 ) ;
#64623 = CARTESIAN_POINT ( 'NONE',  ( -16.58133674543539371, -10.29093563426468450, 11.49999999999999645 ) ) ;
#64624 = CARTESIAN_POINT ( 'NONE',  ( -4.968349358974361252, -6.376774720514411854, 19.46153846153847056 ) ) ;
#64625 = CARTESIAN_POINT ( 'NONE',  ( -80.48900664166535535, -25.12298712672050982, 7.101635559041870494 ) ) ;
#64626 = ORIENTED_EDGE ( 'NONE', *, *, #22287, .T. ) ;
#64627 = EDGE_CURVE ( 'NONE', #39794, #54462, #95423, .T. ) ;
#64628 = CARTESIAN_POINT ( 'NONE',  ( 4.959846025536391423, -5.876774720514417183, 20.32314756232572250 ) ) ;
#64629 = CARTESIAN_POINT ( 'NONE',  ( -89.51459311308768463, -23.96119346886881374, -0.6495511937831908167 ) ) ;
#64631 = EDGE_CURVE ( 'NONE', #31048, #451, #91325, .T. ) ;
#64630 = CARTESIAN_POINT ( 'NONE',  ( -90.52287095715006160, -25.00158670708909625, 2.256160236439166411 ) ) ;
#64632 = CARTESIAN_POINT ( 'NONE',  ( -80.51244414166535535, -25.03156060877706324, 7.563174219299074963 ) ) ;
#64633 = CARTESIAN_POINT ( 'NONE',  ( 8.085132396474181249, 17.94908993440701295, -1.500000000000002220 ) ) ;
#64634 = ADVANCED_FACE ( 'NONE', ( #22792 ), #63403, .T. ) ;
#64635 = VERTEX_POINT ( 'NONE', #32933 ) ;
#64636 = CARTESIAN_POINT ( 'NONE',  ( -78.52287095715006160, -24.51283580621366198, 0.6167428607019652675 ) ) ;
#64637 = PLANE ( 'NONE',  #35031 ) ;
#64638 = B_SPLINE_CURVE_WITH_KNOTS ( 'NONE', 3,
 ( #23229, #53712, #15129, #93251, #46092, #85646 ),
 .UNSPECIFIED., .F., .F.,
 ( 4, 2, 4 ),
 ( 6.391158118964604309E-06, 0.001387004593080781809, 0.002767618028042598960 ),
 .UNSPECIFIED. ) ;
#64639 = PERSON_AND_ORGANIZATION_ROLE ( 'design_owner' ) ;
#64640 = CARTESIAN_POINT ( 'NONE',  ( -91.92287095715003886, -23.47593901973090524, -1.443836447538997314 ) ) ;
#64641 = DIRECTION ( 'NONE',  ( 0.000000000000000000, 0.000000000000000000, 1.000000000000000000 ) ) ;
#64642 = CARTESIAN_POINT ( 'NONE',  ( -110.1363633712414298, -25.11151251321651046, 2.838859203344919813 ) ) ;
#64643 = CARTESIAN_POINT ( 'NONE',  ( -97.63537931045868845, -23.73791477778912196, 11.05961554403170410 ) ) ;
#64644 = CARTESIAN_POINT ( 'NONE',  ( -86.52287095715006160, -24.66019654487199375, 8.947790411086119278 ) ) ;
#64645 = VECTOR ( 'NONE', #11364, 1000.000000000000000 ) ;
#64646 = CARTESIAN_POINT ( 'NONE',  ( -69.34374060353803770, -25.24515230211321537, 6.178485843430418178 ) ) ;
#64647 = DIRECTION ( 'NONE',  ( -0.7071067811865474617, -0.000000000000000000, -0.7071067811865474617 ) ) ;
#64648 = CARTESIAN_POINT ( 'NONE',  ( -19.80664267627650688, 2.137978742899185214, -1.500000000000002220 ) ) ;
#64649 = CARTESIAN_POINT ( 'NONE',  ( -75.59181694504910354, -24.40133493613049964, 9.663955038902805939 ) ) ;
#64650 = CARTESIAN_POINT ( 'NONE',  ( -18.79335158860655142, 6.462138572525057967, -1.500000000000002220 ) ) ;
#64651 = VERTEX_POINT ( 'NONE', #48166 ) ;
#64652 = AXIS2_PLACEMENT_3D ( 'NONE', #38776, #84452, #14934 ) ;
#64653 = CARTESIAN_POINT ( 'NONE',  ( -71.52287095715004739, -23.72747288104470087, -1.053458166803227236 ) ) ;
#64654 = CARTESIAN_POINT ( 'NONE',  ( -50.53967329592638436, -25.13373113272038850, 7.098271152210802626 ) ) ;
#64655 = CARTESIAN_POINT ( 'NONE',  ( 32.53346577320684219, 2.682774720514426559, -11.93731717363806766 ) ) ;
#64656 = CARTESIAN_POINT ( 'NONE',  ( -80.53629517725291009, -25.00182538069146787, 7.747789668545041586 ) ) ;
#64657 = CARTESIAN_POINT ( 'NONE',  ( 20.60118427460899326, -2.865472796819775958, 11.49999999999999645 ) ) ;
#64658 = CARTESIAN_POINT ( 'NONE',  ( -6.818021687177533430, -6.376774720514408301, 19.14905311829361167 ) ) ;
#64659 = AXIS2_PLACEMENT_3D ( 'NONE', #17958, #34687, #72255 ) ;
#64660 = B_SPLINE_CURVE_WITH_KNOTS ( 'NONE', 3,
 ( #82734, #7112, #90852, #21323 ),
 .UNSPECIFIED., .F., .F.,
 ( 4, 4 ),
 ( 0.000000000000000000, 9.999999999998897304E-05 ),
 .UNSPECIFIED. ) ;
#64661 = DIRECTION ( 'NONE',  ( -0.2488812114211667037, -0.000000000000000000, -0.9685340172660599212 ) ) ;
#64662 = CARTESIAN_POINT ( 'NONE',  ( 7.682656365740156090, -21.48159684637525046, 11.49999999999999645 ) ) ;
#64663 = ORIENTED_EDGE ( 'NONE', *, *, #80542, .F. ) ;
#64664 = CARTESIAN_POINT ( 'NONE',  ( -29.49875734969025842, -5.965225279485572685, 23.37402280011862743 ) ) ;
#64665 = CARTESIAN_POINT ( 'NONE',  ( -127.5564497244640592, -23.48783264082477373, -1.443836473390084363 ) ) ;
#64666 = ORIENTED_EDGE ( 'NONE', *, *, #34911, .T. ) ;
#64667 = AXIS2_PLACEMENT_3D ( 'NONE', #5354, #36308, #98187 ) ;
#64668 = CARTESIAN_POINT ( 'NONE',  ( -20.17641613807547785, 1.360797614858565874, -1.500000000000002220 ) ) ;
#64669 = CARTESIAN_POINT ( 'NONE',  ( -55.58953762381672448, -25.00158670708909270, 2.256160236439167299 ) ) ;
#64670 = CARTESIAN_POINT ( 'NONE',  ( -114.5895376238167103, -24.66019654487199730, 8.947790411086117501 ) ) ;
#64671 = FACE_OUTER_BOUND ( 'NONE', #77488, .T. ) ;
#64672 = ORIENTED_EDGE ( 'NONE', *, *, #68576, .F. ) ;
#64673 = DIRECTION ( 'NONE',  ( 0.000000000000000000, 0.000000000000000000, -1.000000000000000000 ) ) ;
#64674 = CARTESIAN_POINT ( 'NONE',  ( -100.6228709571500559, -24.91544648472626378, 1.928969306349431534 ) ) ;
#64675 = CARTESIAN_POINT ( 'NONE',  ( 7.431233518514567926, -18.57414813805618081, -1.500000000000002220 ) ) ;
#64676 = CARTESIAN_POINT ( 'NONE',  ( -12.80012119340476140, -16.60591428456014640, 11.49999999999999645 ) ) ;
#64677 = LINE ( 'NONE', #86974, #77708 ) ;
#64678 = CARTESIAN_POINT ( 'NONE',  ( -124.6228709571500701, -24.50321055353806443, 9.387540953477524042 ) ) ;
#64679 = CARTESIAN_POINT ( 'NONE',  ( 21.95769793831392036, 2.030053023538682222, -1.500000000000002220 ) ) ;
#64680 = CARTESIAN_POINT ( 'NONE',  ( -40.11299260137283795, -25.31589322304537504, 5.047402315637626202 ) ) ;
#64681 = OPEN_SHELL ( 'NONE', ( #34457 ) ) ;
#64682 = VERTEX_POINT ( 'NONE', #78582 ) ;
#64683 = LINE ( 'NONE', #47932, #64645 ) ;
#64684 = FACE_OUTER_BOUND ( 'NONE', #67003, .T. ) ;
#64685 = CARTESIAN_POINT ( 'NONE',  ( -50.52287095715006160, -24.99132157543166599, 2.256160258750667502 ) ) ;
#64686 = ORIENTED_EDGE ( 'NONE', *, *, #11656, .F. ) ;
#64687 = PLANE ( 'NONE',  #43763 ) ;
#64688 = EDGE_CURVE ( 'NONE', #81281, #96245, #3383, .T. ) ;
#64689 = ORIENTED_EDGE ( 'NONE', *, *, #13716, .F. ) ;
#64690 = ADVANCED_FACE ( 'NONE', ( #9091 ), #17705, .T. ) ;
#64691 = ORIENTED_EDGE ( 'NONE', *, *, #72028, .T. ) ;
#64692 = CARTESIAN_POINT ( 'NONE',  ( 6.573941812937369455, -7.905506363763796338E-18, 0.2639660507643297183 ) ) ;
#64693 = DIRECTION ( 'NONE',  ( 4.448048651795327725E-16, 1.000000000000000000, 7.118365844322534241E-16 ) ) ;
#64694 = DIRECTION ( 'NONE',  ( 0.000000000000000000, 0.9999999999976377785, 2.173523156925979975E-06 ) ) ;
#64695 = CARTESIAN_POINT ( 'NONE',  ( 2.947869850540926429, 20.32360706268488215, -1.500000000000002220 ) ) ;
#64696 = EDGE_CURVE ( 'NONE', #12570, #76880, #86217, .T. ) ;
#64697 = EDGE_LOOP ( 'NONE', ( #403, #37795, #75226, #43949 ) ) ;
#64698 = CARTESIAN_POINT ( 'NONE',  ( 8.071512145086529699, -9.528487854913505473, 6.500000000000001776 ) ) ;
#64699 = CARTESIAN_POINT ( 'NONE',  ( -8.160000000000000142, 8.793627758918228565, -2.994553991265763049 ) ) ;
#64700 = LINE ( 'NONE', #80891, #82100 ) ;
#64701 = CARTESIAN_POINT ( 'NONE',  ( 15.82088602905085750, -15.72875506571707760, -1.500000000000002220 ) ) ;
#64702 = ADVANCED_FACE ( 'NONE', ( #15701 ), #94320, .F. ) ;
#64703 = ADVANCED_FACE ( 'NONE', ( #25313 ), #10091, .T. ) ;
#64704 = CARTESIAN_POINT ( 'NONE',  ( 32.70426658926474062, -3.547616055647111022, -3.273583889775387057 ) ) ;
#64705 = FACE_OUTER_BOUND ( 'NONE', #76523, .T. ) ;
#64706 = ORIENTED_EDGE ( 'NONE', *, *, #66649, .F. ) ;
#64707 = PLANE ( 'NONE',  #59854 ) ;
#64708 = CARTESIAN_POINT ( 'NONE',  ( -73.52287095715013265, -23.96127896941631974, -0.6493128931038029128 ) ) ;
#64709 = CARTESIAN_POINT ( 'NONE',  ( 11.47802407633690258, -17.41396394059345454, -1.500000000000002220 ) ) ;
#64710 = EDGE_LOOP ( 'NONE', ( #24464, #33724, #88046, #14100 ) ) ;
#64712 = ORIENTED_EDGE ( 'NONE', *, *, #56569, .F. ) ;
#64711 = CARTESIAN_POINT ( 'NONE',  ( -0.2200237740140755516, -6.376774720514408301, 19.17724329193115551 ) ) ;
#64714 = ORIENTED_EDGE ( 'NONE', *, *, #3842, .F. ) ;
#64713 = ADVANCED_BREP_SHAPE_REPRESENTATION ( '', ( #44893, #37391 ), #61811 ) ;
#64715 = CARTESIAN_POINT ( 'NONE',  ( -69.97463645619113493, -25.03149363652662274, 7.520861778187123647 ) ) ;
#64716 = CARTESIAN_POINT ( 'NONE',  ( 12.99892964944760543, 16.54660993828877125, -1.500000000000002220 ) ) ;
#64717 = ORIENTED_EDGE ( 'NONE', *, *, #6081, .T. ) ;
#64718 = CARTESIAN_POINT ( 'NONE',  ( -102.5228709571500758, -24.65952944569305316, 1.056160979905702346 ) ) ;
#64719 = DIRECTION ( 'NONE',  ( -1.000000000000000000, -0.000000000000000000, 0.000000000000000000 ) ) ;
#64720 = CARTESIAN_POINT ( 'NONE',  ( -108.6228709571500559, -29.50250243563736774, 8.947779886222136270 ) ) ;
#64721 = AXIS2_PLACEMENT_3D ( 'NONE', #45620, #51733, #91772 ) ;
#64722 = CARTESIAN_POINT ( 'NONE',  ( -86.54506020849899528, -24.51419770103155926, 9.386484678747184063 ) ) ;
#64723 = CARTESIAN_POINT ( 'NONE',  ( -59.51516556476029507, -23.73766607897669445, -1.055555164236460675 ) ) ;
#64724 = CARTESIAN_POINT ( 'NONE',  ( 0.4029737066630413311, -21.70969715354747009, -1.500000000000002220 ) ) ;
#64725 = DIRECTION ( 'NONE',  ( 0.000000000000000000, -1.000000000000000000, 0.000000000000000000 ) ) ;
#64727 = ORIENTED_EDGE ( 'NONE', *, *, #52994, .T. ) ;
#64726 = CARTESIAN_POINT ( 'NONE',  ( -19.85906585229243504, 9.992431322412627992, 11.49999999999999645 ) ) ;
#64728 = CARTESIAN_POINT ( 'NONE',  ( -119.4728709571500644, -25.40558663563398056, 5.000950440326719537 ) ) ;
#64729 = CARTESIAN_POINT ( 'NONE',  ( -100.6814946224345846, -25.30401792888237367, 5.197789011716578145 ) ) ;
#64730 = EDGE_CURVE ( 'NONE', #61820, #93974, #63911, .T. ) ;
#64731 = CARTESIAN_POINT ( 'NONE',  ( -70.65813959336661298, -25.30064099092117758, 5.349778433208494555 ) ) ;
#64732 = ORIENTED_EDGE ( 'NONE', *, *, #12986, .T. ) ;
#64733 = AXIS2_PLACEMENT_3D ( 'NONE', #33725, #58079, #10887 ) ;
#64735 = ORIENTED_EDGE ( 'NONE', *, *, #79430, .T. ) ;
#64734 = CARTESIAN_POINT ( 'NONE',  ( -5.895658455092926076, -6.376774720514418959, 20.50445910983877340 ) ) ;
#64736 = ADVANCED_FACE ( 'NONE', ( #40043 ), #1493, .T. ) ;
#64737 = AXIS2_PLACEMENT_3D ( 'NONE', #37563, #51798, #84225 ) ;
#64738 = ORIENTED_EDGE ( 'NONE', *, *, #72996, .T. ) ;
#64739 = VECTOR ( 'NONE', #93840, 1000.000000000000000 ) ;
#64740 = CARTESIAN_POINT ( 'NONE',  ( -47.58953762381671737, -24.64965694238406613, 8.947790433994660120 ) ) ;
#64741 = DIRECTION ( 'NONE',  ( -3.491481338843133355E-15, 1.000000000000000000, -2.352173255807804438E-16 ) ) ;
#64742 = CARTESIAN_POINT ( 'NONE',  ( -32.62287095715005592, -23.96127896941632685, -0.6493128931037921436 ) ) ;
#64743 = ORIENTED_EDGE ( 'NONE', *, *, #68768, .T. ) ;
#64744 = CARTESIAN_POINT ( 'NONE',  ( -130.5728709571501156, -24.71478263084194538, 9.068606591826432251 ) ) ;
#64745 = CARTESIAN_POINT ( 'NONE',  ( -21.90463088927077706, -4.570550247397807908, -1.500000000000002220 ) ) ;
#64746 = ORIENTED_EDGE ( 'NONE', *, *, #65277, .F. ) ;
#64747 = ORIENTED_EDGE ( 'NONE', *, *, #24696, .T. ) ;
#64748 = CARTESIAN_POINT ( 'NONE',  ( -34.52287095715006160, -23.95044443724991723, 10.65354141964649237 ) ) ;
#64749 = CARTESIAN_POINT ( 'NONE',  ( -101.5853466808658254, -24.66019654487200086, 8.947790411086115725 ) ) ;
#64750 = CARTESIAN_POINT ( 'NONE',  ( -39.56956369306367094, -25.31127738444162034, 4.659494810401162646 ) ) ;
#64751 = CARTESIAN_POINT ( 'NONE',  ( -99.52287095715006160, -29.50248528299804818, 1.056150453629042030 ) ) ;
#64753 = EDGE_CURVE ( 'NONE', #9998, #82876, #94110, .T. ) ;
#64752 = CARTESIAN_POINT ( 'NONE',  ( -30.59463558439210118, -24.75179208683297105, 8.640809912072082710 ) ) ;
#64754 = CARTESIAN_POINT ( 'NONE',  ( -19.52990877098713796, 1.257015143768854815, -1.500000000000002220 ) ) ;
#64755 = FACE_OUTER_BOUND ( 'NONE', #72253, .T. ) ;
#64756 = ORIENTED_EDGE ( 'NONE', *, *, #88902, .T. ) ;
#64757 = CARTESIAN_POINT ( 'NONE',  ( -15.45034113870702441, -14.97902827799142500, 11.49999999999998934 ) ) ;
#64758 = CARTESIAN_POINT ( 'NONE',  ( -51.29687923781919068, -25.27367468601215350, 3.993462154588707680 ) ) ;
#64759 = CARTESIAN_POINT ( 'NONE',  ( -71.19450251067907232, -25.25639499143044731, 6.630762337283159447 ) ) ;
#64760 = CARTESIAN_POINT ( 'NONE',  ( 27.86270917940689174, 5.965225279485572685, 29.49402280011862487 ) ) ;
#64761 = ADVANCED_FACE ( 'NONE', ( #69989 ), #31934, .F. ) ;
#64762 = CARTESIAN_POINT ( 'NONE',  ( -20.27875734969026311, -4.543225279485573864, 24.00402280011862288 ) ) ;
#64763 = CARTESIAN_POINT ( 'NONE',  ( 15.56936346670522120, 16.85858822313069894, -1.500000000000002220 ) ) ;
#64764 = AXIS2_PLACEMENT_3D ( 'NONE', #52884, #21903, #83317 ) ;
#64765 = CALENDAR_DATE ( 2026, 9, 10 ) ;
#64766 = PLANE ( 'NONE',  #33691 ) ;
#64767 = CARTESIAN_POINT ( 'NONE',  ( -129.6228709571500417, -29.50250243563736774, 8.947779886222132717 ) ) ;
#64768 = CARTESIAN_POINT ( 'NONE',  ( -18.81522532469529452, 6.996975221643539911, 11.49999999999999645 ) ) ;
#64769 = CARTESIAN_POINT ( 'NONE',  ( 9.402885806365684829, 0.3587747205144265483, 29.04108526060719342 ) ) ;
#64770 = DIRECTION ( 'NONE',  ( 0.03244919754393515293, 0.000000000000000000, -0.9994733861282923959 ) ) ;
#64771 = CARTESIAN_POINT ( 'NONE',  ( -99.52287095715011844, -23.48783264083466449, -1.443836473374706442 ) ) ;
#64772 = CARTESIAN_POINT ( 'NONE',  ( -36.62287095715005592, -24.64965695001467694, 8.947790433994187609 ) ) ;
#64773 = DIRECTION ( 'NONE',  ( 0.000000000000000000, 0.000000000000000000, -1.000000000000000000 ) ) ;
#64774 = CARTESIAN_POINT ( 'NONE',  ( 15.56394622224390645, 12.30447529683395125, -1.500000000000002220 ) ) ;
#64775 = CARTESIAN_POINT ( 'NONE',  ( 2.021814659504407579E-13, -19.30000000000000426, 11.49999999999999645 ) ) ;
#64776 = CARTESIAN_POINT ( 'NONE',  ( 18.28535361393070957, 7.309334553982634652, -1.500000000000002220 ) ) ;
#64777 = LINE ( 'NONE', #10958, #24845 ) ;
#64778 = CARTESIAN_POINT ( 'NONE',  ( -41.62287095715007723, -23.73934037231756733, 11.05740245334329863 ) ) ;
#64779 = PERSON_AND_ORGANIZATION_ROLE ( 'classification_officer' ) ;
#64780 = CARTESIAN_POINT ( 'NONE',  ( -125.6228709571500559, -23.47596703998600631, 11.44779298504227860 ) ) ;
#64781 = CARTESIAN_POINT ( 'NONE',  ( 11.56983764158150052, 5.965225279485572685, 28.29037853177889517 ) ) ;
#64782 = CARTESIAN_POINT ( 'NONE',  ( 18.09409571311175569, -9.955296453752364272, 11.49999999999999645 ) ) ;
#64783 = LINE ( 'NONE', #39906, #26306 ) ;
#64784 = CIRCLE ( 'NONE', #19397, 1.700000000000000178 ) ;
#64785 = CARTESIAN_POINT ( 'NONE',  ( 13.91401389203221406, 5.965225279485572685, 158.0376437107427137 ) ) ;
#64786 = CARTESIAN_POINT ( 'NONE',  ( -20.50338545487000275, 9.463669735852004550, 11.49999999999999645 ) ) ;
#64787 = ORIENTED_EDGE ( 'NONE', *, *, #23637, .F. ) ;
#64788 = CARTESIAN_POINT ( 'NONE',  ( -53.62287095715004881, -24.65952944569303895, 1.056160979905692576 ) ) ;
#64789 = CARTESIAN_POINT ( 'NONE',  ( -97.59657083758668250, -23.73766607897670156, -1.055555164236452237 ) ) ;
#64790 = CARTESIAN_POINT ( 'NONE',  ( -26.26041136509451590, -24.89299099432205864, 3.510312236646374373 ) ) ;
#64791 = AXIS2_PLACEMENT_3D ( 'NONE', #58183, #81516, #51066 ) ;
#64792 = CARTESIAN_POINT ( 'NONE',  ( -26.98635835925963633, -24.61460083625618722, 8.112879358581045253 ) ) ;
#64793 = DIRECTION ( 'NONE',  ( 0.000000000000000000, 0.000000000000000000, -1.000000000000000000 ) ) ;
#64794 = CIRCLE ( 'NONE', #11308, 3.500000000000000000 ) ;
#64795 = ORIENTED_EDGE ( 'NONE', *, *, #64688, .F. ) ;
#64796 = CARTESIAN_POINT ( 'NONE',  ( 11.81885653190370888, -19.86314957129924608, 11.49999999999999645 ) ) ;
#64797 = CARTESIAN_POINT ( 'NONE',  ( 12.51456667378993259, 19.11410217522374921, -1.500000000000002220 ) ) ;
#64798 = DIRECTION ( 'NONE',  ( 0.000000000000000000, 1.000000000000000000, 1.478457507934778393E-16 ) ) ;
#64799 = AXIS2_PLACEMENT_3D ( 'NONE', #40320, #79870, #87998 ) ;
#64800 = CARTESIAN_POINT ( 'NONE',  ( 0.3910256410256418569, -5.876774720514419847, 20.67377804487180271 ) ) ;
#64801 = CARTESIAN_POINT ( 'NONE',  ( -82.50294125089578756, -24.51419770103156281, 9.386484678747185839 ) ) ;
#64802 = CARTESIAN_POINT ( 'NONE',  ( 12.90280524143238594, -18.44629484376132922, 11.49999999999999645 ) ) ;
#64803 = ORIENTED_EDGE ( 'NONE', *, *, #40260, .F. ) ;
#64804 = AXIS2_PLACEMENT_3D ( 'NONE', #74741, #19957, #36196 ) ;
#64805 = CARTESIAN_POINT ( 'NONE',  ( -25.92875734969025814, 3.316774720514426456, 0.7300228001186309656 ) ) ;
#64806 = CARTESIAN_POINT ( 'NONE',  ( 12.42595048307055983, -18.10569578304522764, -1.500000000000002220 ) ) ;
#64807 = CARTESIAN_POINT ( 'NONE',  ( -120.5228709571500616, -25.00158670708909625, 2.256160236439166411 ) ) ;
#64809 = CARTESIAN_POINT ( 'NONE',  ( -111.6286677502680789, -23.96119346886881019, -0.6495511937832035843 ) ) ;
#64808 = AXIS2_PLACEMENT_3D ( 'NONE', #93497, #87398, #47343 ) ;
#64810 = CARTESIAN_POINT ( 'NONE',  ( -29.24615158708846963, -24.79699756444347969, 5.024435584847914527 ) ) ;
#64811 = VERTEX_POINT ( 'NONE', #54284 ) ;
#64812 = CARTESIAN_POINT ( 'NONE',  ( -48.49448130989669892, -24.35071581493543036, 9.817618358456027039 ) ) ;
#64813 = CARTESIAN_POINT ( 'NONE',  ( -0.08860454909227881426, -5.876774720514410077, 19.21747685089457036 ) ) ;
#64814 = VERTEX_POINT ( 'NONE', #78085 ) ;
#64815 = CARTESIAN_POINT ( 'NONE',  ( -54.65091972564611922, -23.73791477778911130, 11.05961554403171299 ) ) ;
#64816 = ADVANCED_FACE ( 'NONE', ( #23808, #79092 ), #39040, .F. ) ;
#64817 = CARTESIAN_POINT ( 'NONE',  ( 17.04084431845542369, 11.38269047019995206, 11.49999999999998934 ) ) ;
#64818 =( BOUNDED_SURFACE ( )  B_SPLINE_SURFACE ( 3, 2, ( 
 ( #22356, #5655, #98491 ),
 ( #15761, #6153, #67574 ),
 ( #28993, #37106, #45723 ),
 ( #98992, #22855, #29483 ) ),
 .UNSPECIFIED., .F., .F., .T. ) 
 B_SPLINE_SURFACE_WITH_KNOTS ( ( 4, 4 ),
 ( 3, 3 ),
 ( 0.004439845973569162343, 0.004703938444645663561 ),
 ( 0.000000000000000000, 1.000000000000000000 ),
 .UNSPECIFIED. ) 
 GEOMETRIC_REPRESENTATION_ITEM ( )  RATIONAL_B_SPLINE_SURFACE ( (
 ( 1.000000000000000000, 0.9005394799515968884, 1.000000000000000000),
 ( 1.000000000000000000, 0.9005352985759397244, 1.000000000000000000),
 ( 1.000000000000000000, 0.8990570573199264670, 1.000000000000000000),
 ( 1.000000000000000000, 0.8962098481621324497, 1.000000000000000000) ) ) 
 REPRESENTATION_ITEM ( '' )  SURFACE ( )  );
#64819 = ORIENTED_EDGE ( 'NONE', *, *, #95586, .T. ) ;
#64820 = ORIENTED_EDGE ( 'NONE', *, *, #11204, .T. ) ;
#64821 = VERTEX_POINT ( 'NONE', #71505 ) ;
#64822 = CARTESIAN_POINT ( 'NONE',  ( -50.31102424471665557, -25.31399524998115780, 5.199282048349309626 ) ) ;
#64823 = CARTESIAN_POINT ( 'NONE',  ( 23.08992502549420323, -0.8469403905869224980, -1.500000000000002220 ) ) ;
#64824 = CARTESIAN_POINT ( 'NONE',  ( -104.6286252005051693, -24.15620529776628800, 10.23563542870659759 ) ) ;
#64825 = CARTESIAN_POINT ( 'NONE',  ( -5.305567426876419468, 19.62801697144059787, -1.500000000000002220 ) ) ;
#64826 = ADVANCED_FACE ( 'NONE', ( #23299 ), #36925, .T. ) ;
#64827 = ORIENTED_EDGE ( 'NONE', *, *, #9249, .F. ) ;
#64828 = CARTESIAN_POINT ( 'NONE',  ( -46.62287095715004881, -29.50247984919015209, -1.443849546365058689 ) ) ;
#64829 = CARTESIAN_POINT ( 'NONE',  ( -88.62287095715004170, -23.48783264082479150, -1.443836473390063935 ) ) ;
#64830 = EDGE_CURVE ( 'NONE', #54879, #95555, #37350, .T. ) ;
#64831 = CARTESIAN_POINT ( 'NONE',  ( -46.58953762381672448, -24.65952944569303895, 1.056160979905690134 ) ) ;
#64832 = CARTESIAN_POINT ( 'NONE',  ( -29.49875734969025842, 0.3587747205144265483, 17.86602280011862476 ) ) ;
#64833 = ORIENTED_EDGE ( 'NONE', *, *, #43960, .T. ) ;
#64834 = CARTESIAN_POINT ( 'NONE',  ( -28.45618646431091392, -24.76880908853930308, 2.526465311820395243 ) ) ;
#64835 = CARTESIAN_POINT ( 'NONE',  ( -49.19182681462018536, -25.31573717972797866, 4.415198315518342298 ) ) ;
#64836 = EDGE_CURVE ( 'NONE', #89496, #95755, #47047, .T. ) ;
#64837 = ORIENTED_EDGE ( 'NONE', *, *, #37682, .F. ) ;
#64838 = EDGE_CURVE ( 'NONE', #75985, #6656, #42212, .T. ) ;
#64839 = CARTESIAN_POINT ( 'NONE',  ( 1.212613378922696050, -20.72488358683818888, 11.49999999999998934 ) ) ;
#64840 = VERTEX_POINT ( 'NONE', #65411 ) ;
#64842 = VERTEX_POINT ( 'NONE', #58765 ) ;
#64841 = CARTESIAN_POINT ( 'NONE',  ( -125.5547332246454175, -24.63355581998386512, 0.9682620441944075340 ) ) ;
#64843 = CARTESIAN_POINT ( 'NONE',  ( -41.60819791265744527, -23.73791477778911485, 11.05961554403170943 ) ) ;
#64844 = LINE ( 'NONE', #95754, #59995 ) ;
#64845 = ORIENTED_EDGE ( 'NONE', *, *, #20572, .F. ) ;
#64846 = ORIENTED_EDGE ( 'NONE', *, *, #34733, .T. ) ;
#64847 = CARTESIAN_POINT ( 'NONE',  ( -6.020540257910568904, -5.876774720514411854, 19.49847411603315095 ) ) ;
#64848 = CARTESIAN_POINT ( 'NONE',  ( -116.6228709571501270, -23.96177878511308634, 10.65340807706329684 ) ) ;
#64849 = LINE ( 'NONE', #63334, #4390 ) ;
#64851 = ORIENTED_EDGE ( 'NONE', *, *, #16805, .T. ) ;
#64850 = CARTESIAN_POINT ( 'NONE',  ( -16.08457400211760913, 15.13120210334024662, 11.49999999999999645 ) ) ;
#64852 = CARTESIAN_POINT ( 'NONE',  ( 2.499999999999993783, 4.999999999999997335, 2.100000000000000089 ) ) ;
#64853 = CARTESIAN_POINT ( 'NONE',  ( -22.56969522194696509, -0.6267768857631424995, -1.500000000000002220 ) ) ;
#64854 = EDGE_CURVE ( 'NONE', #39047, #64365, #28925, .T. ) ;
#64856 = VERTEX_POINT ( 'NONE', #12581 ) ;
#64855 = CARTESIAN_POINT ( 'NONE',  ( -95.62287095715005592, -23.48783264082479150, -1.443836473390061936 ) ) ;
#64857 = EDGE_LOOP ( 'NONE', ( #43091, #51381, #40192, #32745 ) ) ;
#64858 = CARTESIAN_POINT ( 'NONE',  ( 8.160000000000000142, -2.191226316053958875E-18, 2.701633758479787833E-17 ) ) ;
#64859 = AXIS2_PLACEMENT_3D ( 'NONE', #32199, #49956, #55559 ) ;
#64860 = CARTESIAN_POINT ( 'NONE',  ( -57.62780115005737258, -24.51419770103157347, 9.386484678747176957 ) ) ;
#64861 = VERTEX_POINT ( 'NONE', #43049 ) ;
#64862 = CARTESIAN_POINT ( 'NONE',  ( -17.86006801910157193, 11.38285951858322242, -1.500000000000002220 ) ) ;
#64863 = CARTESIAN_POINT ( 'NONE',  ( 29.70220533433690946, -3.316774720514426456, 28.20564067601640801 ) ) ;
#64864 = AXIS2_PLACEMENT_3D ( 'NONE', #51314, #20843, #65069 ) ;
#64865 = CARTESIAN_POINT ( 'NONE',  ( -7.326923076923076650, -5.876774720514417183, 20.36318108974359831 ) ) ;
#64866 = CARTESIAN_POINT ( 'NONE',  ( 11.16000000000000014, -9.652339641703484574, -1.621096496867199033 ) ) ;
#64867 = CARTESIAN_POINT ( 'NONE',  ( -19.97062832128981213, -9.750827054148329509, -1.500000000000002220 ) ) ;
#64868 = CARTESIAN_POINT ( 'NONE',  ( 32.45853543194704116, 5.965225279485572685, 9.169203677920338080 ) ) ;
#64869 = ORIENTED_EDGE ( 'NONE', *, *, #11189, .T. ) ;
#64870 = CYLINDRICAL_SURFACE ( 'NONE', #74044, 2.040000000000000036 ) ;
#64871 = DIRECTION ( 'NONE',  ( -1.250865172912931245E-15, 6.879758451021121945E-15, -1.000000000000000000 ) ) ;
#64872 = VECTOR ( 'NONE', #17275, 1000.000000000000114 ) ;
#64873 = CARTESIAN_POINT ( 'NONE',  ( -10.34999999999999254, 12.00000000000002309, 2.100000000000000089 ) ) ;
#64874 = LINE ( 'NONE', #26277, #1597 ) ;
#64875 = CIRCLE ( 'NONE', #3297, 2.040000000000001368 ) ;
#64876 = CARTESIAN_POINT ( 'NONE',  ( -19.06185424839875964, 3.971334347869299286, 11.49999999999998934 ) ) ;
#64877 = AXIS2_PLACEMENT_3D ( 'NONE', #59036, #20947, #82847 ) ;
#64878 = CARTESIAN_POINT ( 'NONE',  ( 2.169945595249806125, 21.32849103866527329, 11.49999999999998934 ) ) ;
#64879 = CARTESIAN_POINT ( 'NONE',  ( 9.450000000000002842, -2.000000000000001332, 18.24068255301868291 ) ) ;
#64880 = CARTESIAN_POINT ( 'NONE',  ( -27.55569643375672584, -24.57999497573050007, 1.631374204058557043 ) ) ;
#64881 = PLANE ( 'NONE',  #90841 ) ;
#64882 = FACE_OUTER_BOUND ( 'NONE', #96369, .T. ) ;
#64883 = CARTESIAN_POINT ( 'NONE',  ( -16.51154719052397724, 15.62863258182435189, -1.500000000000002220 ) ) ;
#64884 = EDGE_CURVE ( 'NONE', #18359, #20944, #95329, .T. ) ;
#64885 = CARTESIAN_POINT ( 'NONE',  ( -98.58489604146052443, -24.65952944569305316, 1.056160979905700570 ) ) ;
#64886 = CARTESIAN_POINT ( 'NONE',  ( -103.5228709571500758, -23.47596703998600631, 11.44779298504228215 ) ) ;
#64887 = CARTESIAN_POINT ( 'NONE',  ( 18.06118663784855372, 8.336529998961283994, 11.49999999999999645 ) ) ;
#64888 = DIRECTION ( 'NONE',  ( -3.773278334453080206E-23, 0.9999999999976377785, 2.173523156925979975E-06 ) ) ;
#64889 = DIRECTION ( 'NONE',  ( 0.000000000000000000, -1.000000000000000000, 1.478457507934778393E-16 ) ) ;
#64890 = CARTESIAN_POINT ( 'NONE',  ( -48.58720723522154827, -24.34968618360933590, 0.1864209137778884418 ) ) ;
#64891 = ORIENTED_EDGE ( 'NONE', *, *, #98087, .T. ) ;
#64892 = DIRECTION ( 'NONE',  ( -1.000000000000000000, -3.773278334444167608E-23, -8.201307833595939069E-29 ) ) ;
#64893 = EDGE_CURVE ( 'NONE', #31485, #46589, #19684, .T. ) ;
#64894 = CARTESIAN_POINT ( 'NONE',  ( -31.82673689144044360, -24.87479601683088148, 8.247789944647561100 ) ) ;
#64895 = CARTESIAN_POINT ( 'NONE',  ( -14.16021466491576675, 16.42052772630311352, 11.49999999999998934 ) ) ;
#64896 = CARTESIAN_POINT ( 'NONE',  ( -51.60933002250928325, -25.14098292474398377, 7.057872611485954906 ) ) ;
#64897 = CARTESIAN_POINT ( 'NONE',  ( -4.154358412494840280, 19.03220294597612039, -1.500000000000002220 ) ) ;
#64898 = CARTESIAN_POINT ( 'NONE',  ( 14.76093561896379214, 3.316774720514426456, -26.55548769130089681 ) ) ;
#64899 = ORIENTED_EDGE ( 'NONE', *, *, #89891, .T. ) ;
#64900 = B_SPLINE_CURVE_WITH_KNOTS ( 'NONE', 3,
 ( #5511, #22223, #66936, #53204 ),
 .UNSPECIFIED., .F., .F.,
 ( 4, 4 ),
 ( 3.469446951953614189E-18, 0.0001002978978728838905 ),
 .UNSPECIFIED. ) ;
#64901 = PERSON_AND_ORGANIZATION ( #63439, #3637 ) ;
#64902 = CARTESIAN_POINT ( 'NONE',  ( -4.045674540461745572, 11.20951781186025897, 0.000000000000000000 ) ) ;
#64903 = CARTESIAN_POINT ( 'NONE',  ( 18.81987132735423174, -8.002443037797982939, 11.49999999999999645 ) ) ;
#64904 = LINE ( 'NONE', #33924, #63481 ) ;
#64905 = APPROVAL ( #60265, 'UNKNOWN' ) ;
#64906 = LINE ( 'NONE', #27805, #62630 ) ;
#64907 = ORIENTED_EDGE ( 'NONE', *, *, #9452, .F. ) ;
#64908 = DIRECTION ( 'NONE',  ( 0.9822594791677485837, 0.000000000000000000, -0.1875268396392986980 ) ) ;
#64909 = CARTESIAN_POINT ( 'NONE',  ( 0.8635838190919263857, -3.990505948720460605, -8.999999999999998224 ) ) ;
#64910 = CARTESIAN_POINT ( 'NONE',  ( -39.18717306657202215, -25.31628593408776595, 4.881706631208792224 ) ) ;
#64911 = CARTESIAN_POINT ( 'NONE',  ( 30.43908124610670285, -2.682774720514426559, -13.86910542224428866 ) ) ;
#64912 = CARTESIAN_POINT ( 'NONE',  ( -109.6247177088518896, -24.51314013834315730, 0.6176544820404190617 ) ) ;
#64913 = ORIENTED_EDGE ( 'NONE', *, *, #63727, .T. ) ;
#64914 = CARTESIAN_POINT ( 'NONE',  ( -66.49287662190819503, -24.66019654487199375, 8.947790411086119278 ) ) ;
#64915 = CARTESIAN_POINT ( 'NONE',  ( -22.60589916338503613, 3.847557683979087706, 11.49999999999999645 ) ) ;
#64916 = CARTESIAN_POINT ( 'NONE',  ( -2.780358639097238349, 22.57001311929844434, -1.500000000000002220 ) ) ;
#64917 = CARTESIAN_POINT ( 'NONE',  ( 4.689770114687411784, -6.376774720514424288, 21.33175327469028915 ) ) ;
#64918 = CARTESIAN_POINT ( 'NONE',  ( -122.6228709571500417, -23.47593901973091235, -1.443836447538997536 ) ) ;
#64919 = CARTESIAN_POINT ( 'NONE',  ( -90.58763920575688644, -24.63355581998384380, 0.9682620441943978751 ) ) ;
#64920 = CARTESIAN_POINT ( 'NONE',  ( -125.2228709571500644, -23.47593901973090524, -1.443836447538996426 ) ) ;
#64921 = CARTESIAN_POINT ( 'NONE',  ( -44.55620429048338593, -23.48783264082477373, -1.443836473390073261 ) ) ;
#64922 = VECTOR ( 'NONE', #6379, 1000.000000000000114 ) ;
#64923 = CARTESIAN_POINT ( 'NONE',  ( -21.72861685410901700, 2.547970858986955189, 11.49999999999998934 ) ) ;
#64924 = B_SPLINE_CURVE_WITH_KNOTS ( 'NONE', 3,
 ( #90023, #97134, #20993, #98115, #80411, #89030, #73308, #58579, #81910, #74782, #81415, #12388, #89522, #12880 ),
 .UNSPECIFIED., .F., .F.,
 ( 4, 2, 2, 2, 2, 2, 4 ),
 ( 7.059813062317230268E-18, 0.0002389841638349673222, 0.0004779683276699275970, 0.0009559366553398477130, 0.001433904983009767937, 0.001672889146844726803, 0.001911873310679685885 ),
 .UNSPECIFIED. ) ;
#64925 = CARTESIAN_POINT ( 'NONE',  ( -69.58396311289207858, -24.51419770103157347, 9.386484678747178734 ) ) ;
#64926 = CARTESIAN_POINT ( 'NONE',  ( -49.04145601308662350, -25.30525654051268702, 5.514141841267435673 ) ) ;
#64927 = CARTESIAN_POINT ( 'NONE',  ( 22.81105451610979173, -1.477225279485574028, -18.46691820600746681 ) ) ;
#64928 = FACE_OUTER_BOUND ( 'NONE', #43065, .T. ) ;
#64929 = ORIENTED_EDGE ( 'NONE', *, *, #22296, .T. ) ;
#64930 = CARTESIAN_POINT ( 'NONE',  ( -8.052747710315523832, 18.77774781879659116, -1.500000000000002220 ) ) ;
#64931 = ORIENTED_EDGE ( 'NONE', *, *, #75926, .T. ) ;
#64932 = EDGE_LOOP ( 'NONE', ( #96371, #66574, #3270, #81161 ) ) ;
#64933 = CARTESIAN_POINT ( 'NONE',  ( 14.87233727408824713, -17.56007624320114857, -1.500000000000002220 ) ) ;
#64934 = CARTESIAN_POINT ( 'NONE',  ( 21.57151214508649772, 0.000000000000000000, 0.000000000000000000 ) ) ;
#64935 = ORIENTED_EDGE ( 'NONE', *, *, #10014, .F. ) ;
#64936 = DIRECTION ( 'NONE',  ( 0.000000000000000000, -1.000000000000000000, 0.000000000000000000 ) ) ;
#64937 = CARTESIAN_POINT ( 'NONE',  ( -4.929522925832174884, -0.3587747205143967943, -28.63504101147569614 ) ) ;
#64939 = CARTESIAN_POINT ( 'NONE',  ( -2.499999999999993339, 19.99999999999999645, 2.100000000000000089 ) ) ;
#64938 = AXIS2_PLACEMENT_3D ( 'NONE', #92032, #95537, #26024 ) ;
#64940 = CARTESIAN_POINT ( 'NONE',  ( -53.62803857038250044, -24.51419770103157347, 9.386484678747180510 ) ) ;
#64942 = ORIENTED_EDGE ( 'NONE', *, *, #66991, .F. ) ;
#64941 = CARTESIAN_POINT ( 'NONE',  ( -18.12654925440673637, -11.31956730046968751, 11.49999999999999645 ) ) ;
#64943 = ADVANCED_FACE ( 'NONE', ( #10586 ), #81604, .T. ) ;
#64944 = VECTOR ( 'NONE', #20342, 1000.000000000000000 ) ;
#64945 = VERTEX_POINT ( 'NONE', #72502 ) ;
#64946 = CARTESIAN_POINT ( 'NONE',  ( -18.24902840909259538, -12.68162010772806170, -1.500000000000002220 ) ) ;
#64947 = EDGE_CURVE ( 'NONE', #61568, #88227, #26320, .T. ) ;
#64948 = CARTESIAN_POINT ( 'NONE',  ( 15.58315679939408582, 13.61395703526229894, 11.49999999999998934 ) ) ;
#64949 = B_SPLINE_CURVE_WITH_KNOTS ( 'NONE', 3,
 ( #71162, #73166, #86872, #1652, #33594, #79256, #32588, #3163, #88384, #71663 ),
 .UNSPECIFIED., .F., .F.,
 ( 4, 2, 2, 2, 4 ),
 ( 5.204170427930421283E-18, 0.0002155461666041007132, 0.0004310923332081962223, 0.0006466384998122917584, 0.0008621846664163872404 ),
 .UNSPECIFIED. ) ;
#64950 = VECTOR ( 'NONE', #87686, 1000.000000000000000 ) ;
#64951 = ORIENTED_EDGE ( 'NONE', *, *, #88714, .T. ) ;
#64952 = CARTESIAN_POINT ( 'NONE',  ( -6.185411026474866958, -5.876774720514411854, 19.34586827028016742 ) ) ;
#64953 = CARTESIAN_POINT ( 'NONE',  ( -69.85571445902073151, -25.30060019737137367, 6.009288023823078362 ) ) ;
#64954 = ORIENTED_EDGE ( 'NONE', *, *, #64488, .T. ) ;
#64955 = CARTESIAN_POINT ( 'NONE',  ( -129.6228709571500417, -29.50250243563736774, 8.947779886222132717 ) ) ;
#64956 = ORIENTED_EDGE ( 'NONE', *, *, #993, .T. ) ;
#64957 = FACE_OUTER_BOUND ( 'NONE', #53581, .T. ) ;
#64958 = CARTESIAN_POINT ( 'NONE',  ( 12.60132613692001691, 16.66296579206088069, -1.500000000000002220 ) ) ;
#64959 = EDGE_CURVE ( 'NONE', #80762, #41069, #32485, .T. ) ;
#64960 = CARTESIAN_POINT ( 'NONE',  ( 21.14253370195585546, 5.708146584608840612, 11.49999999999999645 ) ) ;
#64961 = B_SPLINE_CURVE_WITH_KNOTS ( 'NONE', 3,
 ( #47064, #71399, #77978, #39442 ),
 .UNSPECIFIED., .F., .F.,
 ( 4, 4 ),
 ( 0.000000000000000000, 0.001749918372063935697 ),
 .UNSPECIFIED. ) ;
#64962 = FACE_OUTER_BOUND ( 'NONE', #42007, .T. ) ;
#64963 = DIRECTION ( 'NONE',  ( -1.000000000000000000, -0.000000000000000000, 0.000000000000000000 ) ) ;
#64964 = CARTESIAN_POINT ( 'NONE',  ( -1.726696889551340153, 22.42386595106472669, -1.500000000000002220 ) ) ;
#64965 = CARTESIAN_POINT ( 'NONE',  ( 19.98859412959824411, 6.261702723725245612, -1.500000000000002220 ) ) ;
#64966 = CARTESIAN_POINT ( 'NONE',  ( -26.22762954581084571, -24.88148982559359723, 6.176716197550690346 ) ) ;
#64967 = DIRECTION ( 'NONE',  ( 0.9975640502598243087, -0.06975647374412546897, -0.000000000000000000 ) ) ;
#64968 = CARTESIAN_POINT ( 'NONE',  ( -121.6228709571500417, -23.47593901973091235, -1.443836447538997536 ) ) ;
#64969 = ORIENTED_EDGE ( 'NONE', *, *, #47260, .F. ) ;
#64970 = ORIENTED_EDGE ( 'NONE', *, *, #16073, .F. ) ;
#64971 = ORIENTED_EDGE ( 'NONE', *, *, #44281, .T. ) ;
#64972 = CARTESIAN_POINT ( 'NONE',  ( -52.62368446719793269, -24.65952944569304606, 1.056160979905696573 ) ) ;
#64973 = EDGE_LOOP ( 'NONE', ( #99837, #60531, #17417, #27430, #88934, #5131, #67171 ) ) ;
#64974 = CARTESIAN_POINT ( 'NONE',  ( 11.27511198983438412, 18.17944245918264912, -1.500000000000002220 ) ) ;
#64975 = EDGE_LOOP ( 'NONE', ( #40996, #4598, #86510, #29618 ) ) ;
#64976 = CARTESIAN_POINT ( 'NONE',  ( -28.62287095715004881, -23.31957264754183967, 11.44779298504227860 ) ) ;
#64977 = CARTESIAN_POINT ( 'NONE',  ( 17.50165659415881336, 11.77592616506222711, 11.49999999999998934 ) ) ;
#64978 = CARTESIAN_POINT ( 'NONE',  ( -30.44146006906462532, -24.26584525523073665, 9.960304333224314632 ) ) ;
#64979 = CARTESIAN_POINT ( 'NONE',  ( 2.677468215678941110, -6.376774720514418959, 20.83735685176740304 ) ) ;
#64980 = FACE_OUTER_BOUND ( 'NONE', #48005, .T. ) ;
#64981 = CARTESIAN_POINT ( 'NONE',  ( -101.5089468450591994, -24.65952944569305316, 1.056160979905706121 ) ) ;
#64982 = CARTESIAN_POINT ( 'NONE',  ( -109.5706907882233025, -25.31518732623182899, 4.855924937824241283 ) ) ;
#64983 = CARTESIAN_POINT ( 'NONE',  ( 19.90762846840230083, -9.494064324355022677, -1.500000000000002220 ) ) ;
#64984 = ORIENTED_EDGE ( 'NONE', *, *, #37521, .F. ) ;
#64985 = CARTESIAN_POINT ( 'NONE',  ( -65.49046995964316409, -24.73531770709095312, 8.716586749053508498 ) ) ;
#64986 = DIRECTION ( 'NONE',  ( 2.352173255807796549E-16, -0.000000000000000000, -1.000000000000000000 ) ) ;
#64987 = CARTESIAN_POINT ( 'NONE',  ( -60.62578254086317742, -24.92564183028978420, 1.928384488918252648 ) ) ;
#64988 = ADVANCED_FACE ( 'NONE', ( #27812 ), #33426, .F. ) ;
#64989 = CARTESIAN_POINT ( 'NONE',  ( -25.51202922834713149, -24.77321340604576960, 7.214475432169975555 ) ) ;
#64990 = DIRECTION ( 'NONE',  ( 0.000000000000000000, -1.000000000000000000, 0.000000000000000000 ) ) ;
#64991 = CARTESIAN_POINT ( 'NONE',  ( 5.097264368846809113, 1.579225279485572342, -27.56135813788808875 ) ) ;
#64992 = CARTESIAN_POINT ( 'NONE',  ( -0.3244385709253747585, -21.36021439428519386, -1.500000000000002220 ) ) ;
#64993 = CARTESIAN_POINT ( 'NONE',  ( -81.52287095715009002, -24.50216790748205398, 0.6166512839542526159 ) ) ;
#64994 = CARTESIAN_POINT ( 'NONE',  ( -52.58953762381672448, -23.48783264082478794, -1.443836473390070596 ) ) ;
#64995 = CIRCLE ( 'NONE', #29247, 1.325999999999943446 ) ;
#64996 = ADVANCED_FACE ( 'NONE', ( #42059 ), #45048, .F. ) ;
#64997 = DIRECTION ( 'NONE',  ( 0.000000000000000000, 0.000000000000000000, 1.000000000000000000 ) ) ;
#64998 = CARTESIAN_POINT ( 'NONE',  ( -19.80875734969026425, 0.3587747205144265483, 31.02402280011862246 ) ) ;
#64999 = CARTESIAN_POINT ( 'NONE',  ( 0.2737972009257602091, 22.58959237946467624, -1.500000000000002220 ) ) ;
#65000 = CARTESIAN_POINT ( 'NONE',  ( -112.6228709571500559, -23.47593901973091235, -1.443836447538999312 ) ) ;
#65001 = ORIENTED_EDGE ( 'NONE', *, *, #42111, .F. ) ;
#65002 = CARTESIAN_POINT ( 'NONE',  ( -50.51965600136372103, -25.31394903530583917, 5.202396475616230198 ) ) ;
#65003 = FACE_OUTER_BOUND ( 'NONE', #32112, .T. ) ;
#65004 = CARTESIAN_POINT ( 'NONE',  ( 18.24634267693259559, -7.554628487255452107, 11.49999999999999645 ) ) ;
#65005 = CARTESIAN_POINT ( 'NONE',  ( -93.52287095715006160, -23.48786465467241769, 11.44779295918254292 ) ) ;
#65006 = B_SPLINE_CURVE_WITH_KNOTS ( 'NONE', 3,
 ( #81294, #50355, #34631, #65600 ),
 .UNSPECIFIED., .F., .F.,
 ( 4, 4 ),
 ( 0.000000000000000000, 0.0001000000000000167422 ),
 .UNSPECIFIED. ) ;
#65007 = CARTESIAN_POINT ( 'NONE',  ( -67.60891996484096467, -23.48783264082477018, -1.443836473390094799 ) ) ;
#65008 = ORIENTED_EDGE ( 'NONE', *, *, #44738, .F. ) ;
#65009 = PLANE ( 'NONE',  #87937 ) ;
#65010 = CARTESIAN_POINT ( 'NONE',  ( -99.55620429048339304, -24.66019654487199730, 8.947790411086124607 ) ) ;
#65011 = DIRECTION ( 'NONE',  ( 0.000000000000000000, 0.000000000000000000, -1.000000000000000000 ) ) ;
#65012 = CARTESIAN_POINT ( 'NONE',  ( -13.01863397230089170, 17.21462230531794901, 11.49999999999998934 ) ) ;
#65013 = CARTESIAN_POINT ( 'NONE',  ( -91.52287095715006160, -23.47593901973090524, -1.443836447538996648 ) ) ;
#65014 = CARTESIAN_POINT ( 'NONE',  ( -76.62287095715007013, -24.66019654487199730, 8.947790411086128159 ) ) ;
#65015 = DIRECTION ( 'NONE',  ( 0.000000000000000000, 0.000000000000000000, -1.000000000000000000 ) ) ;
#65016 = DIRECTION ( 'NONE',  ( -3.773278334453080206E-23, 0.9999999999976377785, 2.173523156925979975E-06 ) ) ;
#65017 = CARTESIAN_POINT ( 'NONE',  ( -17.81549539028256746, -8.563599010019245839, -1.500000000000002220 ) ) ;
#65018 = AXIS2_PLACEMENT_3D ( 'NONE', #31249, #24136, #55103 ) ;
#65019 = ORIENTED_EDGE ( 'NONE', *, *, #15465, .F. ) ;
#65020 = AXIS2_PLACEMENT_3D ( 'NONE', #42029, #19162, #95794 ) ;
#65021 = CARTESIAN_POINT ( 'NONE',  ( 8.375906630400100639, -18.44307005126401933, 11.49999999999999645 ) ) ;
#65022 = CARTESIAN_POINT ( 'NONE',  ( -7.338700834008208496, -5.876774720514410966, 19.35116211686183263 ) ) ;
#65023 = EDGE_CURVE ( 'NONE', #41151, #35233, #75966, .T. ) ;
#65024 = APPROVAL ( #93665, 'UNSPECIFIED' ) ;
#65025 = EDGE_LOOP ( 'NONE', ( #46511, #20389, #10655, #100184 ) ) ;
#65026 = CARTESIAN_POINT ( 'NONE',  ( -67.52287095715006160, -24.66019654487199730, 8.947790411086115725 ) ) ;
#65027 = CARTESIAN_POINT ( 'NONE',  ( -99.58039134064964060, -25.28222918948337039, 4.246872970242233869 ) ) ;
#65028 = FACE_OUTER_BOUND ( 'NONE', #85747, .T. ) ;
#65029 = PLANE ( 'NONE',  #14291 ) ;
#65030 = LINE ( 'NONE', #9709, #11641 ) ;
#65031 = CARTESIAN_POINT ( 'NONE',  ( -32.07722060962682775, -25.11010177581465186, 2.831122766525584478 ) ) ;
#65032 = CARTESIAN_POINT ( 'NONE',  ( 14.85562765054232059, -13.46834898924134372, -1.500000000000002220 ) ) ;
#65033 = PLANE ( 'NONE',  #83967 ) ;
#65034 = VERTEX_POINT ( 'NONE', #97814 ) ;
#65035 = EDGE_CURVE ( 'NONE', #39486, #10502, #50641, .T. ) ;
#65036 = B_SPLINE_CURVE_WITH_KNOTS ( 'NONE', 3,
 ( #79479, #71883, #18574, #3379, #65783, #33300, #96698, #95210 ),
 .UNSPECIFIED., .F., .F.,
 ( 4, 2, 2, 4 ),
 ( 0.000000000000000000, 0.002001079623178230599, 0.003001619434767341561, 0.004002159246356452524 ),
 .UNSPECIFIED. ) ;
#65037 = CARTESIAN_POINT ( 'NONE',  ( -51.52287095715004739, -23.73907113216990084, -1.053371485793254791 ) ) ;
#65038 = FACE_OUTER_BOUND ( 'NONE', #80503, .T. ) ;
#65039 = CARTESIAN_POINT ( 'NONE',  ( -80.15554980868958523, -25.30558339281096636, 4.989559503397144269 ) ) ;
#65040 = B_SPLINE_CURVE_WITH_KNOTS ( 'NONE', 3,
 ( #21260, #29384, #43622, #38001 ),
 .UNSPECIFIED., .F., .F.,
 ( 4, 4 ),
 ( 0.000000000000000000, 1.000000000000000000 ),
 .UNSPECIFIED. ) ;
#65041 = CARTESIAN_POINT ( 'NONE',  ( -10.11875734969026297, -6.376774720514426953, 30.51402280011862089 ) ) ;
#65042 = CARTESIAN_POINT ( 'NONE',  ( -100.7591363217603231, -25.11633374933415652, 2.865693444292612746 ) ) ;
#65043 = CARTESIAN_POINT ( 'NONE',  ( 15.63775912259742995, 4.567193422986040474, -28.22903731538627525 ) ) ;
#65044 = CARTESIAN_POINT ( 'NONE',  ( -84.62287095715005592, -24.64898659630367561, 1.056161002820826145 ) ) ;
#65045 = ORIENTED_EDGE ( 'NONE', *, *, #33047, .T. ) ;
#65046 = CARTESIAN_POINT ( 'NONE',  ( -19.38859340154505873, -6.080128201517944753, -1.500000000000002220 ) ) ;
#65047 = VERTEX_POINT ( 'NONE', #90709 ) ;
#65048 = EDGE_CURVE ( 'NONE', #50583, #37074, #59265, .T. ) ;
#65049 = CARTESIAN_POINT ( 'NONE',  ( 31.62080439023052492, 4.380055315099236957, 26.73348078282562668 ) ) ;
#65050 = CARTESIAN_POINT ( 'NONE',  ( -118.5562042904834072, -23.47596703998600631, 11.44779298504227683 ) ) ;
#65051 = ORIENTED_EDGE ( 'NONE', *, *, #6915, .F. ) ;
#65052 = CARTESIAN_POINT ( 'NONE',  ( -127.6228709571500559, -29.50247984919015209, -1.443849546365044922 ) ) ;
#65053 = B_SPLINE_CURVE_WITH_KNOTS ( 'NONE', 3,
 ( #18349, #17852, #88363, #80247 ),
 .UNSPECIFIED., .F., .F.,
 ( 4, 4 ),
 ( 0.000000000000000000, 1.000000000000000000 ),
 .UNSPECIFIED. ) ;
#65054 = CARTESIAN_POINT ( 'NONE',  ( 15.03820766250734309, 3.514597374712530531, -27.31689629941529773 ) ) ;
#65055 = LINE ( 'NONE', #2636, #44796 ) ;
#65056 = CARTESIAN_POINT ( 'NONE',  ( 13.55612473118199723, -16.30799122071102403, 11.49999999999999645 ) ) ;
#65057 = CARTESIAN_POINT ( 'NONE',  ( 4.116201370682176730, 21.75534844777131838, -1.500000000000002220 ) ) ;
#65058 = VECTOR ( 'NONE', #82551, 1000.000000000000227 ) ;
#65059 = EDGE_CURVE ( 'NONE', #33073, #49749, #90210, .T. ) ;
#65060 = CARTESIAN_POINT ( 'NONE',  ( 18.80685554986811070, -8.408966509905500430, -1.500000000000002220 ) ) ;
#65061 = EDGE_LOOP ( 'NONE', ( #82316, #86117, #49587, #86317 ) ) ;
#65062 = FACE_OUTER_BOUND ( 'NONE', #36134, .T. ) ;
#65063 = ORIENTED_EDGE ( 'NONE', *, *, #77633, .F. ) ;
#65064 = CARTESIAN_POINT ( 'NONE',  ( 7.111284305517425075, -6.376774720514422512, 21.05363841023157434 ) ) ;
#65065 = CARTESIAN_POINT ( 'NONE',  ( -50.52287095715006870, -24.51254535375842636, 9.355368624242256459 ) ) ;
#65066 = VERTEX_POINT ( 'NONE', #92198 ) ;
#65067 = ORIENTED_EDGE ( 'NONE', *, *, #70272, .T. ) ;
#65068 = VERTEX_POINT ( 'NONE', #22675 ) ;
#65069 = DIRECTION ( 'NONE',  ( 0.000000000000000000, -0.000000000000000000, -1.000000000000000000 ) ) ;
#65070 = CARTESIAN_POINT ( 'NONE',  ( 6.509931258083027750, -5.876774720514417183, 20.09204137875607188 ) ) ;
#65071 = DIRECTION ( 'NONE',  ( 0.7071067811865516806, 0.7071067811865434649, 0.000000000000000000 ) ) ;
#65072 = CARTESIAN_POINT ( 'NONE',  ( 20.68991284688621946, 0.5745778482356619365, -1.500000000000002220 ) ) ;
#65073 = EDGE_CURVE ( 'NONE', #14044, #41241, #86930, .T. ) ;
#65074 = CARTESIAN_POINT ( 'NONE',  ( 2.849777056880220982, 21.50153301832798647, 11.49999999999999645 ) ) ;
#65075 = EDGE_LOOP ( 'NONE', ( #88784, #51610, #86168, #12312 ) ) ;
#65076 = CARTESIAN_POINT ( 'NONE',  ( -127.5228709571500616, -24.65952944569304606, 1.056160979905707675 ) ) ;
#65077 = CARTESIAN_POINT ( 'NONE',  ( -28.62287095715004881, -23.33150569529546914, 11.44779297407613150 ) ) ;
#65078 = CARTESIAN_POINT ( 'NONE',  ( -12.73782554413503654, -18.45060914899308457, 11.49999999999998934 ) ) ;
#65079 = EDGE_CURVE ( 'NONE', #86743, #63165, #13058, .T. ) ;
#65080 = CARTESIAN_POINT ( 'NONE',  ( -93.52287095715006160, -23.47593901973090524, -1.443836447538996648 ) ) ;
#65081 = LINE ( 'NONE', #73661, #67543 ) ;
#65082 = VERTEX_POINT ( 'NONE', #29303 ) ;
#65083 = CARTESIAN_POINT ( 'NONE',  ( 29.74616903497430442, 6.356993644837154456, 26.56043482791313082 ) ) ;
#65084 = VECTOR ( 'NONE', #47757, 1000.000000000000000 ) ;
#65085 = CYLINDRICAL_SURFACE ( 'NONE', #78246, 1.000000000000000888 ) ;
#65086 = CC_DESIGN_APPROVAL ( #65024, ( #3602 ) ) ;
#65087 = VERTEX_POINT ( 'NONE', #52150 ) ;
#65088 = ORIENTED_EDGE ( 'NONE', *, *, #62771, .F. ) ;
#65089 = CARTESIAN_POINT ( 'NONE',  ( -103.6228709571500559, -24.64898659630368627, 1.056161002820829697 ) ) ;
#65090 = VERTEX_POINT ( 'NONE', #13070 ) ;
#65091 = CARTESIAN_POINT ( 'NONE',  ( -18.66175431467001999, 10.11895122522205526, -1.500000000000002220 ) ) ;
#65092 = EDGE_LOOP ( 'NONE', ( #88672, #7918, #63832, #91836 ) ) ;
#65093 = FACE_OUTER_BOUND ( 'NONE', #31575, .T. ) ;
#65094 = CARTESIAN_POINT ( 'NONE',  ( 8.176594470695947692, -20.27425322898990601, -1.500000000000002220 ) ) ;
#65095 = CARTESIAN_POINT ( 'NONE',  ( -52.65164253565483676, -23.73791477778911840, 11.05961554403171299 ) ) ;
#65096 = CARTESIAN_POINT ( 'NONE',  ( -40.84535658588885099, -25.18430885309796352, 3.358264732341272651 ) ) ;
#65097 = DIRECTION ( 'NONE',  ( -3.773278334453079618E-23, 0.9999999999976377785, 2.173523156925979975E-06 ) ) ;
#65098 = CARTESIAN_POINT ( 'NONE',  ( 18.42579859434530931, 11.83097890990371148, -1.500000000000002220 ) ) ;
#65099 = CARTESIAN_POINT ( 'NONE',  ( 6.627987042499408510, -6.376774720514424288, 21.45334999081212146 ) ) ;
#65100 = ORIENTED_EDGE ( 'NONE', *, *, #91665, .F. ) ;
#65101 = CARTESIAN_POINT ( 'NONE',  ( -69.62287095715005592, -24.34917612406838572, 0.1852690917426620121 ) ) ;
#65102 = CYLINDRICAL_SURFACE ( 'NONE', #28221, 6.099999999999999645 ) ;
#65103 = VERTEX_POINT ( 'NONE', #98811 ) ;
#65104 = CARTESIAN_POINT ( 'NONE',  ( -30.57692235644935153, -25.30655462701041714, 5.551177274637566939 ) ) ;
#65105 = VERTEX_POINT ( 'NONE', #22178 ) ;
#65106 = CARTESIAN_POINT ( 'NONE',  ( -113.5562042904833930, -23.47593901973091235, -1.443836447538999312 ) ) ;
#65107 = CARTESIAN_POINT ( 'NONE',  ( -82.50964971285777949, -24.15543982623907482, -0.2315651400026498552 ) ) ;
#65108 = CARTESIAN_POINT ( 'NONE',  ( -12.22836702412972087, 17.35733969022439993, 11.49999999999998934 ) ) ;
#65109 = LINE ( 'NONE', #86911, #85484 ) ;
#65110 = CARTESIAN_POINT ( 'NONE',  ( -130.5728709571500588, -24.88273649812091293, 8.549170486301877148 ) ) ;
#65111 = CARTESIAN_POINT ( 'NONE',  ( -1.044871794871790938, -6.376774720514427841, 21.75000000000000355 ) ) ;
#65112 = CARTESIAN_POINT ( 'NONE',  ( -129.5228709571500758, -24.65952944569305316, 1.056160979905707675 ) ) ;
#65113 = CARTESIAN_POINT ( 'NONE',  ( -18.68671320864135765, 5.291888989699490509, -1.500000000000002220 ) ) ;
#65114 = ADVANCED_FACE ( 'NONE', ( #5471 ), #84587, .T. ) ;
#65115 = AXIS2_PLACEMENT_3D ( 'NONE', #51095, #75405, #60211 ) ;
#65116 = CARTESIAN_POINT ( 'NONE',  ( -45.47189084317965069, -25.00158670708910336, 2.256160236439225031 ) ) ;
#65117 = VERTEX_POINT ( 'NONE', #53159 ) ;
#65118 = CARTESIAN_POINT ( 'NONE',  ( 18.62133539762988121, 6.091496293051981148, 11.49999999999999645 ) ) ;
#65119 = CARTESIAN_POINT ( 'NONE',  ( -5.576843645946834016, -6.376774720514418959, 20.41272575174755133 ) ) ;
#65120 = DIRECTION ( 'NONE',  ( -1.000000000000000000, 0.000000000000000000, 0.000000000000000000 ) ) ;
#65121 = ORIENTED_EDGE ( 'NONE', *, *, #2377, .T. ) ;
#65122 = CARTESIAN_POINT ( 'NONE',  ( -97.52287095715010423, -23.48783264082477018, -1.443836473390087027 ) ) ;
#65123 = CARTESIAN_POINT ( 'NONE',  ( -89.51148841281252544, -24.15543982623907837, -0.2315651400026483009 ) ) ;
#65124 = DIRECTION ( 'NONE',  ( -0.1478094111296165691, 0.9890158633619158257, -6.377659838150018832E-17 ) ) ;
#65125 = CARTESIAN_POINT ( 'NONE',  ( -89.40841769935767047, -25.06732983082694943, 7.447789526168953955 ) ) ;
#65126 = CARTESIAN_POINT ( 'NONE',  ( 18.75866648459458830, -6.009157199652424453, -1.500000000000002220 ) ) ;
#65127 = VERTEX_POINT ( 'NONE', #84089 ) ;
#65128 = VECTOR ( 'NONE', #39893, 1000.000000000000000 ) ;
#65129 = CARTESIAN_POINT ( 'NONE',  ( -94.62287095715002749, -23.72747288104469732, -1.053458166803225682 ) ) ;
#65130 = DIRECTION ( 'NONE',  ( 1.000000000000000000, 3.773278334444167608E-23, 8.201307833595939069E-29 ) ) ;
#65131 = B_SPLINE_CURVE_WITH_KNOTS ( 'NONE', 3,
 ( #35699, #20452, #66675, #82853, #51425, #44316 ),
 .UNSPECIFIED., .F., .F.,
 ( 4, 2, 4 ),
 ( 0.000000000000000000, 0.001380901958385387677, 0.002761803916770775354 ),
 .UNSPECIFIED. ) ;
#65132 = ADVANCED_FACE ( 'NONE', ( #66893 ), #76463, .T. ) ;
#65133 = APPLICATION_PROTOCOL_DEFINITION ( 'international standard', 'config_control_design', 1994, #10995 ) ;
#65134 = ORIENTED_EDGE ( 'NONE', *, *, #66305, .F. ) ;
#65135 = FACE_OUTER_BOUND ( 'NONE', #56441, .T. ) ;
#65136 = CARTESIAN_POINT ( 'NONE',  ( -1.568769572606061535, -6.376774720514415407, 19.76359802465961835 ) ) ;
#65137 = CARTESIAN_POINT ( 'NONE',  ( -47.53539927575063473, -24.51314013834316086, 0.6176544820404172853 ) ) ;
#65138 = CARTESIAN_POINT ( 'NONE',  ( -105.6228709571500559, -24.92604778743017491, 8.074972756849359001 ) ) ;
#65140 = EDGE_CURVE ( 'NONE', #63171, #60621, #98586, .T. ) ;
#65139 = CARTESIAN_POINT ( 'NONE',  ( -79.91920829509126634, -25.20144873054373136, 6.835696071488102099 ) ) ;
#65141 = CARTESIAN_POINT ( 'NONE',  ( -69.51029376924685721, -25.24515128556519272, 5.710789870928137724 ) ) ;
#65142 = DIRECTION ( 'NONE',  ( 1.000000000000000000, 3.773278334444167608E-23, 8.201307833595939069E-29 ) ) ;
#65143 = CARTESIAN_POINT ( 'NONE',  ( 10.26108024787556516, -17.11367029881254709, 11.49999999999998934 ) ) ;
#65144 = FACE_OUTER_BOUND ( 'NONE', #17585, .T. ) ;
#65145 = CARTESIAN_POINT ( 'NONE',  ( -9.044204435542846809, 17.70297415775587169, -1.500000000000002220 ) ) ;
#65146 = VERTEX_POINT ( 'NONE', #6971 ) ;
#65147 = EDGE_CURVE ( 'NONE', #35959, #97546, #13570, .T. ) ;
#65148 = DIRECTION ( 'NONE',  ( 0.000000000000000000, 2.173523156925980399E-06, -0.9999999999976378895 ) ) ;
#65149 = EDGE_CURVE ( 'NONE', #41451, #65090, #37921, .T. ) ;
#65150 = B_SPLINE_CURVE_WITH_KNOTS ( 'NONE', 3,
 ( #88587, #41924, #65770, #87076 ),
 .UNSPECIFIED., .F., .F.,
 ( 4, 4 ),
 ( 0.000000000000000000, 9.999999999998897304E-05 ),
 .UNSPECIFIED. ) ;
#65151 = VECTOR ( 'NONE', #54771, 1000.000000000000114 ) ;
#65153 = EDGE_CURVE ( 'NONE', #8482, #40343, #86590, .T. ) ;
#65152 = APPROVAL_PERSON_ORGANIZATION ( #15420, #71746, #45396 ) ;
#65154 = CARTESIAN_POINT ( 'NONE',  ( -51.27260140835372937, -25.18295898317592219, 6.794811910356732376 ) ) ;
#65155 = CARTESIAN_POINT ( 'NONE',  ( -93.62287095715005592, -24.66019654487199730, 8.947790411086124607 ) ) ;
#65156 = CARTESIAN_POINT ( 'NONE',  ( -80.62685887991092670, -24.83644354573579349, 8.397322867130101898 ) ) ;
#65157 = CARTESIAN_POINT ( 'NONE',  ( -8.262104503270727207, -19.10415460921518971, 11.49999999999999645 ) ) ;
#65158 = LINE ( 'NONE', #49420, #85656 ) ;
#65159 = CARTESIAN_POINT ( 'NONE',  ( -60.22287095715005023, -23.47593901973090169, -1.443836447538997536 ) ) ;
#65160 = CARTESIAN_POINT ( 'NONE',  ( -21.14637036216210575, 8.611126525438130841, 11.49999999999999645 ) ) ;
#65161 = EDGE_LOOP ( 'NONE', ( #59445, #67092, #64472, #15493 ) ) ;
#65162 = DIRECTION ( 'NONE',  ( 1.000000000000000000, 0.000000000000000000, 0.000000000000000000 ) ) ;
#65163 = DIRECTION ( 'NONE',  ( 0.000000000000000000, 0.000000000000000000, 1.000000000000000000 ) ) ;
#65164 = ORIENTED_EDGE ( 'NONE', *, *, #24661, .F. ) ;
#65165 = CARTESIAN_POINT ( 'NONE',  ( 2.165584020960389822, 20.11889322763239107, 11.49999999999998934 ) ) ;
#65166 = EDGE_CURVE ( 'NONE', #57723, #91984, #24187, .T. ) ;
#65167 = CARTESIAN_POINT ( 'NONE',  ( 22.02124265030973760, 6.143225279485574397, 16.20402280011862217 ) ) ;
#65168 = LINE ( 'NONE', #43800, #10699 ) ;
#65169 = CARTESIAN_POINT ( 'NONE',  ( -84.52287095715007581, -24.33832256527049509, 0.1851278514138626485 ) ) ;
#65170 = ORIENTED_EDGE ( 'NONE', *, *, #3725, .F. ) ;
#65171 = CARTESIAN_POINT ( 'NONE',  ( -109.5562042904833504, -24.64965694238575367, 8.947790433994187609 ) ) ;
#65172 = DIRECTION ( 'NONE',  ( 1.000000000000000000, 0.000000000000000000, 0.000000000000000000 ) ) ;
#65173 = CARTESIAN_POINT ( 'NONE',  ( -3.050325703546597822, 19.74810961616558913, -1.500000000000002220 ) ) ;
#65174 = CARTESIAN_POINT ( 'NONE',  ( 18.73254098450790295, -9.497730595714260815, 11.49999999999999645 ) ) ;
#65175 = CARTESIAN_POINT ( 'NONE',  ( 10.86264265030973952, 5.965225279485574461, -28.05717073599341305 ) ) ;
#65176 = FACE_OUTER_BOUND ( 'NONE', #23357, .T. ) ;
#65177 = CARTESIAN_POINT ( 'NONE',  ( 19.90762846840230083, -9.494064324355022677, 11.49999999999998934 ) ) ;
#65178 = EDGE_CURVE ( 'NONE', #91571, #88013, #56538, .T. ) ;
#65179 = CARTESIAN_POINT ( 'NONE',  ( -5.023036858974361252, -6.376774720514410077, 19.14743589743590846 ) ) ;
#65180 = EDGE_LOOP ( 'NONE', ( #92468, #8498, #51396, #24234 ) ) ;
#65181 = VECTOR ( 'NONE', #89663, 1000.000000000000000 ) ;
#65182 = CARTESIAN_POINT ( 'NONE',  ( 14.76093561896378148, -3.316774720514426456, -26.55548769130088971 ) ) ;
#65183 = FACE_OUTER_BOUND ( 'NONE', #1783, .T. ) ;
#65184 = ADVANCED_FACE ( 'NONE', ( #31303 ), #6242, .T. ) ;
#65185 = CARTESIAN_POINT ( 'NONE',  ( -72.64440388517061820, -23.73766607897670156, -1.055555164236458454 ) ) ;
#65186 = CARTESIAN_POINT ( 'NONE',  ( -86.58953762381669605, -24.65952944569304606, 1.056160979905697239 ) ) ;
#65187 = ORIENTED_EDGE ( 'NONE', *, *, #91076, .F. ) ;
#65188 = VERTEX_POINT ( 'NONE', #87092 ) ;
#65189 = DIRECTION ( 'NONE',  ( 0.7512896232465891000, 1.109416176496794925E-16, 0.6599726524652351767 ) ) ;
#65190 = CARTESIAN_POINT ( 'NONE',  ( -101.1026865405329147, -25.10935838865034597, 2.999872854746632900 ) ) ;
#65191 = CARTESIAN_POINT ( 'NONE',  ( -4.930333147521421822, -5.876774720514410077, 19.46306892155547530 ) ) ;
#65192 = CARTESIAN_POINT ( 'NONE',  ( 15.48611046165106941, -13.43736321338083783, -1.500000000000002220 ) ) ;
#65193 = ADVANCED_FACE ( 'NONE', ( #93196 ), #85087, .F. ) ;
#65194 = ORIENTED_EDGE ( 'NONE', *, *, #9905, .T. ) ;
#65195 = CARTESIAN_POINT ( 'NONE',  ( -80.88924702628075636, -29.50249297023137629, 4.592912097770885715 ) ) ;
#65196 = CARTESIAN_POINT ( 'NONE',  ( -29.49875734969025842, -0.3587747205144265483, 17.86602280011862476 ) ) ;
#65197 = CARTESIAN_POINT ( 'NONE',  ( -103.6228709571500559, -24.64965695001469115, 8.947790433994178727 ) ) ;
#65198 = CARTESIAN_POINT ( 'NONE',  ( -1.228339276683141579, -22.28195500894762660, -1.500000000000002220 ) ) ;
#65199 = EDGE_CURVE ( 'NONE', #27742, #87028, #100202, .T. ) ;
#65200 = CARTESIAN_POINT ( 'NONE',  ( 29.77147767949874790, -5.356774720514425603, 26.15915692125051706 ) ) ;
#65201 = CARTESIAN_POINT ( 'NONE',  ( -122.2228709571500502, -23.47596703998600631, 11.44779298504227860 ) ) ;
#65202 = VERTEX_POINT ( 'NONE', #76965 ) ;
#65203 = EDGE_CURVE ( 'NONE', #41305, #16459, #46537, .T. ) ;
#65204 = CARTESIAN_POINT ( 'NONE',  ( -42.62287095715004881, -24.64898659630367561, 1.056161002820819261 ) ) ;
#65205 = CARTESIAN_POINT ( 'NONE',  ( -51.69691692161301688, -25.27141761418660337, 4.090265752574888225 ) ) ;
#65206 = AXIS2_PLACEMENT_3D ( 'NONE', #24163, #86067, #47517 ) ;
#65207 = CARTESIAN_POINT ( 'NONE',  ( -19.30504728598367237, -7.930543132070424051, 11.49999999999998934 ) ) ;
#65208 = CIRCLE ( 'NONE', #76456, 3.979149600822063704 ) ;
#65209 = ORIENTED_EDGE ( 'NONE', *, *, #94958, .F. ) ;
#65211 = ORIENTED_EDGE ( 'NONE', *, *, #29767, .F. ) ;
#65210 = CARTESIAN_POINT ( 'NONE',  ( -74.52287095715007581, -23.48783264082476308, -1.443836473390090802 ) ) ;
#65212 = VERTEX_POINT ( 'NONE', #77463 ) ;
#65213 = CARTESIAN_POINT ( 'NONE',  ( -69.47374562227740569, -25.25935290055894100, 7.284000681396445742 ) ) ;
#65214 = CARTESIAN_POINT ( 'NONE',  ( 3.661087877195506213, -20.73962600213626217, -1.500000000000002220 ) ) ;
#65215 = ORIENTED_EDGE ( 'NONE', *, *, #88602, .F. ) ;
#65216 = DIRECTION ( 'NONE',  ( -3.773278334453079030E-23, 0.9999999999976377785, 2.173523156925979128E-06 ) ) ;
#65217 = CARTESIAN_POINT ( 'NONE',  ( -37.52287095715006870, -23.47596703998600631, 11.44779298504229281 ) ) ;
#65218 = CARTESIAN_POINT ( 'NONE',  ( -103.6228709571500559, -29.50248528299804818, 1.056150453629042030 ) ) ;
#65219 = B_SPLINE_CURVE_WITH_KNOTS ( 'NONE', 3,
 ( #9603, #54792, #70506, #79107, #31439, #85727, #997, #93837, #77599, #78095, #40563, #94333, #62400, #38552, #1503, #56302, #92829, #86226, #31945, #93329, #8609, #17211, #55297, #9101, #39051, #23312 ),
 .UNSPECIFIED., .F., .F.,
 ( 4, 2, 2, 2, 2, 2, 2, 2, 2, 2, 2, 2, 4 ),
 ( 6.348815807395609649E-06, 0.001695567397426964206, 0.002540176688236749167, 0.003384785979046533045, 0.004229395269856312152, 0.005074004560666090825, 0.006763223142285652509, 0.007607832433095433784, 0.008452441723905215060, 0.01014166030552477935, 0.01098626959633456149, 0.01183087888714434363, 0.01352009746876390618 ),
 .UNSPECIFIED. ) ;
#65220 = CARTESIAN_POINT ( 'NONE',  ( -101.6955034991685238, -25.25419416351397217, 6.928825754601663611 ) ) ;
#65221 = LINE ( 'NONE', #5280, #98336 ) ;
#65222 = CARTESIAN_POINT ( 'NONE',  ( 19.61570337458852364, 9.273991169892711994, -1.500000000000002220 ) ) ;
#65223 = CARTESIAN_POINT ( 'NONE',  ( -80.94627791849588050, -25.12224370068017620, 7.000535761828535541 ) ) ;
#65225 = VERTEX_POINT ( 'NONE', #69370 ) ;
#65224 = CARTESIAN_POINT ( 'NONE',  ( -22.27612280437926273, 0.2766752662994830247, 11.49999999999999645 ) ) ;
#65226 = CARTESIAN_POINT ( 'NONE',  ( -50.72223433783125301, -25.24728732082473570, 5.237078820334065909 ) ) ;
#65227 = DIRECTION ( 'NONE',  ( 0.000000000000000000, 1.000000000000000000, 0.000000000000000000 ) ) ;
#65228 = CARTESIAN_POINT ( 'NONE',  ( -69.55620429048339304, -23.48786465467241058, 11.44779295918255002 ) ) ;
#65229 = ORIENTED_EDGE ( 'NONE', *, *, #29742, .T. ) ;
#65231 = ORIENTED_EDGE ( 'NONE', *, *, #100148, .T. ) ;
#65230 = CARTESIAN_POINT ( 'NONE',  ( 8.971512145086521173, -7.528487854913501920, 4.500000000000000888 ) ) ;
#65232 = AXIS2_PLACEMENT_3D ( 'NONE', #4481, #57770, #13563 ) ;
#65233 = EDGE_LOOP ( 'NONE', ( #33878, #47143, #80403, #90230 ) ) ;
#65234 = SECURITY_CLASSIFICATION ( '', '', #10817 ) ;
#65235 = CARTESIAN_POINT ( 'NONE',  ( 31.31121903262429029, -5.174141622015902442, 0.9154248472334550746 ) ) ;
#65236 = B_SPLINE_CURVE_WITH_KNOTS ( 'NONE', 3,
 ( #51472, #99117, #5285, #90028, #37239, #28626 ),
 .UNSPECIFIED., .F., .F.,
 ( 4, 2, 4 ),
 ( 6.391158118959990520E-06, 0.001387004593080779424, 0.002767618028042598960 ),
 .UNSPECIFIED. ) ;
#65237 = B_SPLINE_CURVE_WITH_KNOTS ( 'NONE', 3,
 ( #34654, #87428, #73218, #18421 ),
 .UNSPECIFIED., .F., .F.,
 ( 4, 4 ),
 ( 0.4991261060968514851, 0.5001268531376167337 ),
 .UNSPECIFIED. ) ;
#65238 = FACE_OUTER_BOUND ( 'NONE', #68405, .T. ) ;
#65239 = CARTESIAN_POINT ( 'NONE',  ( -32.62287095715007013, -24.34917612406838217, 0.1852690917426584039 ) ) ;
#65240 = ORIENTED_EDGE ( 'NONE', *, *, #52760, .F. ) ;
#65241 = CARTESIAN_POINT ( 'NONE',  ( -130.5728709571500303, -25.10882183463795414, 2.294997381946255022 ) ) ;
#65242 = CARTESIAN_POINT ( 'NONE',  ( -10.09097066620046235, 20.03973272787133553, -1.500000000000002220 ) ) ;
#65243 = VERTEX_POINT ( 'NONE', #9468 ) ;
#65244 = CARTESIAN_POINT ( 'NONE',  ( -89.40841769935764205, -25.19340450609639603, 6.757884810842872625 ) ) ;
#65245 = CARTESIAN_POINT ( 'NONE',  ( -96.52287095715006160, -23.48786465467241769, 11.44779295918254114 ) ) ;
#65246 = CARTESIAN_POINT ( 'NONE',  ( 2.650685085285006348, -6.376774720514410077, 19.28073557658628445 ) ) ;
#65247 = B_SPLINE_CURVE_WITH_KNOTS ( 'NONE', 3,
 ( #7818, #94549, #24538, #23021, #46890, #30660, #76812, #25038, #61630, #85947, #70224, #84939, #15424, #40274, #704, #31651 ),
 .UNSPECIFIED., .F., .F.,
 ( 4, 2, 2, 2, 2, 2, 2, 4 ),
 ( 0.000000000000000000, 0.0002745580509702497183, 0.0005491161019404994367, 0.0008236741529107492093, 0.001098232203880998873, 0.001647348305821530077, 0.001921906356791795679, 0.002196464407762061498 ),
 .UNSPECIFIED. ) ;
#65248 = DIRECTION ( 'NONE',  ( 0.000000000000000000, 0.000000000000000000, 1.000000000000000000 ) ) ;
#65249 = CARTESIAN_POINT ( 'NONE',  ( -130.5728709571500588, -24.75179208683297460, 8.640809912072082710 ) ) ;
#65250 = CARTESIAN_POINT ( 'NONE',  ( 8.161054176536994831, -17.82452852192863091, -1.500000000000002220 ) ) ;
#65251 = B_SPLINE_SURFACE_WITH_KNOTS ( 'NONE', 3, 3, ( 
 ( #58866, #65007, #80699, #73098 ),
 ( #96923, #10692, #95922, #3588 ),
 ( #25911, #4585, #26417, #89808 ),
 ( #42657, #73591, #57389, #66505 ),
 ( #34531, #18303, #35535, #50258 ),
 ( #12173, #20278, #4080, #96425 ),
 ( #35032, #81198, #51249, #82189 ) ),
 .UNSPECIFIED., .F., .F., .F.,
 ( 4, 3, 4 ),
 ( 4, 4 ),
 ( 0.0004766839783816928175, 0.1029713700210893867, 0.2054660560637970868 ),
 ( 0.6296541705118287036, 0.6309574163451897588 ),
 .UNSPECIFIED. ) ;
#65252 = CARTESIAN_POINT ( 'NONE',  ( -49.87546937309745232, -25.30911630651809574, 4.600197623896191246 ) ) ;
#65253 = ORIENTED_EDGE ( 'NONE', *, *, #59043, .T. ) ;
#65254 = CARTESIAN_POINT ( 'NONE',  ( 4.075586527997184128, 21.15050231453075824, 11.49999999999998934 ) ) ;
#65255 = CARTESIAN_POINT ( 'NONE',  ( -20.27875734969026311, 6.143225279485574397, 26.25402280011862288 ) ) ;
#65256 = LINE ( 'NONE', #97173, #46445 ) ;
#65257 = CARTESIAN_POINT ( 'NONE',  ( -53.52287095715006870, -23.47596703998600631, 11.44779298504229104 ) ) ;
#65258 = LINE ( 'NONE', #35287, #73111 ) ;
#65259 = CARTESIAN_POINT ( 'NONE',  ( 22.59171682324826236, -3.780823453261925593, -1.500000000000002220 ) ) ;
#65260 = AXIS2_PLACEMENT_3D ( 'NONE', #100248, #86552, #17037 ) ;
#65261 = ADVANCED_FACE ( 'NONE', ( #31812 ), #92040, .T. ) ;
#65262 = APPROVAL_STATUS ( 'not_yet_approved' ) ;
#65263 = LINE ( 'NONE', #49019, #95267 ) ;
#65264 = CARTESIAN_POINT ( 'NONE',  ( -53.62368173164319529, -24.65952944569304250, 1.056160979905695463 ) ) ;
#65265 = CARTESIAN_POINT ( 'NONE',  ( -18.95788008782500356, -6.583919088883305015, 11.49999999999999645 ) ) ;
#65266 = DIRECTION ( 'NONE',  ( -1.000000000000000000, -0.000000000000000000, -0.000000000000000000 ) ) ;
#65267 = CARTESIAN_POINT ( 'NONE',  ( -31.52287095715006160, -24.65952944569304606, 1.056160979905690134 ) ) ;
#65268 = EDGE_CURVE ( 'NONE', #46589, #31325, #31214, .T. ) ;
#65269 = CARTESIAN_POINT ( 'NONE',  ( -59.52287095715006160, -29.50248528299804818, 1.056150453629034924 ) ) ;
#65270 = CARTESIAN_POINT ( 'NONE',  ( -41.32836283488544638, 5.152774720514427642, 39.26872235229541985 ) ) ;
#65271 = DIRECTION ( 'NONE',  ( 0.000000000000000000, -1.000000000000000000, 0.000000000000000000 ) ) ;
#65272 = CARTESIAN_POINT ( 'NONE',  ( -18.60049703728633474, -6.982253431394513932, -1.500000000000002220 ) ) ;
#65273 = EDGE_CURVE ( 'NONE', #74181, #20569, #73867, .T. ) ;
#65274 = LINE ( 'NONE', #10446, #2633 ) ;
#65275 = CARTESIAN_POINT ( 'NONE',  ( -19.47062899137607772, 3.135797168518691169, -1.500000000000002220 ) ) ;
#65276 = ADVANCED_FACE ( 'NONE', ( #96214 ), #19074, .T. ) ;
#65277 = EDGE_CURVE ( 'NONE', #17423, #58197, #57843, .T. ) ;
#65278 = CALENDAR_DATE ( 2026, 9, 10 ) ;
#65279 = AXIS2_PLACEMENT_3D ( 'NONE', #24536, #77805, #55505 ) ;
#65280 = EDGE_CURVE ( 'NONE', #11225, #70943, #65036, .T. ) ;
#65281 = CARTESIAN_POINT ( 'NONE',  ( 15.30669617938070459, 3.316774720514427344, -28.51986056384665957 ) ) ;
#65282 = CARTESIAN_POINT ( 'NONE',  ( -111.5228709571501042, -23.96127896941632685, -0.6493128931037972507 ) ) ;
#65283 = CARTESIAN_POINT ( 'NONE',  ( 4.697267095454844998, -20.06606415395816967, 11.49999999999999645 ) ) ;
#65284 = CARTESIAN_POINT ( 'NONE',  ( -49.52287095715006160, -29.50250786944525672, 11.44777988621624054 ) ) ;
#65285 = CARTESIAN_POINT ( 'NONE',  ( -21.72567761722203628, 6.514095075961352954, 11.49999999999999645 ) ) ;
#65286 = ORIENTED_EDGE ( 'NONE', *, *, #34116, .T. ) ;
#65287 = CARTESIAN_POINT ( 'NONE',  ( -69.34384048089543739, -25.12218957384244788, 6.239613635728673557 ) ) ;
#65288 = CARTESIAN_POINT ( 'NONE',  ( -51.29483375901499898, -25.27820168282615754, 4.047861613338572084 ) ) ;
#65289 = EDGE_CURVE ( 'NONE', #30127, #36030, #42440, .T. ) ;
#65290 = CARTESIAN_POINT ( 'NONE',  ( -27.65532027823855543, -24.61460113667579819, 8.251097176666958077 ) ) ;
#65291 = CARTESIAN_POINT ( 'NONE',  ( -56.52287095715006870, -23.48786465467241058, 11.44779295918254824 ) ) ;
#65292 = ORIENTED_EDGE ( 'NONE', *, *, #71297, .F. ) ;
#65293 = VECTOR ( 'NONE', #92530, 1000.000000000000000 ) ;
#65294 = EDGE_CURVE ( 'NONE', #28213, #88368, #20246, .T. ) ;
#65295 = CARTESIAN_POINT ( 'NONE',  ( -27.13414387080440093, 5.965225279485594001, -10.21530720150730254 ) ) ;
#65296 = CARTESIAN_POINT ( 'NONE',  ( 17.70901601935662839, 14.43836031950349152, -1.500000000000002220 ) ) ;
#65297 = CARTESIAN_POINT ( 'NONE',  ( -105.5228709571500616, -24.99132157543084887, 2.256160258750667502 ) ) ;
#65298 = DIRECTION ( 'NONE',  ( -0.7689940216596065081, 0.000000000000000000, 0.6392559695863502256 ) ) ;
#65299 = CARTESIAN_POINT ( 'NONE',  ( -82.59968746745757073, -23.73791477778911840, 11.05961554403170766 ) ) ;
#65300 = CC_DESIGN_SECURITY_CLASSIFICATION ( #14993, ( #100421 ) ) ;
#65301 = CARTESIAN_POINT ( 'NONE',  ( -5.125883829288005344, 21.89707322345674712, 11.49999999999999645 ) ) ;
#65302 = ORIENTED_EDGE ( 'NONE', *, *, #94197, .F. ) ;
#65303 = CARTESIAN_POINT ( 'NONE',  ( -89.81226385320383088, -25.19340450609436743, 6.757884810855529167 ) ) ;
#65304 = CARTESIAN_POINT ( 'NONE',  ( 18.29167757401336303, -12.14499471347784798, 11.49999999999998934 ) ) ;
#65305 = CARTESIAN_POINT ( 'NONE',  ( 32.58581522646812090, 4.151341569991283897, -4.025368652865530805 ) ) ;
#65306 = EDGE_CURVE ( 'NONE', #28558, #29452, #41425, .T. ) ;
#65307 = DIRECTION ( 'NONE',  ( 0.000000000000000000, 1.000000000000000000, 0.000000000000000000 ) ) ;
#65308 = CARTESIAN_POINT ( 'NONE',  ( -112.5562042904833930, -24.64965694238575011, 8.947790433994189385 ) ) ;
#65309 = VECTOR ( 'NONE', #44018, 1000.000000000000114 ) ;
#65310 = VERTEX_POINT ( 'NONE', #58646 ) ;
#65311 = CARTESIAN_POINT ( 'NONE',  ( -116.5228709571501042, -23.47593901973090524, -1.443836447538996426 ) ) ;
#65312 = CARTESIAN_POINT ( 'NONE',  ( -0.2200237740140755516, -6.376774720514408301, 19.17724329193115551 ) ) ;
#65313 = ORIENTED_EDGE ( 'NONE', *, *, #45606, .F. ) ;
#65314 = CARTESIAN_POINT ( 'NONE',  ( -54.63855600440099636, -24.15620529776628089, 10.23563542870661180 ) ) ;
#65315 = CARTESIAN_POINT ( 'NONE',  ( 12.01435098137705637, -16.61664908515649941, 11.49999999999998934 ) ) ;
#65316 = VERTEX_POINT ( 'NONE', #82471 ) ;
#65317 = ORIENTED_EDGE ( 'NONE', *, *, #51037, .T. ) ;
#65318 = AXIS2_PLACEMENT_3D ( 'NONE', #76506, #46086, #85634 ) ;
#65319 = EDGE_LOOP ( 'NONE', ( #6846, #94731, #10792, #11717 ) ) ;
#65320 = CARTESIAN_POINT ( 'NONE',  ( -80.60591430188112838, -25.13389835371019032, 7.097322268695329228 ) ) ;
#65321 = CARTESIAN_POINT ( 'NONE',  ( 5.194767643164344584, 22.50260600399833422, 11.49999999999998934 ) ) ;
#65322 = DIRECTION ( 'NONE',  ( 0.000000000000000000, -0.000000000000000000, -1.000000000000000000 ) ) ;
#65323 = B_SPLINE_CURVE_WITH_KNOTS ( 'NONE', 3,
 ( #22866, #84783, #6163, #53353, #53851, #37115, #43742, #76655, #98503, #99000, #59971, #74676, #29494, #90407, #60477, #91393, #83783, #21870 ),
 .UNSPECIFIED., .F., .F.,
 ( 4, 2, 2, 2, 2, 2, 2, 2, 4 ),
 ( 0.000000000000000000, 0.1250000000000001388, 0.1875000000000000278, 0.2499999999999999445, 0.5000000000000001110, 0.7500000000000002220, 0.8125000000000001110, 0.8750000000000000000, 1.000000000000000000 ),
 .UNSPECIFIED. ) ;
#65324 = CARTESIAN_POINT ( 'NONE',  ( -20.15914900662387055, -2.930279687489938389, -1.500000000000002220 ) ) ;
#65325 = ORIENTED_EDGE ( 'NONE', *, *, #1322, .F. ) ;
#65326 = CARTESIAN_POINT ( 'NONE',  ( -29.67004714597209869, -23.41239500526456041, 11.44779303447556984 ) ) ;
#65327 = ADVANCED_FACE ( 'NONE', ( #67267 ), #98690, .T. ) ;
#65328 = CARTESIAN_POINT ( 'NONE',  ( -105.5608691116280511, -23.48783264082477018, -1.443836473390094355 ) ) ;
#65329 = CARTESIAN_POINT ( 'NONE',  ( -57.58953762381671737, -23.48783264082478794, -1.443836473390068820 ) ) ;
#65330 = ORIENTED_EDGE ( 'NONE', *, *, #4350, .T. ) ;
#65331 = CARTESIAN_POINT ( 'NONE',  ( -27.68651082257922980, -25.21531658275831589, 2.274902402383796041 ) ) ;
#65332 = CARTESIAN_POINT ( 'NONE',  ( -93.52287095715006160, -24.64965694238407323, 8.947790433994196491 ) ) ;
#65333 = ORIENTED_EDGE ( 'NONE', *, *, #97653, .F. ) ;
#65334 = CARTESIAN_POINT ( 'NONE',  ( -15.76495264167062160, -13.51897010167481739, -1.500000000000002220 ) ) ;
#65335 = ADVANCED_FACE ( 'NONE', ( #90092 ), #28817, .T. ) ;
#65336 = ORIENTED_EDGE ( 'NONE', *, *, #65845, .F. ) ;
#65338 = ORIENTED_EDGE ( 'NONE', *, *, #25021, .F. ) ;
#65337 = CARTESIAN_POINT ( 'NONE',  ( 30.09341516180546350, 4.772774720514425972, -11.39311774897855756 ) ) ;
#65339 = CIRCLE ( 'NONE', #57217, 2.000000000000000000 ) ;
#65340 = B_SPLINE_SURFACE_WITH_KNOTS ( 'NONE', 3, 1, ( 
 ( #55264, #62886 ),
 ( #16679, #25798 ),
 ( #86195, #9071 ),
 ( #56272, #85699 ),
 ( #47146, #78064 ),
 ( #1974, #94300 ),
 ( #47649, #24787 ),
 ( #8578, #48659 ),
 ( #39525, #17684 ),
 ( #55767, #79074 ),
 ( #9571, #71486 ),
 ( #22598, #92128 ),
 ( #83516, #68803 ),
 ( #23602, #38842 ),
 ( #69297, #77888 ) ),
 .UNSPECIFIED., .F., .F., .F.,
 ( 4, 1, 1, 1, 1, 1, 1, 1, 1, 1, 1, 1, 4 ),
 ( 2, 2 ),
 ( 0.000000000000000000, 0.07405842627338315998, 0.1488703523168777021, 0.2266676683691784822, 0.3077347594511126161, 0.3911572038059789591, 0.4739293555425539428, 0.5579277515150540268, 0.6449892900513599647, 0.7333640555176174081, 0.8210920421841580996, 0.9092872149973385554, 1.000000000000000000 ),
 ( 0.000000000000000000, 1.000000000000000000 ),
 .UNSPECIFIED. ) ;
#65341 = CARTESIAN_POINT ( 'NONE',  ( -77.52287095715006160, -24.50216790748205042, 0.6166512839542531710 ) ) ;
#65342 = CARTESIAN_POINT ( 'NONE',  ( -107.6228709571500701, -23.47593901973091235, -1.443836447538999312 ) ) ;
#65343 = ORIENTED_EDGE ( 'NONE', *, *, #3223, .T. ) ;
#65344 = VERTEX_POINT ( 'NONE', #66782 ) ;
#65345 = CARTESIAN_POINT ( 'NONE',  ( -78.62287095715004170, -24.65952944569304606, 1.056160979905698349 ) ) ;
#65346 = CARTESIAN_POINT ( 'NONE',  ( -116.6228709571501270, -24.35013146730204525, 9.818937971375104823 ) ) ;
#65348 = ADVANCED_FACE ( 'NONE', ( #43919, #51038 ), #44427, .T. ) ;
#65347 = CARTESIAN_POINT ( 'NONE',  ( -71.10442080388585850, -25.24515113135309718, 5.639839579979339490 ) ) ;
#65350 = ORIENTED_EDGE ( 'NONE', *, *, #18957, .F. ) ;
#65349 = CARTESIAN_POINT ( 'NONE',  ( -9.261969182712835646, 20.05037652441878038, 11.49999999999999645 ) ) ;
#65351 = DIRECTION ( 'NONE',  ( 1.000000000000000000, 0.000000000000000000, 0.000000000000000000 ) ) ;
#65352 = CARTESIAN_POINT ( 'NONE',  ( 18.79633983808273712, -12.56333175589740847, -1.500000000000002220 ) ) ;
#65354 = ORIENTED_EDGE ( 'NONE', *, *, #35263, .F. ) ;
#65353 = DIRECTION ( 'NONE',  ( 3.773278334444167608E-23, -1.000000000000000000, 0.000000000000000000 ) ) ;
#65355 = CIRCLE ( 'NONE', #28084, 28.96799999999999642 ) ;
#65356 = ORIENTED_EDGE ( 'NONE', *, *, #60128, .F. ) ;
#65357 = LINE ( 'NONE', #87157, #23943 ) ;
#65358 = LINE ( 'NONE', #80547, #55452 ) ;
#65359 = ORIENTED_EDGE ( 'NONE', *, *, #10623, .T. ) ;
#65360 = CARTESIAN_POINT ( 'NONE',  ( -19.38594737788604405, 8.525550480899875438, 11.49999999999998934 ) ) ;
#65361 = CARTESIAN_POINT ( 'NONE',  ( -125.6228709571500559, -24.62226745350437795, 0.9660975649728152925 ) ) ;
#65362 = CARTESIAN_POINT ( 'NONE',  ( -40.58094919657983723, -25.29362508255670150, 5.541655676671355835 ) ) ;
#65363 = CARTESIAN_POINT ( 'NONE',  ( 10.78255534502030777, 19.45608938089507234, -1.500000000000002220 ) ) ;
#65364 = LINE ( 'NONE', #64868, #25715 ) ;
#65365 = EDGE_LOOP ( 'NONE', ( #26742, #51276, #29063, #57583 ) ) ;
#65366 = LINE ( 'NONE', #33887, #88681 ) ;
#65367 = CARTESIAN_POINT ( 'NONE',  ( -4.141025641025642301, -6.376774720514408301, 19.19230769230769695 ) ) ;
#65368 = CARTESIAN_POINT ( 'NONE',  ( -36.66656757783551512, -23.48786465467240347, 11.44779295918255180 ) ) ;
#65369 = LINE ( 'NONE', #73456, #3202 ) ;
#65370 = VECTOR ( 'NONE', #34050, 1000.000000000000000 ) ;
#65371 = CARTESIAN_POINT ( 'NONE',  ( -16.58133674543539371, -10.29093563426468450, 11.49999999999998934 ) ) ;
#65372 = ORGANIZATION ( 'NAUO-ORG8', 'UNSPECIFIED', 'UNSPECIFIED' ) ;
#65373 = CARTESIAN_POINT ( 'NONE',  ( 21.23773461148298836, -3.020459416520930862, -1.500000000000002220 ) ) ;
#65374 = CARTESIAN_POINT ( 'NONE',  ( -26.47871760004291630, -24.57999593927708304, 2.074685142752674238 ) ) ;
#65375 = CARTESIAN_POINT ( 'NONE',  ( 7.150000000000004796, -2.000000000000001776, 19.19609335255483984 ) ) ;
#65376 = CARTESIAN_POINT ( 'NONE',  ( -77.50432408278001617, -24.34968618360934300, 0.1864209137778811143 ) ) ;
#65377 = CARTESIAN_POINT ( 'NONE',  ( 22.46337926046256328, 3.617889471270266277, -1.500000000000002220 ) ) ;
#65378 = VECTOR ( 'NONE', #74712, 1000.000000000000000 ) ;
#65379 = EDGE_CURVE ( 'NONE', #50584, #82905, #83142, .T. ) ;
#65380 = CARTESIAN_POINT ( 'NONE',  ( -98.62355863167962866, -24.65952944569305316, 1.056160979905700570 ) ) ;
#65381 = CARTESIAN_POINT ( 'NONE',  ( -128.5228709571500758, -23.47593901973090524, -1.443836447538996204 ) ) ;
#65382 = CARTESIAN_POINT ( 'NONE',  ( -8.676013072486071565, -17.92234406281952275, 11.49999999999999645 ) ) ;
#65383 = CARTESIAN_POINT ( 'NONE',  ( -101.6228709571500559, -23.48786465467242479, 11.44779295918254114 ) ) ;
#65384 = ADVANCED_FACE ( 'NONE', ( #90585 ), #29185, .T. ) ;
#65385 = VECTOR ( 'NONE', #84416, 1000.000000000000000 ) ;
#65386 = ADVANCED_FACE ( 'NONE', ( #28692 ), #98480, .F. ) ;
#65387 = CARTESIAN_POINT ( 'NONE',  ( -39.60068811824800150, -23.96169478059713143, 10.65365249895718769 ) ) ;
#65388 = B_SPLINE_CURVE_WITH_KNOTS ( 'NONE', 3,
 ( #81159, #73551, #33480, #4043 ),
 .UNSPECIFIED., .F., .F.,
 ( 4, 4 ),
 ( 0.000000000000000000, 1.000000000000000000 ),
 .UNSPECIFIED. ) ;
#65389 = CARTESIAN_POINT ( 'NONE',  ( -48.53564735683374209, -24.51314013834315375, 0.6176544820404137326 ) ) ;
#65390 = ORIENTED_EDGE ( 'NONE', *, *, #88971, .F. ) ;
#65391 = CARTESIAN_POINT ( 'NONE',  ( 29.73828978136054602, 4.772774720514425972, -4.021765098496561386 ) ) ;
#65392 = CARTESIAN_POINT ( 'NONE',  ( -77.52287095715004739, -23.73907113216989728, -1.053371485793253903 ) ) ;
#65393 = EDGE_CURVE ( 'NONE', #34332, #8750, #16954, .T. ) ;
#65394 = CARTESIAN_POINT ( 'NONE',  ( 21.69746526873944958, -0.4026533170205861545, -1.500000000000002220 ) ) ;
#65395 = CARTESIAN_POINT ( 'NONE',  ( -51.76873150024551506, -25.17952130149804191, 6.819150868768721452 ) ) ;
#65396 = CARTESIAN_POINT ( 'NONE',  ( -13.92019785312828972, -13.74635529968554515, -1.500000000000002220 ) ) ;
#65397 = EDGE_CURVE ( 'NONE', #21, #85607, #62144, .T. ) ;
#65398 = DIRECTION ( 'NONE',  ( 0.000000000000000000, -1.000000000000000000, 0.000000000000000000 ) ) ;
#65399 = ORIENTED_EDGE ( 'NONE', *, *, #45299, .F. ) ;
#65400 = CALENDAR_DATE ( 2026, 9, 10 ) ;
#65401 = CARTESIAN_POINT ( 'NONE',  ( 18.72495633783376334, 0.000000000000000000, 2.346898003627108320 ) ) ;
#65402 = CARTESIAN_POINT ( 'NONE',  ( -19.81292649638395531, 4.959676026661640869, 11.49999999999999645 ) ) ;
#65403 = CARTESIAN_POINT ( 'NONE',  ( -41.62287095715006302, -29.50250243563736774, 8.947779886222148704 ) ) ;
#65404 = CARTESIAN_POINT ( 'NONE',  ( -60.24005924445285842, -25.32056586294729783, 4.734103931585309510 ) ) ;
#65405 = VERTEX_POINT ( 'NONE', #24560 ) ;
#65406 = DIRECTION ( 'NONE',  ( -0.000000000000000000, 0.000000000000000000, -1.000000000000000000 ) ) ;
#65407 = FACE_OUTER_BOUND ( 'NONE', #82975, .T. ) ;
#65408 = CARTESIAN_POINT ( 'NONE',  ( -125.5895376238167245, -23.48786465467241769, 11.44779295918253403 ) ) ;
#65409 =( BOUNDED_SURFACE ( )  B_SPLINE_SURFACE ( 3, 1, ( 
 ( #27498, #67069 ),
 ( #65581, #80783 ),
 ( #57461, #87891 ),
 ( #12245, #74164 ) ),
 .UNSPECIFIED., .F., .F., .T. ) 
 B_SPLINE_SURFACE_WITH_KNOTS ( ( 4, 4 ),
 ( 2, 2 ),
 ( 0.000000000000000000, 1.000000000000000000 ),
 ( 0.000000000000000000, 1.000000000000000000 ),
 .UNSPECIFIED. ) 
 GEOMETRIC_REPRESENTATION_ITEM ( )  RATIONAL_B_SPLINE_SURFACE ( (
 ( 1.000000000000000000, 1.000000000000000000),
 ( 0.3333333333333333703, 0.3333333333333333703),
 ( 0.3333333333333333703, 0.3333333333333333703),
 ( 1.000000000000000000, 1.000000000000000000) ) ) 
 REPRESENTATION_ITEM ( '' )  SURFACE ( )  );
#65410 = B_SPLINE_CURVE_WITH_KNOTS ( 'NONE', 3,
 ( #63665, #94587, #79357, #25068 ),
 .UNSPECIFIED., .F., .F.,
 ( 4, 4 ),
 ( 5.511242692161060920E-09, 0.0003958033267307038716 ),
 .UNSPECIFIED. ) ;
#65411 = CARTESIAN_POINT ( 'NONE',  ( -11.64875734969026233, 5.965225279485572685, 30.51402280011862089 ) ) ;
#65412 = VECTOR ( 'NONE', #24498, 1000.000000000000000 ) ;
#65413 = ORIENTED_EDGE ( 'NONE', *, *, #34721, .T. ) ;
#65414 = CARTESIAN_POINT ( 'NONE',  ( -128.5228709571500758, -29.50250243563736774, 8.947779886222132717 ) ) ;
#65415 = CARTESIAN_POINT ( 'NONE',  ( -20.69623851537618364, -9.862649113751288610, 11.49999999999999645 ) ) ;
#65416 = CARTESIAN_POINT ( 'NONE',  ( 10.97283692364161922, -19.94330716608196852, 11.49999999999998934 ) ) ;
#65417 = CARTESIAN_POINT ( 'NONE',  ( -70.52865987952087323, -25.04472902735052031, 7.555535287402955547 ) ) ;
#65418 = VECTOR ( 'NONE', #14655, 1000.000000000000114 ) ;
#65419 = LINE ( 'NONE', #34441, #52829 ) ;
#65420 = CARTESIAN_POINT ( 'NONE',  ( -90.56379385379925395, -23.48783264082477018, -1.443836473390091690 ) ) ;
#65421 = CARTESIAN_POINT ( 'NONE',  ( -9.278253834636473130, -5.876774720514426953, 18.21871304725684482 ) ) ;
#65422 = CARTESIAN_POINT ( 'NONE',  ( -89.52287095715003318, -23.48783264083374789, -1.443836473376144180 ) ) ;
#65423 = CARTESIAN_POINT ( 'NONE',  ( 11.25260618158950621, 18.78031238747207610, -1.500000000000002220 ) ) ;
#65424 = LINE ( 'NONE', #58291, #41395 ) ;
#65425 = CARTESIAN_POINT ( 'NONE',  ( -10.21384395349174490, 6.376774720514426953, 29.49402280011861777 ) ) ;
#65426 = DIRECTION ( 'NONE',  ( 0.000000000000000000, -1.000000000000000000, 0.000000000000000000 ) ) ;
#65427 = CARTESIAN_POINT ( 'NONE',  ( -58.54270549319968353, -24.34968618360933945, 0.1864209137778795045 ) ) ;
#65428 = VERTEX_POINT ( 'NONE', #93069 ) ;
#65429 = CARTESIAN_POINT ( 'NONE',  ( -12.12210191164509965, 16.44476101713275185, 11.49999999999998934 ) ) ;
#65430 = ORIENTED_EDGE ( 'NONE', *, *, #5837, .F. ) ;
#65431 = ORIENTED_EDGE ( 'NONE', *, *, #6161, .F. ) ;
#65432 = ORIENTED_EDGE ( 'NONE', *, *, #96458, .F. ) ;
#65433 = CARTESIAN_POINT ( 'NONE',  ( -14.43837761634077310, -17.93274050997184332, 11.49999999999998934 ) ) ;
#65434 = DIRECTION ( 'NONE',  ( 0.000000000000000000, 1.000000000000000000, 0.000000000000000000 ) ) ;
#65435 = CARTESIAN_POINT ( 'NONE',  ( -20.16912494768211417, -0.3064379698199363733, -1.500000000000002220 ) ) ;
#65436 = VERTEX_POINT ( 'NONE', #78836 ) ;
#65437 = CARTESIAN_POINT ( 'NONE',  ( -67.62287095715005592, -23.48786465467241058, 11.44779295918254647 ) ) ;
#65438 = CARTESIAN_POINT ( 'NONE',  ( 0.000000000000000000, -1.530000000000000027, -0.3850000000000000089 ) ) ;
#65439 = CARTESIAN_POINT ( 'NONE',  ( -95.50652094920334889, -24.63355581998386157, 0.9682620441943944334 ) ) ;
#65440 = DIRECTION ( 'NONE',  ( -0.9496245541219264785, 6.845827386180410961E-16, -0.3133898629642195011 ) ) ;
#65442 = EDGE_LOOP ( 'NONE', ( #98988, #98012, #24315 ) ) ;
#65441 = CARTESIAN_POINT ( 'NONE',  ( -19.64189229742525455, -8.423329616690555355, 11.49999999999999645 ) ) ;
#65443 = CARTESIAN_POINT ( 'NONE',  ( 7.166666666666668739, -5.876774720514419847, 20.78665865384614975 ) ) ;
#65444 = ORIENTED_EDGE ( 'NONE', *, *, #60394, .T. ) ;
#65445 = CARTESIAN_POINT ( 'NONE',  ( 22.02009960291501045, 3.200778107580485532, 11.49999999999998934 ) ) ;
#65446 = CARTESIAN_POINT ( 'NONE',  ( -18.79711486612840332, 8.613068827758688428, 11.49999999999998934 ) ) ;
#65447 = EDGE_CURVE ( 'NONE', #40883, #95766, #727, .T. ) ;
#65448 = ORIENTED_EDGE ( 'NONE', *, *, #31209, .T. ) ;
#65449 = ADVANCED_FACE ( 'NONE', ( #39290 ), #23550, .T. ) ;
#65450 = CARTESIAN_POINT ( 'NONE',  ( -8.978253834636468866, -5.876774720514426953, 18.51871304725684553 ) ) ;
#65451 = VERTEX_POINT ( 'NONE', #54036 ) ;
#65452 = DIRECTION ( 'NONE',  ( -1.084136044942898696E-16, -0.000000000000000000, 1.000000000000000000 ) ) ;
#65453 = ORIENTED_EDGE ( 'NONE', *, *, #96315, .T. ) ;
#65454 = AXIS2_PLACEMENT_3D ( 'NONE', #74822, #66249, #44896 ) ;
#65455 = CARTESIAN_POINT ( 'NONE',  ( -50.32469610480872291, -25.27517877801826884, 2.834264043007450162 ) ) ;
#65456 = CARTESIAN_POINT ( 'NONE',  ( -7.180602670292889123, -19.69607742855361465, -1.500000000000002220 ) ) ;
#65457 = CARTESIAN_POINT ( 'NONE',  ( -15.13543854793762300, 15.80457324685279374, 11.49999999999999645 ) ) ;
#65458 = CARTESIAN_POINT ( 'NONE',  ( -26.43901205547898670, -24.77993617750158606, 6.777242332140119174 ) ) ;
#65459 = CARTESIAN_POINT ( 'NONE',  ( 8.356338879324495039, -20.90460381316865934, 11.49999999999998934 ) ) ;
#65460 = B_SPLINE_CURVE_WITH_KNOTS ( 'NONE', 3,
 ( #5352, #52032, #45419, #61152 ),
 .UNSPECIFIED., .F., .F.,
 ( 4, 4 ),
 ( 0.000000000000000000, 9.999999999999592548E-05 ),
 .UNSPECIFIED. ) ;
#65461 = CARTESIAN_POINT ( 'NONE',  ( 0.8316226063609513108, 20.92010288561657205, -1.500000000000002220 ) ) ;
#65462 = DIRECTION ( 'NONE',  ( 2.504262461560503484E-15, -6.886721769291384876E-15, 1.000000000000000000 ) ) ;
#65463 = CARTESIAN_POINT ( 'NONE',  ( 5.930937628982182908, -5.876774720514417183, 20.24478033514397524 ) ) ;
#65464 = CARTESIAN_POINT ( 'NONE',  ( -9.383883476483159569, 17.86611652351680846, 0.000000000000000000 ) ) ;
#65465 = CARTESIAN_POINT ( 'NONE',  ( -70.62287095715007013, -23.47596703998600631, 11.44779298504227505 ) ) ;
#65466 = ORIENTED_EDGE ( 'NONE', *, *, #72142, .T. ) ;
#65467 = ORIENTED_EDGE ( 'NONE', *, *, #73811, .F. ) ;
#65468 = ORIENTED_EDGE ( 'NONE', *, *, #13711, .F. ) ;
#65469 = FACE_OUTER_BOUND ( 'NONE', #42055, .T. ) ;
#65470 = ORIENTED_EDGE ( 'NONE', *, *, #38995, .T. ) ;
#65471 = CARTESIAN_POINT ( 'NONE',  ( 10.13398631766115443, 18.95262098133242290, -1.500000000000002220 ) ) ;
#65472 = ORIENTED_EDGE ( 'NONE', *, *, #100331, .F. ) ;
#65473 = CARTESIAN_POINT ( 'NONE',  ( -41.32836283488544638, 2.682774720514426559, 39.26872235229541985 ) ) ;
#65474 = CARTESIAN_POINT ( 'NONE',  ( 14.35337761433406811, 15.45585641580067104, -1.500000000000002220 ) ) ;
#65475 = CARTESIAN_POINT ( 'NONE',  ( -52.62287095715007013, -24.33927499327854704, 9.819080762295820719 ) ) ;
#65476 = FACE_OUTER_BOUND ( 'NONE', #38366, .T. ) ;
#65477 = DIRECTION ( 'NONE',  ( 2.417950247244706201E-16, -8.673617379884035472E-16, -1.000000000000000000 ) ) ;
#65478 = PLANE ( 'NONE',  #96143 ) ;
#65479 = CARTESIAN_POINT ( 'NONE',  ( -129.5218485930514873, -24.51419770103158413, 9.386484678747176957 ) ) ;
#65480 = CARTESIAN_POINT ( 'NONE',  ( 14.91618686576236108, -16.25093855066790738, -1.500000000000002220 ) ) ;
#65481 = VERTEX_POINT ( 'NONE', #47415 ) ;
#65482 = CARTESIAN_POINT ( 'NONE',  ( -116.5175178794913649, -24.34968618360935366, 0.1864209137779019587 ) ) ;
#65483 = AXIS2_PLACEMENT_3D ( 'NONE', #65052, #33574, #57432 ) ;
#65484 = CARTESIAN_POINT ( 'NONE',  ( -111.6228709571500701, -23.96177878511308634, 10.65340807706329862 ) ) ;
#65485 = CARTESIAN_POINT ( 'NONE',  ( -78.62287095715005592, -23.73934037231757799, 11.05740245334328442 ) ) ;
#65486 = EDGE_CURVE ( 'NONE', #88521, #27856, #14948, .T. ) ;
#65487 = CARTESIAN_POINT ( 'NONE',  ( -62.53524634668898585, -24.66019654487199730, 8.947790411086124607 ) ) ;
#65488 = AXIS2_PLACEMENT_3D ( 'NONE', #68907, #53197, #46082 ) ;
#65489 = CARTESIAN_POINT ( 'NONE',  ( -121.6228709571500417, -29.50250243563736774, 8.947779886222134493 ) ) ;
#65490 = DIRECTION ( 'NONE',  ( 0.8246584009594636333, -1.974890369949422146E-15, 0.5656310827093757876 ) ) ;
#65491 = CARTESIAN_POINT ( 'NONE',  ( -5.188002292566340934, -20.72503599944539587, -1.500000000000002220 ) ) ;
#65492 = CARTESIAN_POINT ( 'NONE',  ( -81.52287095715010423, -23.47593901973090524, -1.443836447538996648 ) ) ;
#65493 = CARTESIAN_POINT ( 'NONE',  ( -48.85554520786481447, -25.25978491487771649, 3.590542621692356384 ) ) ;
#65494 = CARTESIAN_POINT ( 'NONE',  ( 30.53060340732035982, 1.477225279485574028, 19.84760796525321425 ) ) ;
#65495 = FACE_OUTER_BOUND ( 'NONE', #59523, .T. ) ;
#65496 = CARTESIAN_POINT ( 'NONE',  ( 22.48748499206561746, 2.281147167042596013, -1.500000000000002220 ) ) ;
#65497 = LINE ( 'NONE', #96419, #40972 ) ;
#65498 = ORIENTED_EDGE ( 'NONE', *, *, #94038, .T. ) ;
#65499 = CARTESIAN_POINT ( 'NONE',  ( 4.612744205187371271, -5.876774720514418959, 20.61169588237105188 ) ) ;
#65500 = CARTESIAN_POINT ( 'NONE',  ( -79.49885629545516963, -24.65952944569304606, 1.056160979905700126 ) ) ;
#65501 = CARTESIAN_POINT ( 'NONE',  ( -14.12090166725071327, 13.77431136191591143, 11.49999999999999645 ) ) ;
#65502 = CARTESIAN_POINT ( 'NONE',  ( -82.62287095715007013, -24.50321055353805377, 9.387540953477531147 ) ) ;
#65503 = ADVANCED_FACE ( 'NONE', ( #78342 ), #55537, .F. ) ;
#65504 = CARTESIAN_POINT ( 'NONE',  ( -104.6228709571500559, -29.50250243563736774, 8.947779886222138046 ) ) ;
#65505 = ORIENTED_EDGE ( 'NONE', *, *, #64466, .F. ) ;
#65506 = CARTESIAN_POINT ( 'NONE',  ( 8.573524122111766843, -5.965225279485574461, -28.10203366675327175 ) ) ;
#65507 = CARTESIAN_POINT ( 'NONE',  ( -29.81116077451118329, -25.26026984619284121, 4.841835660607406666 ) ) ;
#65508 = EDGE_CURVE ( 'NONE', #68549, #89130, #77340, .T. ) ;
#65509 = CARTESIAN_POINT ( 'NONE',  ( -47.52287095715006160, -29.50248528299804818, 1.056150453629033370 ) ) ;
#65510 = CARTESIAN_POINT ( 'NONE',  ( -21.01067979154616694, 5.129389437380057259, -1.500000000000002220 ) ) ;
#65511 = CARTESIAN_POINT ( 'NONE',  ( -126.6228709571500559, -24.64965695001469825, 8.947790433994173398 ) ) ;
#65512 = CARTESIAN_POINT ( 'NONE',  ( -2.960655606634402748, -19.13016773636607581, -1.500000000000002220 ) ) ;
#65513 = ADVANCED_FACE ( 'NONE', ( #84961 ), #8844, .F. ) ;
#65514 = CARTESIAN_POINT ( 'NONE',  ( -10.37843575862113887, -5.356774720514428267, 27.71903885537846435 ) ) ;
#65515 = CARTESIAN_POINT ( 'NONE',  ( -118.5228709571500758, -24.64965694238408034, 8.947790433994191162 ) ) ;
#65516 = CARTESIAN_POINT ( 'NONE',  ( 6.953341435731974940, 18.52374150113109152, -1.500000000000002220 ) ) ;
#65517 = ORIENTED_EDGE ( 'NONE', *, *, #53006, .T. ) ;
#65518 = EDGE_CURVE ( 'NONE', #28958, #18679, #70750, .T. ) ;
#65519 = CARTESIAN_POINT ( 'NONE',  ( 13.55758662847591900, -15.04642845256218031, 11.49999999999999645 ) ) ;
#65520 = CARTESIAN_POINT ( 'NONE',  ( 5.730633878096764278, -5.876774720514418959, 20.45679216967608838 ) ) ;
#65521 = EDGE_CURVE ( 'NONE', #91571, #54552, #40300, .T. ) ;
#65522 = VERTEX_POINT ( 'NONE', #70246 ) ;
#65523 = CARTESIAN_POINT ( 'NONE',  ( -67.52287095715009002, -24.35013146730203815, 9.818937971375095941 ) ) ;
#65524 = FACE_OUTER_BOUND ( 'NONE', #74517, .T. ) ;
#65525 = DIRECTION ( 'NONE',  ( 0.000000000000000000, 0.000000000000000000, 1.000000000000000000 ) ) ;
#65526 = CARTESIAN_POINT ( 'NONE',  ( -69.55126625704997423, -25.15208592601422311, 3.076695591939294427 ) ) ;
#65527 = CARTESIAN_POINT ( 'NONE',  ( -44.52287095715006160, -24.64965694238575011, 8.947790433994205372 ) ) ;
#65528 = CARTESIAN_POINT ( 'NONE',  ( -71.62287095715005592, -23.94994826722565762, -0.6494450866342720285 ) ) ;
#65529 = CARTESIAN_POINT ( 'NONE',  ( -10.14125802585430947, 17.27231531754821603, -1.500000000000002220 ) ) ;
#65530 = ADVANCED_FACE ( 'NONE', ( #62647 ), #46408, .T. ) ;
#65531 = DIRECTION ( 'NONE',  ( 0.000000000000000000, -0.000000000000000000, 1.000000000000000000 ) ) ;
#65532 = ORIENTED_EDGE ( 'NONE', *, *, #76562, .T. ) ;
#65533 = CARTESIAN_POINT ( 'NONE',  ( -90.58953762381672448, -23.47596703998600631, 11.44779298504227683 ) ) ;
#65534 = DIRECTION ( 'NONE',  ( 0.000000000000000000, -0.9999999999976377785, -2.173523156925979128E-06 ) ) ;
#65535 = DIRECTION ( 'NONE',  ( -3.773278334453079030E-23, 0.9999999999976377785, 2.173523156925979128E-06 ) ) ;
#65536 = B_SPLINE_CURVE_WITH_KNOTS ( 'NONE', 3,
 ( #82254, #61930, #67546, #59939, #6629, #22831 ),
 .UNSPECIFIED., .F., .F.,
 ( 4, 2, 4 ),
 ( 0.000000000000000000, 0.001380901958385382473, 0.002761803916770764946 ),
 .UNSPECIFIED. ) ;
#65537 = DIRECTION ( 'NONE',  ( 0.000000000000000000, 2.173523156925980399E-06, -0.9999999999976378895 ) ) ;
#65538 = CARTESIAN_POINT ( 'NONE',  ( -45.52287095715006160, -25.00158670708908915, 2.256160236439166411 ) ) ;
#65539 = VECTOR ( 'NONE', #48277, 1000.000000000000114 ) ;
#65540 = CARTESIAN_POINT ( 'NONE',  ( 14.43441819134413073, 3.316774720514428232, -28.36222020317436687 ) ) ;
#65541 = CARTESIAN_POINT ( 'NONE',  ( -49.26828308126997769, -25.12100811749006724, 7.112893600995336740 ) ) ;
#65542 = ORIENTED_EDGE ( 'NONE', *, *, #75476, .F. ) ;
#65543 = CARTESIAN_POINT ( 'NONE',  ( 5.487062353440709472, 19.58251264919930534, 11.49999999999998934 ) ) ;
#65544 = EDGE_LOOP ( 'NONE', ( #45500, #30170, #6739, #1704 ) ) ;
#65545 = EDGE_CURVE ( 'NONE', #32090, #40087, #32176, .T. ) ;
#65546 = CARTESIAN_POINT ( 'NONE',  ( -22.92702450682246251, 0.3551139841105944162, 11.49999999999998934 ) ) ;
#65547 = CARTESIAN_POINT ( 'NONE',  ( 31.65781406150966149, 5.771867554241929987, 28.25297929084410242 ) ) ;
#65548 = AXIS2_PLACEMENT_3D ( 'NONE', #72914, #11496, #59183 ) ;
#65549 = VERTEX_POINT ( 'NONE', #61155 ) ;
#65550 = CARTESIAN_POINT ( 'NONE',  ( -96.52287095715006160, -29.50250243563736774, 8.947779886222138046 ) ) ;
#65552 = EDGE_CURVE ( 'NONE', #72410, #94726, #92842, .T. ) ;
#65551 = CARTESIAN_POINT ( 'NONE',  ( 14.61581676223891613, 3.316774720514426900, -27.35847991879931485 ) ) ;
#65553 = B_SPLINE_CURVE_WITH_KNOTS ( 'NONE', 3,
 ( #44877, #75799, #73813, #74803, #37257, #29633 ),
 .UNSPECIFIED., .F., .F.,
 ( 4, 2, 4 ),
 ( 0.000000000000000000, 0.001380764517854760846, 0.002761529035709521691 ),
 .UNSPECIFIED. ) ;
#65554 = DIRECTION ( 'NONE',  ( 0.09721092304694051167, 0.000000000000000000, -0.9952638024365005887 ) ) ;
#65555 = CARTESIAN_POINT ( 'NONE',  ( -6.524719417830534773, 20.15472526627327454, 11.49999999999999645 ) ) ;
#65556 = CARTESIAN_POINT ( 'NONE',  ( 17.13038851031509680, -14.05419017248541813, 11.49999999999998934 ) ) ;
#65557 = ADVANCED_FACE ( 'NONE', ( #86964 ), #41815, .T. ) ;
#65558 = CARTESIAN_POINT ( 'NONE',  ( 15.34425395324244867, 13.73259486114767114, -1.500000000000002220 ) ) ;
#65559 = ORIENTED_EDGE ( 'NONE', *, *, #29385, .F. ) ;
#65560 = CARTESIAN_POINT ( 'NONE',  ( -41.56943525746097379, -23.48783264082477729, -1.443836473390076147 ) ) ;
#65561 = ORIENTED_EDGE ( 'NONE', *, *, #35493, .T. ) ;
#65562 = CARTESIAN_POINT ( 'NONE',  ( -54.63855744824223137, -24.15543982623906416, -0.2315651400026691176 ) ) ;
#65563 = EDGE_CURVE ( 'NONE', #11608, #35597, #35453, .T. ) ;
#65564 = CARTESIAN_POINT ( 'NONE',  ( -50.52287095715006160, -24.82576562948880294, 8.398263436605674315 ) ) ;
#65565 = EDGE_LOOP ( 'NONE', ( #77657, #7379, #21447, #89390 ) ) ;
#65566 = ORIENTED_EDGE ( 'NONE', *, *, #72810, .F. ) ;
#65567 = ORIENTED_EDGE ( 'NONE', *, *, #43964, .F. ) ;
#65568 = CARTESIAN_POINT ( 'NONE',  ( -116.6228709571500417, -23.95044443724992433, 10.65354141964649237 ) ) ;
#65569 = FACE_OUTER_BOUND ( 'NONE', #42603, .T. ) ;
#65570 = DIRECTION ( 'NONE',  ( -3.773278334453080206E-23, 0.9999999999976377785, 2.173523156925979975E-06 ) ) ;
#65571 = CARTESIAN_POINT ( 'NONE',  ( 17.59156710592704442, 10.99281682905060897, -1.500000000000002220 ) ) ;
#65572 = CARTESIAN_POINT ( 'NONE',  ( 2.995010171738120786, 21.53247193037183038, 11.49999999999999645 ) ) ;
#65573 = ORIENTED_EDGE ( 'NONE', *, *, #63923, .T. ) ;
#65574 = CARTESIAN_POINT ( 'NONE',  ( -62.62287095715004881, -24.65952944569304606, 1.056160979905693909 ) ) ;
#65575 = CARTESIAN_POINT ( 'NONE',  ( -37.52287095715006870, -24.65952944569304250, 1.056160979905691910 ) ) ;
#65576 = CARTESIAN_POINT ( 'NONE',  ( 12.67250375155129127, 18.46511205475877304, 11.49999999999998934 ) ) ;
#65577 = CARTESIAN_POINT ( 'NONE',  ( -33.52287095715006160, -24.64965694238574656, 8.947790433994207149 ) ) ;
#65578 = CARTESIAN_POINT ( 'NONE',  ( -23.71328795744024021, -5.965225279485594001, -17.58350715675015152 ) ) ;
#65579 = ORIENTED_EDGE ( 'NONE', *, *, #13785, .F. ) ;
#65580 = CARTESIAN_POINT ( 'NONE',  ( -31.62287095715003815, -24.35013146730203459, 9.818937971375119034 ) ) ;
#65581 = CARTESIAN_POINT ( 'NONE',  ( -119.4728709548940628, -25.40673988423724694, 2.000950539785692150 ) ) ;
#65582 = VECTOR ( 'NONE', #14908, 1000.000000000000114 ) ;
#65583 = VERTEX_POINT ( 'NONE', #88479 ) ;
#65584 = ORIENTED_EDGE ( 'NONE', *, *, #55124, .T. ) ;
#65585 = CARTESIAN_POINT ( 'NONE',  ( -103.6228709571500133, -23.72747288104441665, -1.053458166803660445 ) ) ;
#65586 = CC_DESIGN_PERSON_AND_ORGANIZATION_ASSIGNMENT ( #7693, #54882, ( #19046 ) ) ;
#65587 = ORIENTED_EDGE ( 'NONE', *, *, #98562, .F. ) ;
#65588 = CARTESIAN_POINT ( 'NONE',  ( 21.11169859150035677, 2.410084449224629832, -1.500000000000002220 ) ) ;
#65589 = ORIENTED_EDGE ( 'NONE', *, *, #3527, .F. ) ;
#65590 = CARTESIAN_POINT ( 'NONE',  ( -88.51440607272326133, -23.96119346886880308, -0.6495511937832096905 ) ) ;
#65591 = CARTESIAN_POINT ( 'NONE',  ( 19.20967809413044236, -10.42350525531561978, 11.49999999999998934 ) ) ;
#65592 = PLANE ( 'NONE',  #82168 ) ;
#65593 = CARTESIAN_POINT ( 'NONE',  ( -22.63693132222386950, 1.387278323242118416, 11.49999999999998934 ) ) ;
#65594 = CARTESIAN_POINT ( 'NONE',  ( -40.65892442973913745, -25.28892425236737296, 3.308409971807110050 ) ) ;
#65595 = CARTESIAN_POINT ( 'NONE',  ( -19.77875734969026311, 6.143225279485574397, 27.35402280011862430 ) ) ;
#65596 = CARTESIAN_POINT ( 'NONE',  ( 17.39636294008568740, -13.23181597624684791, -1.500000000000002220 ) ) ;
#65597 = CARTESIAN_POINT ( 'NONE',  ( 6.826756808399247589, -5.876774720514423400, 21.36722843294932161 ) ) ;
#65598 = ORIENTED_EDGE ( 'NONE', *, *, #74789, .T. ) ;
#65599 = CARTESIAN_POINT ( 'NONE',  ( -65.62287095715005592, -24.52232992886362695, 0.6492154411906108091 ) ) ;
#65600 = CARTESIAN_POINT ( 'NONE',  ( -126.6228709571500843, -24.65952944569305316, 1.056160979905707675 ) ) ;
#65601 = ORIENTED_EDGE ( 'NONE', *, *, #45916, .F. ) ;
#65602 = CARTESIAN_POINT ( 'NONE',  ( -90.62287095715004170, -25.00158670708908915, 2.256160236439166411 ) ) ;
#65603 = ORIENTED_EDGE ( 'NONE', *, *, #54722, .F. ) ;
#65604 = CARTESIAN_POINT ( 'NONE',  ( 30.53060340732036693, -5.278445918605220832, 6.049079371708084629 ) ) ;
#65605 = DIRECTION ( 'NONE',  ( 1.000000000000000000, 4.089440751051245812E-15, 0.000000000000000000 ) ) ;
#65606 = CARTESIAN_POINT ( 'NONE',  ( 13.48273455363431772, -16.43370779934446801, -1.500000000000002220 ) ) ;
#65607 = LINE ( 'NONE', #57987, #41771 ) ;
#65608 = CARTESIAN_POINT ( 'NONE',  ( -26.12582186233688830, -24.75186408905701541, 4.293464003132087647 ) ) ;
#65609 = VECTOR ( 'NONE', #92327, 1000.000000000000114 ) ;
#65610 = LINE ( 'NONE', #36131, #16235 ) ;
#65612 = B_SPLINE_CURVE_WITH_KNOTS ( 'NONE', 3,
 ( #54699, #76012, #69914, #37469 ),
 .UNSPECIFIED., .F., .F.,
 ( 4, 4 ),
 ( 1.486098242880303625E-05, 0.002476302731154660791 ),
 .UNSPECIFIED. ) ;
#65611 = DIRECTION ( 'NONE',  ( 3.773278334444167020E-23, -1.000000000000000000, 0.000000000000000000 ) ) ;
#65613 = CARTESIAN_POINT ( 'NONE',  ( -117.5555597079124936, -23.96169478059714564, 10.65365249895717170 ) ) ;
#65614 = ORIENTED_EDGE ( 'NONE', *, *, #94734, .T. ) ;
#65615 = CARTESIAN_POINT ( 'NONE',  ( 15.80261042061247068, 11.49252619723154112, 11.49999999999999645 ) ) ;
#65616 = CARTESIAN_POINT ( 'NONE',  ( -4.968349358974361252, -5.876774720514410077, 19.46153846153847056 ) ) ;
#65617 = EDGE_CURVE ( 'NONE', #6691, #51543, #38400, .T. ) ;
#65618 = LINE ( 'NONE', #74689, #77158 ) ;
#65619 = ORIENTED_EDGE ( 'NONE', *, *, #41828, .F. ) ;
#65620 = CIRCLE ( 'NONE', #20237, 1.149999999999999911 ) ;
#65621 = LINE ( 'NONE', #96538, #14987 ) ;
#65622 = CARTESIAN_POINT ( 'NONE',  ( -99.42228033019944178, -25.31551726817962944, 5.054791656742963823 ) ) ;
#65623 = CARTESIAN_POINT ( 'NONE',  ( -94.52287095715006160, -29.50250243563736774, 8.947779886222139822 ) ) ;
#65624 = DIRECTION ( 'NONE',  ( 0.000000000000000000, 0.000000000000000000, -1.000000000000000000 ) ) ;
#65625 = CARTESIAN_POINT ( 'NONE',  ( -17.62575346185542102, 8.740161020289619387, 11.49999999999998934 ) ) ;
#65626 = ORIENTED_EDGE ( 'NONE', *, *, #45923, .T. ) ;
#65627 = EDGE_CURVE ( 'NONE', #2525, #86407, #841, .T. ) ;
#65628 = DIRECTION ( 'NONE',  ( -3.773278334453079618E-23, 0.9999999999976377785, 2.173523156925979975E-06 ) ) ;
#65629 = CARTESIAN_POINT ( 'NONE',  ( 30.61643171304413613, -3.478988201194511909, 27.37433008668280365 ) ) ;
#65630 = ADVANCED_FACE ( 'NONE', ( #9842 ), #79850, .F. ) ;
#65631 = COORDINATED_UNIVERSAL_TIME_OFFSET ( 0, 0, .AHEAD. ) ;
#65632 = ORIENTED_EDGE ( 'NONE', *, *, #83283, .T. ) ;
#65633 = CARTESIAN_POINT ( 'NONE',  ( -74.52287095715011844, -24.51283580621364422, 0.6167428607019772580 ) ) ;
#65634 = FACE_OUTER_BOUND ( 'NONE', #51985, .T. ) ;
#65635 = CARTESIAN_POINT ( 'NONE',  ( 8.978253834636468866, -5.876774720514426953, 18.51871304725684553 ) ) ;
#65636 = CARTESIAN_POINT ( 'NONE',  ( -97.59978409505167463, -23.48786465467241413, 11.44779295918254469 ) ) ;
#65637 = DIRECTION ( 'NONE',  ( 0.000000000000000000, 1.000000000000000000, -0.000000000000000000 ) ) ;
#65638 = DIRECTION ( 'NONE',  ( 0.000000000000000000, 0.000000000000000000, 1.000000000000000000 ) ) ;
#65639 = CARTESIAN_POINT ( 'NONE',  ( -114.5584140531362607, -23.48786465467241413, 11.44779295918253581 ) ) ;
#65640 = CARTESIAN_POINT ( 'NONE',  ( 15.91301918423788919, -12.03417825965012433, 11.49999999999998934 ) ) ;
#65641 = B_SPLINE_CURVE_WITH_KNOTS ( 'NONE', 3,
 ( #90511, #6271, #92498, #28617 ),
 .UNSPECIFIED., .F., .F.,
 ( 4, 4 ),
 ( 0.000000000000000000, 9.999999999998897304E-05 ),
 .UNSPECIFIED. ) ;
#65642 = EDGE_CURVE ( 'NONE', #81135, #87028, #63656, .T. ) ;
#65643 = CARTESIAN_POINT ( 'NONE',  ( -0.03818598950967933697, -22.55565235769328680, 8.432995269277139272 ) ) ;
#65644 = CARTESIAN_POINT ( 'NONE',  ( 14.98761344906185577, -13.09354923471379983, -1.500000000000002220 ) ) ;
#65645 = VERTEX_POINT ( 'NONE', #71756 ) ;
#65646 = B_SPLINE_CURVE_WITH_KNOTS ( 'NONE', 3,
 ( #6454, #99291, #36405, #51638 ),
 .UNSPECIFIED., .F., .F.,
 ( 4, 4 ),
 ( 0.000000000000000000, 9.999999999999592548E-05 ),
 .UNSPECIFIED. ) ;
#65647 = CARTESIAN_POINT ( 'NONE',  ( 6.660000000000001030, -11.08332949055823846, -0.7794760011071779626 ) ) ;
#65648 = B_SPLINE_CURVE_WITH_KNOTS ( 'NONE', 3,
 ( #70389, #33317, #87108, #79996 ),
 .UNSPECIFIED., .F., .F.,
 ( 4, 4 ),
 ( 0.000000000000000000, 9.999999999998900014E-05 ),
 .UNSPECIFIED. ) ;
#65649 = DIRECTION ( 'NONE',  ( -0.000000000000000000, 1.000000000000000000, -0.000000000000000000 ) ) ;
#65650 = AXIS2_PLACEMENT_3D ( 'NONE', #88084, #10953, #64773 ) ;
#65651 = CARTESIAN_POINT ( 'NONE',  ( 10.68713020350923060, -6.376774720514430506, -28.05292731626249392 ) ) ;
#65652 = CARTESIAN_POINT ( 'NONE',  ( -18.78340662496949776, 8.880393494302802893, 11.49999999999999645 ) ) ;
#65653 = CARTESIAN_POINT ( 'NONE',  ( -6.901944873432418248, -5.876774720514410077, 19.15221817653406688 ) ) ;
#65654 = PLANE ( 'NONE',  #69671 ) ;
#65655 = CARTESIAN_POINT ( 'NONE',  ( -6.082769120682566921, -21.99330073093985405, 11.49999999999999645 ) ) ;
#65656 = EDGE_LOOP ( 'NONE', ( #23995, #68424, #79528, #14886 ) ) ;
#65657 = CARTESIAN_POINT ( 'NONE',  ( 30.53060340732036337, -4.740660005057330650, -2.970021620632059101 ) ) ;
#65658 = CARTESIAN_POINT ( 'NONE',  ( -103.6228709571500559, -29.50250243563736774, 8.947779886222138046 ) ) ;
#65659 = EDGE_LOOP ( 'NONE', ( #10806, #88498, #30233, #52564 ) ) ;
#65660 = CARTESIAN_POINT ( 'NONE',  ( 9.769481717609929561, -17.74358427669893956, -1.500000000000002220 ) ) ;
#65661 = EDGE_CURVE ( 'NONE', #9193, #14515, #97704, .T. ) ;
#65662 = CARTESIAN_POINT ( 'NONE',  ( -108.6228709571500559, -24.64965695001468404, 8.947790433994176951 ) ) ;
#65663 = FACE_OUTER_BOUND ( 'NONE', #17876, .T. ) ;
#65664 = CARTESIAN_POINT ( 'NONE',  ( -115.6228709571500559, -23.47593901973091235, -1.443836447538997536 ) ) ;
#65665 = ORIENTED_EDGE ( 'NONE', *, *, #464, .T. ) ;
#65667 = EDGE_CURVE ( 'NONE', #71522, #35425, #49429, .T. ) ;
#65666 = CARTESIAN_POINT ( 'NONE',  ( -80.29437483463682668, -25.31554926095677160, 4.970974304119136988 ) ) ;
#65668 = CARTESIAN_POINT ( 'NONE',  ( -30.47287095715007510, -23.47596699454220470, 11.42688508591989560 ) ) ;
#65669 = CARTESIAN_POINT ( 'NONE',  ( 18.34943919012036773, 8.063251210807163005, -1.500000000000002220 ) ) ;
#65670 = CARTESIAN_POINT ( 'NONE',  ( -0.5131542516139314669, 21.03015271272555253, 11.49999999999999645 ) ) ;
#65671 = FACE_BOUND ( 'NONE', #77494, .T. ) ;
#65672 = CARTESIAN_POINT ( 'NONE',  ( 3.300000000000004263, 2.247226876435393361E-15, -18.35000000000000142 ) ) ;
#65673 = CARTESIAN_POINT ( 'NONE',  ( 15.63414672909509839, 15.54323407889855879, -1.500000000000002220 ) ) ;
#65674 = VECTOR ( 'NONE', #23696, 1000.000000000000000 ) ;
#65675 = ADVANCED_FACE ( 'NONE', ( #96577 ), #67732, .T. ) ;
#65676 = CARTESIAN_POINT ( 'NONE',  ( -46.62287095715004881, -23.47593901973091235, -1.443836447539009749 ) ) ;
#65677 = EDGE_CURVE ( 'NONE', #84515, #18736, #99055, .T. ) ;
#65678 = CARTESIAN_POINT ( 'NONE',  ( -47.55620429048338593, -24.65952944569304606, 1.056160979905693686 ) ) ;
#65679 = CARTESIAN_POINT ( 'NONE',  ( -50.36897396760109302, -25.18440102080580445, 3.294677851422761261 ) ) ;
#65680 = LINE ( 'NONE', #88995, #31614 ) ;
#65681 = CARTESIAN_POINT ( 'NONE',  ( -31.62287095715005236, -24.65952944569304250, 1.056160979905689690 ) ) ;
#65682 = ORIENTED_EDGE ( 'NONE', *, *, #21471, .T. ) ;
#65683 = VERTEX_POINT ( 'NONE', #37178 ) ;
#65684 = LINE ( 'NONE', #42834, #68090 ) ;
#65685 = DIRECTION ( 'NONE',  ( 1.000000000000000000, -1.988296846060374587E-13, 0.000000000000000000 ) ) ;
#65686 = CARTESIAN_POINT ( 'NONE',  ( 22.65031661608483660, 500000.0000000000582, -20.71116937900383093 ) ) ;
#65687 = CARTESIAN_POINT ( 'NONE',  ( 20.53815866822273861, -0.6333348845813139283, -1.500000000000002220 ) ) ;
#65688 = AXIS2_PLACEMENT_3D ( 'NONE', #57968, #34621, #79777 ) ;
#65689 = VERTEX_POINT ( 'NONE', #89966 ) ;
#65690 = CARTESIAN_POINT ( 'NONE',  ( 3.750000000000001776, 26.59999999999999432, 2.100000000000000089 ) ) ;
#65691 = CARTESIAN_POINT ( 'NONE',  ( -10.21991166328316325, 3.845527176268170422, 29.42879868625613327 ) ) ;
#65692 = FACE_OUTER_BOUND ( 'NONE', #42514, .T. ) ;
#65693 = CARTESIAN_POINT ( 'NONE',  ( -12.45998644600372884, -18.51849504856558681, -1.500000000000002220 ) ) ;
#65694 = AXIS2_PLACEMENT_3D ( 'NONE', #46810, #78729, #23437 ) ;
#65695 = CARTESIAN_POINT ( 'NONE',  ( -0.07188169300783603388, -22.11943499646449141, 0.5637492489085904612 ) ) ;
#65696 = CARTESIAN_POINT ( 'NONE',  ( -31.58953762381672092, -23.48783264082477729, -1.443836473390074149 ) ) ;
#65697 = VERTEX_POINT ( 'NONE', #12830 ) ;
#65698 = CARTESIAN_POINT ( 'NONE',  ( -32.62287095715004881, -23.72773821059535848, 11.05748984161097503 ) ) ;
#65699 = CARTESIAN_POINT ( 'NONE',  ( -51.57158818203188844, -25.29445700113289419, 4.475956743242817559 ) ) ;
#65700 = CARTESIAN_POINT ( 'NONE',  ( 20.25184064777635484, 4.944226511633750043, 11.49999999999998934 ) ) ;
#65701 = VERTEX_POINT ( 'NONE', #97575 ) ;
#65703 = ORIENTED_EDGE ( 'NONE', *, *, #86319, .T. ) ;
#65702 = DIRECTION ( 'NONE',  ( 0.000000000000000000, -0.9999999999976377785, -2.173523156925979975E-06 ) ) ;
#65704 = EDGE_CURVE ( 'NONE', #88376, #71422, #78280, .T. ) ;
#65705 = VERTEX_POINT ( 'NONE', #82349 ) ;
#65706 = CARTESIAN_POINT ( 'NONE',  ( -68.93918693012690824, -25.25935051156955780, 6.184868435727651992 ) ) ;
#65707 = CARTESIAN_POINT ( 'NONE',  ( -18.71117167593497399, 9.704403692310313190, -1.500000000000002220 ) ) ;
#65708 = ORIENTED_EDGE ( 'NONE', *, *, #15186, .F. ) ;
#65709 = FACE_OUTER_BOUND ( 'NONE', #31754, .T. ) ;
#65710 = DIRECTION ( 'NONE',  ( 1.000000000000000000, 0.000000000000000000, 0.000000000000000000 ) ) ;
#65711 = DIRECTION ( 'NONE',  ( 0.000000000000000000, -2.173523156925979552E-06, 0.9999999999976378895 ) ) ;
#65712 = EDGE_CURVE ( 'NONE', #59310, #82863, #81858, .T. ) ;
#65713 = FACE_OUTER_BOUND ( 'NONE', #29823, .T. ) ;
#65714 = DIRECTION ( 'NONE',  ( 0.000000000000000000, -0.9999999999976377785, -2.173523156925979975E-06 ) ) ;
#65715 = CARTESIAN_POINT ( 'NONE',  ( -6.994818212361641585, 20.52682044044541598, -1.500000000000002220 ) ) ;
#65716 = CARTESIAN_POINT ( 'NONE',  ( -81.48149462243461016, -25.12224216488500517, 6.293943252966847091 ) ) ;
#65718 = ORIENTED_EDGE ( 'NONE', *, *, #55288, .T. ) ;
#65717 = CARTESIAN_POINT ( 'NONE',  ( -4.073883676365832152, 21.86232641878667593, 11.49999999999999645 ) ) ;
#65719 = CARTESIAN_POINT ( 'NONE',  ( -51.39979512284951824, -25.24728839109623024, 5.729492026579687369 ) ) ;
#65720 = DIRECTION ( 'NONE',  ( 0.7071067811865476838, 0.000000000000000000, -0.7071067811865474617 ) ) ;
#65721 = CARTESIAN_POINT ( 'NONE',  ( -106.5228709571500758, -23.95044443724991723, 10.65354141964648704 ) ) ;
#65722 = VERTEX_POINT ( 'NONE', #43799 ) ;
#65723 = EDGE_CURVE ( 'NONE', #47263, #40585, #37138, .T. ) ;
#65724 = EDGE_CURVE ( 'NONE', #94858, #67184, #28701, .T. ) ;
#65726 = ORIENTED_EDGE ( 'NONE', *, *, #58426, .T. ) ;
#65725 = CARTESIAN_POINT ( 'NONE',  ( -104.6228709571500559, -23.47596703998600631, 11.44779298504227860 ) ) ;
#65727 = EDGE_LOOP ( 'NONE', ( #10418, #66470, #78744, #59926 ) ) ;
#65728 = CARTESIAN_POINT ( 'NONE',  ( -10.30982817980527777, -21.98926139291979709, -1.497999999999531928 ) ) ;
#65729 = LINE ( 'NONE', #98133, #30801 ) ;
#65730 = CARTESIAN_POINT ( 'NONE',  ( 22.02124265030973760, 3.456774720514426136, 16.20402280011862217 ) ) ;
#65731 = DIRECTION ( 'NONE',  ( 0.000000000000000000, -1.000000000000000000, 0.000000000000000000 ) ) ;
#65732 = VERTEX_POINT ( 'NONE', #27580 ) ;
#65733 = CARTESIAN_POINT ( 'NONE',  ( -39.52287095715006870, -23.48786465467241058, 11.44779295918255180 ) ) ;
#65734 = CARTESIAN_POINT ( 'NONE',  ( 12.99221220249228281, -18.32192329980629708, -1.500000000000002220 ) ) ;
#65735 = EDGE_CURVE ( 'NONE', #58117, #12272, #51914, .T. ) ;
#65736 = EDGE_LOOP ( 'NONE', ( #34736, #80622, #56960, #60702 ) ) ;
#65737 = PLANE ( 'NONE',  #75755 ) ;
#65738 = CARTESIAN_POINT ( 'NONE',  ( -101.5910247417354100, -24.15620529776628800, 10.23563542870660292 ) ) ;
#65739 = CARTESIAN_POINT ( 'NONE',  ( 5.325188327271017208, 5.356774720514426491, -25.45818409267644711 ) ) ;
#65740 = CARTESIAN_POINT ( 'NONE',  ( -49.52287095715007581, -23.47593901973090169, -1.443836447538997092 ) ) ;
#65741 = CARTESIAN_POINT ( 'NONE',  ( -30.57951640616625255, -25.14064729901805251, 2.712351064733618422 ) ) ;
#65742 = CARTESIAN_POINT ( 'NONE',  ( 17.63768857353127828, -8.544740250177758512, 11.49999999999998934 ) ) ;
#65743 = CARTESIAN_POINT ( 'NONE',  ( -49.70995324199571996, -25.30398808162055957, 4.467198061186349989 ) ) ;
#65744 = ORIENTED_EDGE ( 'NONE', *, *, #90586, .T. ) ;
#65745 = CARTESIAN_POINT ( 'NONE',  ( 15.50980990363467882, 14.95361599516425244, -1.500000000000002220 ) ) ;
#65746 = CARTESIAN_POINT ( 'NONE',  ( 14.52511747680497933, -5.965225279485572685, -27.86035006098926559 ) ) ;
#65747 = CARTESIAN_POINT ( 'NONE',  ( -119.6228709571500559, -23.47596703998600631, 11.44779298504227860 ) ) ;
#65748 = DIRECTION ( 'NONE',  ( 0.000000000000000000, 1.000000000000000000, 0.000000000000000000 ) ) ;
#65749 = CARTESIAN_POINT ( 'NONE',  ( -74.62287095715005592, -29.50250243563736774, 8.947779886222143375 ) ) ;
#65750 = CARTESIAN_POINT ( 'NONE',  ( 13.56796309060646166, -18.52494293750034871, -1.500000000000002220 ) ) ;
#65751 = EDGE_CURVE ( 'NONE', #91850, #65428, #90960, .T. ) ;
#65752 = AXIS2_PLACEMENT_3D ( 'NONE', #48571, #40938, #79495 ) ;
#65753 = EDGE_CURVE ( 'NONE', #82055, #72410, #58530, .T. ) ;
#65754 = PERSON_AND_ORGANIZATION ( #70597, #27821 ) ;
#65755 = LINE ( 'NONE', #41398, #17538 ) ;
#65756 = CARTESIAN_POINT ( 'NONE',  ( -49.60652983502191660, -23.73766607897670156, -1.055555164236457344 ) ) ;
#65757 = CARTESIAN_POINT ( 'NONE',  ( 5.780499401231428358, -19.25771307485560158, 11.49999999999999645 ) ) ;
#65758 = CARTESIAN_POINT ( 'NONE',  ( -10.79305683637731228, 0.3587747205144057872, -27.49869550653261285 ) ) ;
#65759 = CARTESIAN_POINT ( 'NONE',  ( -12.65407072091355722, -0.3587747205143968499, -26.15404995688569301 ) ) ;
#65761 = DIRECTION ( 'NONE',  ( 0.000000000000000000, 0.9999999999976377785, 2.173523156925979128E-06 ) ) ;
#65760 = AXIS2_PLACEMENT_3D ( 'NONE', #34998, #18762, #41625 ) ;
#65762 = CARTESIAN_POINT ( 'NONE',  ( -65.62287095715005592, -24.99132157543084176, 2.256160258750667502 ) ) ;
#65763 = CARTESIAN_POINT ( 'NONE',  ( 282.9764569301858046, 6.475225279485573360, 20.79159422840526616 ) ) ;
#65764 = CARTESIAN_POINT ( 'NONE',  ( -18.24115112668064853, 7.888873183027880209, -1.500000000000002220 ) ) ;
#65765 = ADVANCED_FACE ( 'NONE', ( #50915 ), #76637, .T. ) ;
#65766 = AXIS2_PLACEMENT_3D ( 'NONE', #87423, #94534, #47873 ) ;
#65767 = CARTESIAN_POINT ( 'NONE',  ( -113.6312417240655890, -23.48783264082477018, -1.443836473390084363 ) ) ;
#65768 = CARTESIAN_POINT ( 'NONE',  ( 10.64064036176630879, -16.58286410872727146, -1.500000000000002220 ) ) ;
#65769 = VECTOR ( 'NONE', #10749, 1000.000000000000114 ) ;
#65770 = CARTESIAN_POINT ( 'NONE',  ( -60.55620429048339304, -23.48783264082478084, -1.443836473390068820 ) ) ;
#65771 = EDGE_CURVE ( 'NONE', #37337, #14386, #32202, .T. ) ;
#65772 = EDGE_CURVE ( 'NONE', #89711, #84354, #92770, .T. ) ;
#65773 = APPROVAL_DATE_TIME ( #71868, #19617 ) ;
#65774 = CARTESIAN_POINT ( 'NONE',  ( 14.46675407819882331, 3.972730170967898378, -28.29579275198952359 ) ) ;
#65775 = CARTESIAN_POINT ( 'NONE',  ( 3.160575456146155204, -6.376774720514408301, 18.86877352677795372 ) ) ;
#65776 = CARTESIAN_POINT ( 'NONE',  ( -18.82610421443283499, -8.410905081555696938, 11.49999999999999645 ) ) ;
#65777 = CARTESIAN_POINT ( 'NONE',  ( -42.62287095715007013, -24.34917612406838217, 0.1852690917426573769 ) ) ;
#65778 = PERSON ( 'NAUO-PER5', 'UNSPECIFIED', 'UNSPECIFIED', ('UNSPECIFIED'), ('UNSPECIFIED'), ('UNSPECIFIED') ) ;
#65779 = CARTESIAN_POINT ( 'NONE',  ( 0.4201012023153268271, 22.63755686032812164, 11.49999999999999645 ) ) ;
#65780 = ORIENTED_EDGE ( 'NONE', *, *, #64836, .F. ) ;
#65781 = CARTESIAN_POINT ( 'NONE',  ( -126.6228709571500559, -23.47593901973091235, -1.443836447538995760 ) ) ;
#65782 = CARTESIAN_POINT ( 'NONE',  ( -97.54990185180675155, -24.34968618360934300, 0.1864209137778855829 ) ) ;
#65783 = CARTESIAN_POINT ( 'NONE',  ( -110.6228709571500701, -24.62285846362216191, 9.038163152653526211 ) ) ;
#65784 = CARTESIAN_POINT ( 'NONE',  ( -1.304987980769231948, -5.876774720514413630, 19.76512419871795245 ) ) ;
#65785 = VERTEX_POINT ( 'NONE', #86727 ) ;
#65786 = EDGE_LOOP ( 'NONE', ( #10427, #24596, #10497, #18784 ) ) ;
#65787 = EDGE_CURVE ( 'NONE', #10045, #18831, #95343, .T. ) ;
#65788 = CARTESIAN_POINT ( 'NONE',  ( -99.29763458690094069, -25.24802974043947046, 6.184591646183218216 ) ) ;
#65789 = CARTESIAN_POINT ( 'NONE',  ( -6.237877366497927234, -22.00199818733190327, 11.49999999999998934 ) ) ;
#65790 = CARTESIAN_POINT ( 'NONE',  ( -105.5562042904834072, -24.99132157543166954, 2.256160258750668834 ) ) ;
#65791 = CARTESIAN_POINT ( 'NONE',  ( 2.580163054138214562, 21.43444414123800712, -1.500000000000002220 ) ) ;
#65792 = CARTESIAN_POINT ( 'NONE',  ( -41.32836283488544638, -2.803225279485573207, 39.26872235229541985 ) ) ;
#65793 = LINE ( 'NONE', #12474, #20916 ) ;
#65794 = CARTESIAN_POINT ( 'NONE',  ( 15.74396088501716839, 16.14010210793005839, 11.49999999999999645 ) ) ;
#65795 = ORIENTED_EDGE ( 'NONE', *, *, #15691, .F. ) ;
#65796 = CARTESIAN_POINT ( 'NONE',  ( -33.52287095715006160, -23.48786465467240347, 11.44779295918255357 ) ) ;
#65797 = CARTESIAN_POINT ( 'NONE',  ( -12.87221125579857528, -17.80329210173279364, -1.500000000000002220 ) ) ;
#65798 = CARTESIAN_POINT ( 'NONE',  ( -44.51365804008561611, -23.73791477778911130, 11.05961554403171121 ) ) ;
#65799 = CARTESIAN_POINT ( 'NONE',  ( -29.10172430483776651, -25.21724726705176778, 6.373704058171686171 ) ) ;
#65800 = VERTEX_POINT ( 'NONE', #7211 ) ;
#65801 = CARTESIAN_POINT ( 'NONE',  ( -89.62287095714998486, -24.51387760970724372, 9.387446482453427166 ) ) ;
#65802 = CARTESIAN_POINT ( 'NONE',  ( 0.03625801282051022839, -5.876774720514410077, 19.27714342948718240 ) ) ;
#65803 = VERTEX_POINT ( 'NONE', #63926 ) ;
#65804 = CARTESIAN_POINT ( 'NONE',  ( 31.93426202889373400, -0.3587747205144265483, 6.907000118922838716 ) ) ;
#65805 = CARTESIAN_POINT ( 'NONE',  ( -5.951451697817415010, -19.63005813332872762, -1.500000000000002220 ) ) ;
#65806 = ORIENTED_EDGE ( 'NONE', *, *, #64884, .T. ) ;
#65807 = EDGE_LOOP ( 'NONE', ( #65240, #29352, #72448, #16676 ) ) ;
#65808 = ORIENTED_EDGE ( 'NONE', *, *, #97937, .F. ) ;
#65809 = DIRECTION ( 'NONE',  ( 0.000000000000000000, -1.000000000000000000, 0.000000000000000000 ) ) ;
#65810 = LINE ( 'NONE', #58184, #64922 ) ;
#65811 = CARTESIAN_POINT ( 'NONE',  ( -104.5573922987845492, -23.73791477778912196, 11.05961554403170410 ) ) ;
#65812 = CARTESIAN_POINT ( 'NONE',  ( -19.36681041099238598, 6.328833669845586485, -1.500000000000002220 ) ) ;
#65813 = ORIENTED_EDGE ( 'NONE', *, *, #91636, .F. ) ;
#65814 = FACE_OUTER_BOUND ( 'NONE', #509, .T. ) ;
#65815 = CARTESIAN_POINT ( 'NONE',  ( -29.48777410446400182, -24.26373688684574503, 9.817618405055078767 ) ) ;
#65816 = CARTESIAN_POINT ( 'NONE',  ( -105.5519832311244812, -24.40034930558991633, 0.3402023900116059041 ) ) ;
#65817 = DIRECTION ( 'NONE',  ( -2.352173255807804438E-16, 2.352173255807796056E-16, 1.000000000000000000 ) ) ;
#65818 = ORIENTED_EDGE ( 'NONE', *, *, #40054, .F. ) ;
#65819 = CARTESIAN_POINT ( 'NONE',  ( 26.73860345374794889, 5.356774720514427379, -3.111611894936215705 ) ) ;
#65820 = CARTESIAN_POINT ( 'NONE',  ( -97.62287095715005592, -24.66019654487200086, 8.947790411086124607 ) ) ;
#65821 = ORIENTED_EDGE ( 'NONE', *, *, #79561, .T. ) ;
#65822 = CARTESIAN_POINT ( 'NONE',  ( -16.75865769207039335, -12.26659692683164593, 11.49999999999998934 ) ) ;
#65823 = ORIENTED_EDGE ( 'NONE', *, *, #25024, .T. ) ;
#65825 = ORIENTED_EDGE ( 'NONE', *, *, #89295, .T. ) ;
#65824 = CARTESIAN_POINT ( 'NONE',  ( -101.5957409211337392, -23.73766607897670511, -1.055555164236452237 ) ) ;
#65826 = AXIS2_PLACEMENT_3D ( 'NONE', #79488, #9975, #40929 ) ;
#65827 = ADVANCED_FACE ( 'NONE', ( #15321, #22915 ), #6717, .F. ) ;
#65828 = PLANE ( 'NONE',  #52002 ) ;
#65829 = CARTESIAN_POINT ( 'NONE',  ( -73.52287095715007581, -24.64898659630528854, 1.056161002820824368 ) ) ;
#65830 = ORIENTED_EDGE ( 'NONE', *, *, #50224, .F. ) ;
#65831 = VERTEX_POINT ( 'NONE', #84841 ) ;
#65832 = VECTOR ( 'NONE', #33471, 1000.000000000000000 ) ;
#65833 = CARTESIAN_POINT ( 'NONE',  ( 27.53860345374771867, 4.772774720514425972, -9.482392034746240483 ) ) ;
#65834 = CARTESIAN_POINT ( 'NONE',  ( -123.5228709571500616, -24.64965694238408034, 8.947790433994191162 ) ) ;
#65835 = AXIS2_PLACEMENT_3D ( 'NONE', #4824, #41904, #34283 ) ;
#65836 = LINE ( 'NONE', #90639, #71224 ) ;
#65837 = CARTESIAN_POINT ( 'NONE',  ( -74.62287095715008434, -24.50216790748205753, 0.6166512839542480640 ) ) ;
#65839 = ORIENTED_EDGE ( 'NONE', *, *, #47151, .T. ) ;
#65838 = CARTESIAN_POINT ( 'NONE',  ( 18.88560736741940005, 11.47387103136259690, 11.49999999999999645 ) ) ;
#65840 = B_SPLINE_CURVE_WITH_KNOTS ( 'NONE', 3,
 ( #22795, #37548, #61896, #77092 ),
 .UNSPECIFIED., .F., .F.,
 ( 4, 4 ),
 ( 0.000000000000000000, 1.000000000000000000 ),
 .UNSPECIFIED. ) ;
#65841 = AXIS2_PLACEMENT_3D ( 'NONE', #70586, #32019, #40141 ) ;
#65842 = CARTESIAN_POINT ( 'NONE',  ( -47.62287095715004170, -24.51387760970723662, 9.387446482453421837 ) ) ;
#65843 = CARTESIAN_POINT ( 'NONE',  ( -3.801653518169780366, -22.29579330195574016, 11.49999999999998934 ) ) ;
#65844 = EDGE_CURVE ( 'NONE', #34495, #34088, #81813, .T. ) ;
#65845 = EDGE_CURVE ( 'NONE', #71576, #81001, #91512, .T. ) ;
#65846 = AXIS2_PLACEMENT_3D ( 'NONE', #11966, #19574, #42935 ) ;
#65847 = B_SPLINE_CURVE_WITH_KNOTS ( 'NONE', 3,
 ( #75257, #97598, #27098, #89492 ),
 .UNSPECIFIED., .F., .F.,
 ( 4, 4 ),
 ( 0.000000000000000000, 9.999999999998897304E-05 ),
 .UNSPECIFIED. ) ;
#65848 = EDGE_CURVE ( 'NONE', #14129, #30802, #44258, .T. ) ;
#65850 = ORIENTED_EDGE ( 'NONE', *, *, #97309, .T. ) ;
#65849 = CARTESIAN_POINT ( 'NONE',  ( -115.6244851806074507, -24.83644354573579349, 8.397322867130093016 ) ) ;
#65851 = ORIENTED_EDGE ( 'NONE', *, *, #57176, .T. ) ;
#65852 = ADVANCED_FACE ( 'NONE', ( #2006 ), #51753, .F. ) ;
#65853 = CARTESIAN_POINT ( 'NONE',  ( -10.34999999999997833, 27.69999999999999929, 2.100000000000000089 ) ) ;
#65854 = FACE_OUTER_BOUND ( 'NONE', #3647, .T. ) ;
#65855 = VERTEX_POINT ( 'NONE', #79614 ) ;
#65856 = CARTESIAN_POINT ( 'NONE',  ( -19.98373207111551508, 7.008865001458166155, 11.49999999999998934 ) ) ;
#65857 = CARTESIAN_POINT ( 'NONE',  ( -7.318926569091948942, -5.876774720514417183, 20.09505574050193033 ) ) ;
#65858 = PLANE ( 'NONE',  #79 ) ;
#65859 = CARTESIAN_POINT ( 'NONE',  ( 19.02167141253037030, -11.55642654327076535, -1.500000000000002220 ) ) ;
#65860 = DIRECTION ( 'NONE',  ( -1.000000000000000000, -3.773278334444167608E-23, -8.201307833595939069E-29 ) ) ;
#65861 = EDGE_CURVE ( 'NONE', #56523, #13066, #41064, .T. ) ;
#65862 = ORIENTED_EDGE ( 'NONE', *, *, #41198, .T. ) ;
#65863 = CARTESIAN_POINT ( 'NONE',  ( -65.62287095715005592, -23.47593901973091235, -1.443836447539006196 ) ) ;
#65864 = DIRECTION ( 'NONE',  ( -1.000000000000000000, 0.000000000000000000, -0.000000000000000000 ) ) ;
#65865 = VECTOR ( 'NONE', #23278, 1000.000000000000114 ) ;
#65866 = CARTESIAN_POINT ( 'NONE',  ( -36.48443619261569637, -24.51419770103156637, 9.386484678747175181 ) ) ;
#65867 = DIRECTION ( 'NONE',  ( -0.5656310827093757876, -0.8246584009594636333, -1.161164194647626387E-16 ) ) ;
#65868 = ADVANCED_FACE ( 'NONE', ( #87737 ), #18222, .F. ) ;
#65869 = CARTESIAN_POINT ( 'NONE',  ( -17.32436372870746055, -8.985247798433253053, -1.500000000000002220 ) ) ;
#65870 = CARTESIAN_POINT ( 'NONE',  ( -7.526967427842778946, 20.06989004931119425, 11.49999999999998934 ) ) ;
#65871 = CARTESIAN_POINT ( 'NONE',  ( -26.85447117215736412, -24.57999539825883772, 1.825772105227124520 ) ) ;
#65872 = PLANE ( 'NONE',  #29275 ) ;
#65873 = CARTESIAN_POINT ( 'NONE',  ( -77.51234862871442033, -23.96119346886880663, -0.6495511937832126881 ) ) ;
#65874 = CARTESIAN_POINT ( 'NONE',  ( 22.20067557195093855, 5.203973054738295190, -1.500000000000002220 ) ) ;
#65875 = EDGE_CURVE ( 'NONE', #67215, #21350, #72519, .T. ) ;
#65876 = DIRECTION ( 'NONE',  ( -0.8235638664188268399, 2.722359648489627795E-18, 0.5672235519874618825 ) ) ;
#65877 = CARTESIAN_POINT ( 'NONE',  ( -98.58671180656558874, -24.51314013834316086, 0.6176544820404117342 ) ) ;
#65878 = CARTESIAN_POINT ( 'NONE',  ( 8.371512145086501988, -1.000000000000002665, -3.746884140868835367 ) ) ;
#65879 = CARTESIAN_POINT ( 'NONE',  ( 17.57725459251073019, -9.329341740261039462, 11.49999999999999645 ) ) ;
#65880 = CARTESIAN_POINT ( 'NONE',  ( -104.5976451972810679, -23.48783264082477373, -1.443836473390085917 ) ) ;
#65881 = DIRECTION ( 'NONE',  ( -3.469446951953614189E-15, 1.000000000000000000, 0.000000000000000000 ) ) ;
#65882 = CARTESIAN_POINT ( 'NONE',  ( -98.52287095715007581, -23.47593901973090524, -1.443836447538996648 ) ) ;
#65883 = ORIENTED_EDGE ( 'NONE', *, *, #98545, .F. ) ;
#65884 = CARTESIAN_POINT ( 'NONE',  ( -82.52287095715007581, -24.66019654487199730, 8.947790411086122830 ) ) ;
#65885 = LINE ( 'NONE', #26299, #79883 ) ;
#65886 = EDGE_CURVE ( 'NONE', #52727, #56992, #63688, .T. ) ;
#65887 = CARTESIAN_POINT ( 'NONE',  ( -4.559408409702599307, -21.23122434433648209, -1.500000000000002220 ) ) ;
#65888 = CARTESIAN_POINT ( 'NONE',  ( -67.58953762381672448, -24.65952944569304606, 1.056160979905700126 ) ) ;
#65889 = CARTESIAN_POINT ( 'NONE',  ( -18.58057592369839384, -6.135153870360039896, -1.500000000000002220 ) ) ;
#65890 = VECTOR ( 'NONE', #66873, 1000.000000000000000 ) ;
#65891 = CARTESIAN_POINT ( 'NONE',  ( -77.62287095715007013, -24.65952944569304606, 1.056160979905699016 ) ) ;
#65892 = EDGE_CURVE ( 'NONE', #4551, #11386, #24135, .T. ) ;
#65893 = PERSON_AND_ORGANIZATION_ROLE ( 'design_supplier' ) ;
#65894 = CARTESIAN_POINT ( 'NONE',  ( -69.62287095715005592, -23.47596703998600631, 11.44779298504227683 ) ) ;
#65895 = CARTESIAN_POINT ( 'NONE',  ( -3.558151220431595707, 20.12126150705307381, 11.49999999999999645 ) ) ;
#65896 = CARTESIAN_POINT ( 'NONE',  ( -28.98875734969026041, 0.3587747205144265483, 17.86602280011862476 ) ) ;
#65897 = B_SPLINE_CURVE_WITH_KNOTS ( 'NONE', 3,
 ( #787, #1797, #78397, #2304 ),
 .UNSPECIFIED., .F., .F.,
 ( 4, 4 ),
 ( 0.1205861075877675687, 0.1295925388598832828 ),
 .UNSPECIFIED. ) ;
#65898 = AXIS2_PLACEMENT_3D ( 'NONE', #598, #31549, #32553 ) ;
#65899 = CARTESIAN_POINT ( 'NONE',  ( -0.1490770655183801252, -21.12008023607309681, -1.443836447538997758 ) ) ;
#65900 = ORIENTED_EDGE ( 'NONE', *, *, #87507, .T. ) ;
#65901 = DIRECTION ( 'NONE',  ( -1.000000000000000000, -3.773278334444166432E-23, -8.201307841325785021E-29 ) ) ;
#65902 = DIRECTION ( 'NONE',  ( -0.9980236263794188822, 0.000000000000000000, 0.06283980576413537855 ) ) ;
#65903 = VECTOR ( 'NONE', #50309, 1000.000000000000000 ) ;
#65904 = CARTESIAN_POINT ( 'NONE',  ( -116.5884057677307055, -24.51419770103160189, 9.386484678747169852 ) ) ;
#65905 = AXIS2_PLACEMENT_3D ( 'NONE', #90000, #75752, #98092 ) ;
#65906 = CARTESIAN_POINT ( 'NONE',  ( -109.5890824698541195, -24.34968618360934300, 0.1864209137778879144 ) ) ;
#65907 = EDGE_LOOP ( 'NONE', ( #78193, #18852, #18685, #12892 ) ) ;
#65908 = DIRECTION ( 'NONE',  ( 0.000000000000000000, -1.000000000000000000, 0.000000000000000000 ) ) ;
#65909 = CIRCLE ( 'NONE', #20523, 28.96799999999999642 ) ;
#65910 = CARTESIAN_POINT ( 'NONE',  ( 16.94363762160741516, 15.55198921429254533, 11.49999999999999645 ) ) ;
#65911 = CARTESIAN_POINT ( 'NONE',  ( -4.374245501123523283, 22.36648047097513725, 11.49999999999998934 ) ) ;
#65912 = CARTESIAN_POINT ( 'NONE',  ( 4.038745349937860496, -6.376774720514429617, 21.81354843764681206 ) ) ;
#65913 = FACE_OUTER_BOUND ( 'NONE', #49215, .T. ) ;
#65914 = CARTESIAN_POINT ( 'NONE',  ( -49.89338008494267740, -25.20873888344022973, 3.392385934324123387 ) ) ;
#65915 = CARTESIAN_POINT ( 'NONE',  ( -54.52287095715005449, -23.48783264082476308, -1.443836473390096797 ) ) ;
#65916 = PLANE ( 'NONE',  #83740 ) ;
#65917 = CARTESIAN_POINT ( 'NONE',  ( -21.47987282208850601, -4.139150239982721580, 11.49999999999998934 ) ) ;
#65918 = CARTESIAN_POINT ( 'NONE',  ( -69.63096295692471926, -24.35071581493542681, 9.817618358456032368 ) ) ;
#65919 = CARTESIAN_POINT ( 'NONE',  ( 7.150000000000004796, -2.000000000000001776, 19.19609335255483984 ) ) ;
#65920 = CARTESIAN_POINT ( 'NONE',  ( -90.52287095715006160, -25.00158670708909625, 2.256160236439166411 ) ) ;
#65921 = CARTESIAN_POINT ( 'NONE',  ( -0.02075734969026423599, -0.3587747205144213303, -0.08597719988137648983 ) ) ;
#65922 = VERTEX_POINT ( 'NONE', #35450 ) ;
#65923 = CARTESIAN_POINT ( 'NONE',  ( -8.052747710315523832, 18.77774781879659116, 11.49999999999998934 ) ) ;
#65924 = ORIENTED_EDGE ( 'NONE', *, *, #47746, .T. ) ;
#65925 = ORIENTED_EDGE ( 'NONE', *, *, #9192, .F. ) ;
#65926 = VERTEX_POINT ( 'NONE', #96343 ) ;
#65927 = ORIENTED_EDGE ( 'NONE', *, *, #63910, .T. ) ;
#65928 = CARTESIAN_POINT ( 'NONE',  ( -22.84742429131147645, -2.885717679200183738, 11.49999999999998934 ) ) ;
#65929 = DIRECTION ( 'NONE',  ( 3.773278334444167608E-23, -1.000000000000000000, 0.000000000000000000 ) ) ;
#65930 = CARTESIAN_POINT ( 'NONE',  ( 18.63370447891095694, 7.782165041754079304, -1.500000000000002220 ) ) ;
#65931 = EDGE_LOOP ( 'NONE', ( #83018, #51455, #24602, #84876 ) ) ;
#65932 = VECTOR ( 'NONE', #66436, 1000.000000000000000 ) ;
#65933 = CARTESIAN_POINT ( 'NONE',  ( -67.62287095715004170, -24.66019654487199020, 8.947790411086131712 ) ) ;
#65934 = DIRECTION ( 'NONE',  ( 0.000000000000000000, -1.000000000000000000, 0.000000000000000000 ) ) ;
#65935 = CARTESIAN_POINT ( 'NONE',  ( -95.50254368814682948, -24.92564183028979485, 1.928384488918254425 ) ) ;
#65936 = CARTESIAN_POINT ( 'NONE',  ( -53.49617477238062691, -24.35071581493542681, 9.817618358456032368 ) ) ;
#65938 = VERTEX_POINT ( 'NONE', #3506 ) ;
#65937 = CARTESIAN_POINT ( 'NONE',  ( 14.52366289275476419, -15.72616519631134580, 11.49999999999999645 ) ) ;
#65939 = CARTESIAN_POINT ( 'NONE',  ( 6.429811694900724461, -5.876774720514425177, 21.48000018967326596 ) ) ;
#65940 = ORIENTED_EDGE ( 'NONE', *, *, #74432, .F. ) ;
#65941 = AXIS2_PLACEMENT_3D ( 'NONE', #28019, #11290, #58480 ) ;
#65942 = CARTESIAN_POINT ( 'NONE',  ( -17.34812393562427246, -13.96779696820907191, -1.500000000000002220 ) ) ;
#65943 = CARTESIAN_POINT ( 'NONE',  ( -20.26430336558559020, 4.098603726722801710, 11.49999999999998934 ) ) ;
#65944 = ORIENTED_EDGE ( 'NONE', *, *, #49118, .T. ) ;
#65945 = CARTESIAN_POINT ( 'NONE',  ( 2.909586618535765723, -5.876774720514411854, 19.75512108203924200 ) ) ;
#65946 = ORIENTED_EDGE ( 'NONE', *, *, #97647, .F. ) ;
#65947 = ADVANCED_FACE ( 'NONE', ( #73509 ), #4001, .F. ) ;
#65948 = CARTESIAN_POINT ( 'NONE',  ( -129.5228709571500758, -23.47593901973090524, -1.443836447538996204 ) ) ;
#65949 = VERTEX_POINT ( 'NONE', #65920 ) ;
#65951 = EDGE_CURVE ( 'NONE', #12570, #95752, #57795, .T. ) ;
#65950 = CARTESIAN_POINT ( 'NONE',  ( 10.22568704553358643, 6.475225279485576024, -27.02513721610328901 ) ) ;
#65952 = CARTESIAN_POINT ( 'NONE',  ( -16.25153318171239647, -13.25006309444557751, -1.500000000000002220 ) ) ;
#65953 = CARTESIAN_POINT ( 'NONE',  ( 13.84421170697429737, -16.98027460053469895, 11.49999999999999645 ) ) ;
#65954 = EDGE_CURVE ( 'NONE', #33122, #54335, #19208, .T. ) ;
#65955 = CARTESIAN_POINT ( 'NONE',  ( -73.50294862231642412, -24.35071581493543036, 9.817618358456027039 ) ) ;
#65956 = CARTESIAN_POINT ( 'NONE',  ( -22.50818191331092777, 0.9639279967183422837, -1.500000000000002220 ) ) ;
#65957 = EDGE_CURVE ( 'NONE', #88013, #31023, #80861, .T. ) ;
#65958 = AXIS2_PLACEMENT_3D ( 'NONE', #25919, #88325, #64520 ) ;
#65959 = CARTESIAN_POINT ( 'NONE',  ( 0.7041596644206948863, -20.94928778062849162, -1.500000000000002220 ) ) ;
#65960 = CARTESIAN_POINT ( 'NONE',  ( -26.10989220437014424, -24.88148810348265627, 5.384403059502965050 ) ) ;
#65961 = CARTESIAN_POINT ( 'NONE',  ( 6.199338013146583393, -5.876774720514415407, 20.11757922567734980 ) ) ;
#65962 = CARTESIAN_POINT ( 'NONE',  ( -72.62287095715001328, -24.33832256526968507, 0.1851278514119847063 ) ) ;
#65963 = CARTESIAN_POINT ( 'NONE',  ( -91.62287095715004170, -24.64965695001468404, 8.947790433994180503 ) ) ;
#65964 = ORIENTED_EDGE ( 'NONE', *, *, #58819, .T. ) ;
#65965 = VERTEX_POINT ( 'NONE', #50177 ) ;
#65966 = ORIENTED_EDGE ( 'NONE', *, *, #58166, .F. ) ;
#65967 = CARTESIAN_POINT ( 'NONE',  ( -44.52287095715004739, -24.51387760970726148, 9.387446482453421837 ) ) ;
#65968 = ORIENTED_EDGE ( 'NONE', *, *, #78276, .T. ) ;
#65969 = VECTOR ( 'NONE', #32318, 1000.000000000000114 ) ;
#65970 = B_SPLINE_CURVE_WITH_KNOTS ( 'NONE', 3,
 ( #84249, #53820, #14734, #76626 ),
 .UNSPECIFIED., .F., .F.,
 ( 4, 4 ),
 ( 0.000000000000000000, 9.999999999996123101E-05 ),
 .UNSPECIFIED. ) ;
#65971 = CARTESIAN_POINT ( 'NONE',  ( 20.52986552169224410, -6.224258026782483633, -1.500000000000002220 ) ) ;
#65972 = CARTESIAN_POINT ( 'NONE',  ( 0.000000000000000000, 2.682774720514426559, 0.000000000000000000 ) ) ;
#65974 = VERTEX_POINT ( 'NONE', #81116 ) ;
#65973 = VECTOR ( 'NONE', #39348, 1000.000000000000227 ) ;
#65975 = CARTESIAN_POINT ( 'NONE',  ( -16.00611555608923098, 13.71732778110762219, -1.500000000000002220 ) ) ;
#65976 = CARTESIAN_POINT ( 'NONE',  ( 0.000000000000000000, -4.056774720514426669, 0.000000000000000000 ) ) ;
#65977 = CARTESIAN_POINT ( 'NONE',  ( 2.611202098145462891, -6.376774720514420736, 20.45574432200782766 ) ) ;
#65978 = DIRECTION ( 'NONE',  ( 1.000000000000000000, 3.773278334444167608E-23, 8.201307833595939069E-29 ) ) ;
#65979 = AXIS2_PLACEMENT_3D ( 'NONE', #12739, #58938, #90874 ) ;
#65980 = CARTESIAN_POINT ( 'NONE',  ( -101.5487956542387451, -24.51314013834316086, 0.6176544820404185065 ) ) ;
#65981 = CARTESIAN_POINT ( 'NONE',  ( -129.5898459561496168, -23.96169478059714564, 10.65365249895717348 ) ) ;
#65982 = CARTESIAN_POINT ( 'NONE',  ( -2.366842300981895519, -21.98859952056468714, -1.500000000000002220 ) ) ;
#65983 = EDGE_LOOP ( 'NONE', ( #71506, #49729, #30591, #16097 ) ) ;
#65984 = B_SPLINE_CURVE_WITH_KNOTS ( 'NONE', 3,
 ( #35554, #66524, #50278, #90825 ),
 .UNSPECIFIED., .F., .F.,
 ( 4, 4 ),
 ( 0.2306647120247341254, 0.2396711432968496869 ),
 .UNSPECIFIED. ) ;
#65985 = CARTESIAN_POINT ( 'NONE',  ( -81.58821135512123135, -24.35071581493543391, 9.817618358456037697 ) ) ;
#65986 = DIRECTION ( 'NONE',  ( 0.000000000000000000, -0.9999999999976377785, -2.173523156925979975E-06 ) ) ;
#65987 = CARTESIAN_POINT ( 'NONE',  ( -41.77207742203299290, -25.31624564944289091, 4.730364161577088389 ) ) ;
#65988 = CARTESIAN_POINT ( 'NONE',  ( -26.97027047204615968, -24.54739053293899786, 1.590605884330588360 ) ) ;
#65989 = EDGE_CURVE ( 'NONE', #54547, #15218, #11597, .T. ) ;
#65990 = CARTESIAN_POINT ( 'NONE',  ( -10.34999999999999254, 1.999999999999999112, 3.499999999999999112 ) ) ;
#65991 = CARTESIAN_POINT ( 'NONE',  ( 19.36035776617087123, -9.008237321879198234, 11.49999999999998934 ) ) ;
#65992 = DIRECTION ( 'NONE',  ( -3.773278334453079618E-23, 0.9999999999976377785, 2.173523156925979975E-06 ) ) ;
#65993 = CARTESIAN_POINT ( 'NONE',  ( -51.95422829247385721, -25.11539320716599377, 2.804431449967496714 ) ) ;
#65994 = CARTESIAN_POINT ( 'NONE',  ( -64.49990038984530827, -24.35071581493543391, 9.817618358456023486 ) ) ;
#65995 = DIRECTION ( 'NONE',  ( 0.000000000000000000, 0.000000000000000000, -1.000000000000000000 ) ) ;
#65996 = CARTESIAN_POINT ( 'NONE',  ( -0.2110286175373513040, -22.56517410205234597, -1.500000000000002220 ) ) ;
#65997 = FACE_OUTER_BOUND ( 'NONE', #13977, .T. ) ;
#65998 = ORIENTED_EDGE ( 'NONE', *, *, #75188, .F. ) ;
#65999 = CARTESIAN_POINT ( 'NONE',  ( 4.647438682898014761, -5.876774720514418071, 20.26932200457894950 ) ) ;
#66000 = CARTESIAN_POINT ( 'NONE',  ( -70.22287095715009286, -23.47593901973090524, -1.443836447538997980 ) ) ;
#66001 = CARTESIAN_POINT ( 'NONE',  ( -10.60818629614422370, 16.63341085705455669, 11.49999999999999645 ) ) ;
#66002 = CARTESIAN_POINT ( 'NONE',  ( -28.98875734969026041, -0.3587747205144262708, 15.62202280011862321 ) ) ;
#66003 =( BOUNDED_SURFACE ( )  B_SPLINE_SURFACE ( 3, 2, ( 
 ( #68202, #14895, #58715 ),
 ( #15394, #89666, #91526 ),
 ( #7788, #38733, #45375 ),
 ( #83918, #69699, #181 ),
 ( #58230, #44874, #89169 ),
 ( #50606, #13896, #14396 ) ),
 .UNSPECIFIED., .F., .F., .T. ) 
 B_SPLINE_SURFACE_WITH_KNOTS ( ( 4, 2, 4 ),
 ( 3, 3 ),
 ( 0.001113071882895040263, 0.001219813747004279327, 0.001326555611113518392 ),
 ( 0.000000000000000000, 1.000000000000000000 ),
 .UNSPECIFIED. ) 
 GEOMETRIC_REPRESENTATION_ITEM ( )  RATIONAL_B_SPLINE_SURFACE ( (
 ( 1.000000000000000000, 0.7071067811865114905, 1.000000000000000000),
 ( 1.000000000000000000, 0.7264088502634352684, 1.000000000000000000),
 ( 1.000000000000000000, 0.7445305694446069378, 1.000000000000000000),
 ( 1.000000000000000000, 0.7788548593121751296, 1.000000000000000000),
 ( 1.000000000000000000, 0.7952519535464425138, 1.000000000000000000),
 ( 1.000000000000000000, 0.8096947957033885368, 1.000000000000000000) ) ) 
 REPRESENTATION_ITEM ( '' )  SURFACE ( )  );
#66004 = CARTESIAN_POINT ( 'NONE',  ( -119.5228709571501753, -23.73907113216990439, -1.053371485793245688 ) ) ;
#66005 = ORIENTED_EDGE ( 'NONE', *, *, #41936, .F. ) ;
#66006 = DIRECTION ( 'NONE',  ( -1.000000000000000000, -0.000000000000000000, -0.000000000000000000 ) ) ;
#66007 = CARTESIAN_POINT ( 'NONE',  ( -29.40205842853959339, -24.60094121823534508, 2.693430781335976576 ) ) ;
#66008 = DIRECTION ( 'NONE',  ( -3.773278334453079030E-23, 0.9999999999976377785, 2.173523156925979128E-06 ) ) ;
#66009 = CARTESIAN_POINT ( 'NONE',  ( -14.23256820581467785, 16.29125061305494526, -1.500000000000002220 ) ) ;
#66010 = AXIS2_PLACEMENT_3D ( 'NONE', #78767, #32106, #55462 ) ;
#66011 = CARTESIAN_POINT ( 'NONE',  ( -76.58953762381673869, -24.64898659630367916, 1.056161002820385830 ) ) ;
#66012 = CARTESIAN_POINT ( 'NONE',  ( 0.000000000000000000, -5.876774720514426953, 0.000000000000000000 ) ) ;
#66013 = CARTESIAN_POINT ( 'NONE',  ( -10.21384395349167562, -3.451719627175087179, 29.49402280011861777 ) ) ;
#66014 = CARTESIAN_POINT ( 'NONE',  ( -118.6228709571500559, -24.64965695001469115, 8.947790433994175174 ) ) ;
#66015 = ADVANCED_FACE ( 'NONE', ( #20202 ), #58783, .T. ) ;
#66016 = CARTESIAN_POINT ( 'NONE',  ( 16.35176858736616978, 11.14859404531058473, -1.500000000000002220 ) ) ;
#66017 = VERTEX_POINT ( 'NONE', #58294 ) ;
#66018 = AXIS2_PLACEMENT_3D ( 'NONE', #78425, #32260, #63230 ) ;
#66019 = CARTESIAN_POINT ( 'NONE',  ( -5.286950244708777724, -19.55949958832428948, 11.49999999999999645 ) ) ;
#66020 = CARTESIAN_POINT ( 'NONE',  ( 9.492487079130338401, 5.851656861456516978, -26.75003832473357690 ) ) ;
#66021 = ADVANCED_FACE ( 'NONE', ( #89232 ), #74009, .F. ) ;
#66022 = B_SPLINE_CURVE_WITH_KNOTS ( 'NONE', 3,
 ( #80155, #41606, #63279, #86588, #54161, #38414, #31300, #1370, #85585, #69367, #77956, #23678, #78465, #6969 ),
 .UNSPECIFIED., .F., .F.,
 ( 4, 2, 2, 1, 1, 2, 2, 4 ),
 ( 0.000000000000000000, 0.2500000000000028311, 0.3750000000000009992, 0.4374999999999976130, 0.4687499999999932276, 0.4843749999999957256, 0.4999999999999982236, 1.000000000000000000 ),
 .UNSPECIFIED. ) ;
#66023 = CARTESIAN_POINT ( 'NONE',  ( 6.110660513271839456, -6.376774720514422512, 21.43053473047838509 ) ) ;
#66024 = ORIENTED_EDGE ( 'NONE', *, *, #59567, .F. ) ;
#66025 = CARTESIAN_POINT ( 'NONE',  ( 32.53135143123563466, 5.965225279485572685, 6.926385399448451885 ) ) ;
#66026 = CARTESIAN_POINT ( 'NONE',  ( -102.5562042904833788, -23.48783264082478084, -1.443836473390062825 ) ) ;
#66027 = CARTESIAN_POINT ( 'NONE',  ( 8.676776695296466002, 18.57322330470350735, 2.100000000000000089 ) ) ;
#66028 = CARTESIAN_POINT ( 'NONE',  ( 13.57581083383196940, -5.876774720514426953, 20.21213203435597094 ) ) ;
#66029 = CARTESIAN_POINT ( 'NONE',  ( -33.62287095715005592, -23.48783264082477373, -1.443836473390074371 ) ) ;
#66030 = CARTESIAN_POINT ( 'NONE',  ( 15.84714387567644955, -12.28532832577633194, -1.500000000000002220 ) ) ;
#66031 = DIRECTION ( 'NONE',  ( -3.773278334453079618E-23, 0.9999999999976377785, 2.173523156925979975E-06 ) ) ;
#66032 = VERTEX_POINT ( 'NONE', #11104 ) ;
#66033 = VECTOR ( 'NONE', #1059, 1000.000000000000114 ) ;
#66034 = CARTESIAN_POINT ( 'NONE',  ( -50.27385278553439463, -25.31297216834682473, 4.732894841895117999 ) ) ;
#66035 = CARTESIAN_POINT ( 'NONE',  ( -24.57525087998973845, 5.965225279485572685, -15.45548830044932309 ) ) ;
#66036 = CARTESIAN_POINT ( 'NONE',  ( -92.62287095715009855, -24.33927499327855415, 9.819080762295817166 ) ) ;
#66037 = DIRECTION ( 'NONE',  ( -0.000000000000000000, 1.000000000000000000, -0.000000000000000000 ) ) ;
#66038 = LINE ( 'NONE', #64543, #42096 ) ;
#66039 = VECTOR ( 'NONE', #34463, 1000.000000000000000 ) ;
#66040 = CARTESIAN_POINT ( 'NONE',  ( -20.27875734969026311, 6.143225279485574397, 24.00402280011862288 ) ) ;
#66041 = CARTESIAN_POINT ( 'NONE',  ( -28.98875734969026041, 6.376774720514426953, 26.43402280011862615 ) ) ;
#66042 = ORIENTED_EDGE ( 'NONE', *, *, #68576, .T. ) ;
#66043 = AXIS2_PLACEMENT_3D ( 'NONE', #47223, #21861, #14754 ) ;
#66044 = CARTESIAN_POINT ( 'NONE',  ( 19.83649001621966335, 4.521578618930774951, -1.500000000000002220 ) ) ;
#66045 = EDGE_LOOP ( 'NONE', ( #25600, #15023 ) ) ;
#66046 = CARTESIAN_POINT ( 'NONE',  ( -16.74478417649319084, -15.65585335247391896, 11.49999999999998934 ) ) ;
#66047 = CARTESIAN_POINT ( 'NONE',  ( 22.02124265030973760, 7.743225279485574042, 17.60402280011862075 ) ) ;
#66048 = EDGE_LOOP ( 'NONE', ( #9017, #54680, #91077, #86668 ) ) ;
#66049 = CARTESIAN_POINT ( 'NONE',  ( -37.62287095715008434, -23.94994826722515313, -0.6494450866351710872 ) ) ;
#66050 = CARTESIAN_POINT ( 'NONE',  ( -49.51155500790866171, -25.26264100752995745, 6.743855136296660113 ) ) ;
#66051 = DIRECTION ( 'NONE',  ( 1.286817348990133408E-16, 0.000000000000000000, -1.000000000000000000 ) ) ;
#66052 = CARTESIAN_POINT ( 'NONE',  ( -14.79452276021403634, 15.15755283273500531, 11.49999999999999645 ) ) ;
#66053 = CARTESIAN_POINT ( 'NONE',  ( -15.97456084408017674, 15.39233244482803009, -1.500000000000002220 ) ) ;
#66054 = CARTESIAN_POINT ( 'NONE',  ( -6.273408026305254737, 19.60348359158234288, 11.49999999999998934 ) ) ;
#66055 = ORIENTED_EDGE ( 'NONE', *, *, #36199, .T. ) ;
#66056 = CARTESIAN_POINT ( 'NONE',  ( -41.60044768456533859, -23.96119346886880663, -0.6495511937831990323 ) ) ;
#66057 = ORIENTED_EDGE ( 'NONE', *, *, #91909, .T. ) ;
#66058 = CARTESIAN_POINT ( 'NONE',  ( -11.64875734969026233, -5.965225279485572685, 31.02402280011862246 ) ) ;
#66059 = DIRECTION ( 'NONE',  ( 3.773278334444166432E-23, -1.000000000000000000, 0.000000000000000000 ) ) ;
#66060 = ORIENTED_EDGE ( 'NONE', *, *, #64364, .F. ) ;
#66062 = ORIENTED_EDGE ( 'NONE', *, *, #82207, .F. ) ;
#66061 = EDGE_CURVE ( 'NONE', #30450, #1347, #62409, .T. ) ;
#66063 = B_SPLINE_CURVE_WITH_KNOTS ( 'NONE', 3,
 ( #48748, #79670, #10169, #13148, #74072, #14148, #75543, #76046, #91285, #52232, #82173, #20261, #43123, #5543, #12156, #20759, #4565, #59851, #35513 ),
 .UNSPECIFIED., .F., .F.,
 ( 4, 1, 1, 1, 1, 1, 1, 1, 1, 1, 1, 1, 1, 1, 1, 1, 4 ),
 ( 0.000000000000000000, 0.07560433049574548370, 0.1479650154827359954, 0.2187969985237009085, 0.2894704453213758910, 0.3597242180874983819, 0.4297077387530445769, 0.5004965198485837874, 0.5744290198679491422, 0.6139472962286710578, 0.6571552698261118319, 0.7039727697209380297, 0.7549389848168008843, 0.8097066112894878431, 0.8688329536985502921, 0.9323854739325977414, 1.000000000000000000 ),
 .UNSPECIFIED. ) ;
#66064 = ORIENTED_EDGE ( 'NONE', *, *, #20421, .T. ) ;
#66065 = CARTESIAN_POINT ( 'NONE',  ( -111.7334199135079302, -25.26981769024641267, 3.943713881720887660 ) ) ;
#66066 = CARTESIAN_POINT ( 'NONE',  ( -28.47397640525979412, -24.49582855094319811, 8.947790409070464079 ) ) ;
#66067 = CARTESIAN_POINT ( 'NONE',  ( 15.01911467442479875, -4.015204461132630520, -28.37592028203562933 ) ) ;
#66068 = CARTESIAN_POINT ( 'NONE',  ( -20.73834036848188234, 1.213307192923735345, -1.500000000000002220 ) ) ;
#66069 = CARTESIAN_POINT ( 'NONE',  ( 21.38347125639554136, -3.707035686939989638, 11.49999999999999645 ) ) ;
#66070 = VERTEX_POINT ( 'NONE', #41571 ) ;
#66071 = EDGE_CURVE ( 'NONE', #61182, #50986, #91711, .T. ) ;
#66072 = CARTESIAN_POINT ( 'NONE',  ( -52.52287095715006870, -24.64898659630367916, 1.056161002820821038 ) ) ;
#66073 = CARTESIAN_POINT ( 'NONE',  ( -115.6284389687382230, -24.15503026093916716, -0.2815557561904330486 ) ) ;
#66074 = CARTESIAN_POINT ( 'NONE',  ( -5.254942042970298210, 21.81482460008805546, -1.500000000000002220 ) ) ;
#66075 = EDGE_CURVE ( 'NONE', #83889, #8604, #28829, .T. ) ;
#66076 = DIRECTION ( 'NONE',  ( 0.000000000000000000, -0.8955258983741306578, -0.4450093991605194033 ) ) ;
#66077 = DIRECTION ( 'NONE',  ( -1.334402673828313093E-16, -0.000000000000000000, -1.000000000000000000 ) ) ;
#66078 = EDGE_LOOP ( 'NONE', ( #38311, #61430, #82869, #66685 ) ) ;
#66079 = CARTESIAN_POINT ( 'NONE',  ( 29.80070917940689412, 6.376774720514426953, 27.39560796525321607 ) ) ;
#66080 = DIRECTION ( 'NONE',  ( 0.000000000000000000, -0.9999999999976377785, -2.173523156925979128E-06 ) ) ;
#66081 = B_SPLINE_SURFACE_WITH_KNOTS ( 'NONE', 3, 3, ( 
 ( #17891, #79779, #27003, #87906 ),
 ( #49862, #33616, #34623, #10276 ),
 ( #55966, #41233, #95009, #86893 ),
 ( #63586, #1671, #72188, #64597 ),
 ( #40229, #96014, #94508, #72685 ),
 ( #11274, #9772, #56471, #95512 ),
 ( #48348, #32610, #73186, #25998 ) ),
 .UNSPECIFIED., .F., .F., .F.,
 ( 4, 3, 4 ),
 ( 4, 4 ),
 ( 0.7945040050992243641, 0.8970133687736501216, 0.9995227324480757680 ),
 ( 0.2695624968113854436, 0.2706996693028251300 ),
 .UNSPECIFIED. ) ;
#66082 = EDGE_CURVE ( 'NONE', #80731, #58107, #58816, .T. ) ;
#66083 = EDGE_LOOP ( 'NONE', ( #2057, #80867, #79034, #72558 ) ) ;
#66084 = AXIS2_PLACEMENT_3D ( 'NONE', #82194, #12679, #43643 ) ;
#66085 = EDGE_CURVE ( 'NONE', #3648, #82610, #90728, .T. ) ;
#66086 = VERTEX_POINT ( 'NONE', #45065 ) ;
#66087 = CYLINDRICAL_SURFACE ( 'NONE', #79827, 2.040000000000000036 ) ;
#66088 = ORIENTED_EDGE ( 'NONE', *, *, #69713, .T. ) ;
#66089 = CARTESIAN_POINT ( 'NONE',  ( 19.98943718749924159, -7.363913660680385220, -1.500000000000002220 ) ) ;
#66090 = ORIENTED_EDGE ( 'NONE', *, *, #48783, .T. ) ;
#66091 = CARTESIAN_POINT ( 'NONE',  ( -88.50537230221658547, -24.51314013834315375, 0.6176544820404129554 ) ) ;
#66092 = CARTESIAN_POINT ( 'NONE',  ( -0.06377455873143267340, 21.83884041771831619, -1.500000000000002220 ) ) ;
#66093 = FACE_OUTER_BOUND ( 'NONE', #89888, .T. ) ;
#66094 = CARTESIAN_POINT ( 'NONE',  ( -20.89466310375201985, -8.809181082428260368, 11.49999999999998934 ) ) ;
#66095 = CARTESIAN_POINT ( 'NONE',  ( -39.62287095715005592, -29.50247984919015209, -1.443849546365060466 ) ) ;
#66096 = PLANE ( 'NONE',  #20629 ) ;
#66097 = CARTESIAN_POINT ( 'NONE',  ( 16.32745387341675780, -14.53119815553504068, -1.500000000000002220 ) ) ;
#66098 = CARTESIAN_POINT ( 'NONE',  ( -66.62287095715009855, -24.34917612406837861, 0.1852690917426618733 ) ) ;
#66099 = ORIENTED_EDGE ( 'NONE', *, *, #3070, .F. ) ;
#66100 = ADVANCED_FACE ( 'NONE', ( #22691, #68885 ), #5986, .T. ) ;
#66101 = CARTESIAN_POINT ( 'NONE',  ( -69.62287095715005592, -24.65952944569304961, 1.056160979905697017 ) ) ;
#66102 = CARTESIAN_POINT ( 'NONE',  ( -49.06509223983938739, -25.26337459480267000, 6.860564339532760236 ) ) ;
#66103 = AXIS2_PLACEMENT_3D ( 'NONE', #71333, #78921, #1318 ) ;
#66104 = ORIENTED_EDGE ( 'NONE', *, *, #87344, .T. ) ;
#66105 = CARTESIAN_POINT ( 'NONE',  ( -90.62287095715004170, -23.48783264082478794, -1.443836473390063713 ) ) ;
#66106 = ORIENTED_EDGE ( 'NONE', *, *, #28304, .F. ) ;
#66107 = CARTESIAN_POINT ( 'NONE',  ( 30.53060340732035982, -5.168677327241859132, 8.808792533107787648 ) ) ;
#66108 = DIRECTION ( 'NONE',  ( -0.000000000000000000, -1.000000000000000000, -0.000000000000000000 ) ) ;
#66109 = CARTESIAN_POINT ( 'NONE',  ( -4.916304867406160461, -20.68799595667769964, -1.500000000000002220 ) ) ;
#66110 = FACE_OUTER_BOUND ( 'NONE', #70686, .T. ) ;
#66111 = CARTESIAN_POINT ( 'NONE',  ( -27.27594984642231069, -24.97064415668394233, 2.337720463694722195 ) ) ;
#66112 = CARTESIAN_POINT ( 'NONE',  ( -85.50395841013464349, -24.52300882791530157, 0.6510814631126307095 ) ) ;
#66113 = AXIS2_PLACEMENT_3D ( 'NONE', #4766, #29586, #43827 ) ;
#66114 = CARTESIAN_POINT ( 'NONE',  ( -68.56535840407821070, -23.48783264082477018, -1.443836473390095243 ) ) ;
#66115 = CARTESIAN_POINT ( 'NONE',  ( -44.62287095715004170, -24.33927499327853639, 9.819080762295815390 ) ) ;
#66116 = ORIENTED_EDGE ( 'NONE', *, *, #5093, .F. ) ;
#66117 = CARTESIAN_POINT ( 'NONE',  ( -0.4769873229303308038, -19.55164744950295841, 11.49999999999999645 ) ) ;
#66118 = CARTESIAN_POINT ( 'NONE',  ( -66.62287095715005592, -23.48786465467241058, 11.44779295918254647 ) ) ;
#66119 = AXIS2_PLACEMENT_3D ( 'NONE', #7369, #76377, #45955 ) ;
#66120 = CARTESIAN_POINT ( 'NONE',  ( -29.03447252004092505, -24.88235332209834993, 7.704480964116209307 ) ) ;
#66121 = ADVANCED_FACE ( 'NONE', ( #84107 ), #14590, .F. ) ;
#66122 = ORIENTED_EDGE ( 'NONE', *, *, #37976, .T. ) ;
#66123 = CARTESIAN_POINT ( 'NONE',  ( -117.5228709571501469, -24.33927499327855770, 9.819080762295802955 ) ) ;
#66124 = CARTESIAN_POINT ( 'NONE',  ( -101.9507253916653440, -25.24282061761981666, 6.236250683194342059 ) ) ;
#66125 = CARTESIAN_POINT ( 'NONE',  ( -23.59123376470063960, 5.356774720514425603, 24.50402280011862288 ) ) ;
#66126 = CARTESIAN_POINT ( 'NONE',  ( -81.43785252974821276, -25.03155984298766867, 7.210847909229809005 ) ) ;
#66127 = CARTESIAN_POINT ( 'NONE',  ( 3.778003860535555702, 19.31821889988591323, 11.49999999999998934 ) ) ;
#66128 = ORIENTED_EDGE ( 'NONE', *, *, #6946, .F. ) ;
#66129 = CARTESIAN_POINT ( 'NONE',  ( 5.514125806255895004E-17, -29.50250243563665720, 8.947779561265919668 ) ) ;
#66130 = CARTESIAN_POINT ( 'NONE',  ( 2.903846153846159517, -5.876774720514415407, 19.99999999999999289 ) ) ;
#66131 = PERSON_AND_ORGANIZATION_ROLE ( 'design_supplier' ) ;
#66132 = EDGE_CURVE ( 'NONE', #8769, #96261, #60094, .T. ) ;
#66133 = ORIENTED_EDGE ( 'NONE', *, *, #90693, .F. ) ;
#66134 = CARTESIAN_POINT ( 'NONE',  ( -54.52287095715010423, -23.95044443724992789, 10.65354141964649237 ) ) ;
#66135 = CARTESIAN_POINT ( 'NONE',  ( 16.15056352287345121, 3.622774720514426949, -27.77856273171767398 ) ) ;
#66136 = LINE ( 'NONE', #35664, #19907 ) ;
#66137 = CARTESIAN_POINT ( 'NONE',  ( -27.96875734969026084, 6.143225279485574397, 23.50402280011861933 ) ) ;
#66138 = PLANE ( 'NONE',  #54806 ) ;
#66139 = CARTESIAN_POINT ( 'NONE',  ( -102.5228709571500758, -29.50250243563736774, 8.947779886222138046 ) ) ;
#66140 = LINE ( 'NONE', #49908, #44548 ) ;
#66141 = CARTESIAN_POINT ( 'NONE',  ( 15.91301918423788919, -12.03417825965012433, -1.500000000000002220 ) ) ;
#66142 = EDGE_CURVE ( 'NONE', #76257, #71901, #80555, .T. ) ;
#66143 = CARTESIAN_POINT ( 'NONE',  ( -0.1307260668091378419, -21.35764833532042672, 11.26293215892713206 ) ) ;
#66144 = CARTESIAN_POINT ( 'NONE',  ( -4.359361796094493258, -19.42695174060331809, -1.500000000000002220 ) ) ;
#66145 = ORIENTED_EDGE ( 'NONE', *, *, #7752, .F. ) ;
#66146 = VECTOR ( 'NONE', #28258, 1000.000000000000114 ) ;
#66147 = CARTESIAN_POINT ( 'NONE',  ( -2.749999999999999112, 27.59999999999999432, 2.100000000000000089 ) ) ;
#66148 = B_SPLINE_CURVE_WITH_KNOTS ( 'NONE', 3,
 ( #26247, #34859, #40975, #42981, #10016, #57220, #50094, #27744, #96260, #88652, #81034, #42492 ),
 .UNSPECIFIED., .F., .F.,
 ( 4, 2, 2, 2, 2, 4 ),
 ( 8.673617379884034509E-19, 0.0002001096462788820726, 0.0004002192925577632778, 0.0008004385851155264471, 0.001200657877673289454, 0.001600877170231052677 ),
 .UNSPECIFIED. ) ;
#66149 =( NAMED_UNIT ( * ) PLANE_ANGLE_UNIT ( ) SI_UNIT ( $, .RADIAN. ) );
#66150 = CARTESIAN_POINT ( 'NONE',  ( -23.31187512739357359, 6.376774720514425177, -17.31005501743528541 ) ) ;
#66151 = CARTESIAN_POINT ( 'NONE',  ( 10.68713020350585197, -3.316774720514176877, -28.05292731652309257 ) ) ;
#66152 = CARTESIAN_POINT ( 'NONE',  ( -105.6228709571500559, -29.50247984919015209, -1.443849546365048253 ) ) ;
#66153 = DIRECTION ( 'NONE',  ( 0.000000000000000000, -1.000000000000000000, 0.000000000000000000 ) ) ;
#66154 = CC_DESIGN_PERSON_AND_ORGANIZATION_ASSIGNMENT ( #18562, #57647, ( #96129 ) ) ;
#66155 = LINE ( 'NONE', #57033, #6440 ) ;
#66156 = ORIENTED_EDGE ( 'NONE', *, *, #37545, .F. ) ;
#66157 = B_SPLINE_SURFACE_WITH_KNOTS ( 'NONE', 3, 3, ( 
 ( #70157, #47327, #39198, #55443 ),
 ( #32088, #78250, #70661, #17370 ),
 ( #62054, #25481, #77248, #1151 ),
 ( #1655, #63570, #640, #63063 ),
 ( #92980, #62554, #93986, #94491 ),
 ( #94991, #87380, #48333, #23454 ),
 ( #31589, #24974, #56455, #24476 ) ),
 .UNSPECIFIED., .F., .F., .F.,
 ( 4, 3, 4 ),
 ( 4, 4 ),
 ( 0.7945040050992243641, 0.8970133687736505657, 0.9995227324480766562 ),
 ( 0.8297048367401780311, 0.8311006081063124773 ),
 .UNSPECIFIED. ) ;
#66158 = CARTESIAN_POINT ( 'NONE',  ( -62.62287095715003460, -23.72747288104441665, -1.053458166803662888 ) ) ;
#66159 = CARTESIAN_POINT ( 'NONE',  ( -65.52287095715006160, -29.50247984919015209, -1.443849546365055359 ) ) ;
#66160 = ORIENTED_EDGE ( 'NONE', *, *, #48783, .F. ) ;
#66161 = CARTESIAN_POINT ( 'NONE',  ( -6.993686169601437186, 18.98418669460116348, 11.49999999999998934 ) ) ;
#66162 = B_SPLINE_CURVE_WITH_KNOTS ( 'NONE', 3,
 ( #86837, #64544, #87851, #41179 ),
 .UNSPECIFIED., .F., .F.,
 ( 4, 4 ),
 ( 0.1488646418289148732, 0.1498653888696803438 ),
 .UNSPECIFIED. ) ;
#66163 = CARTESIAN_POINT ( 'NONE',  ( 6.420673076923079314, -6.376774720514427841, 21.83974358974358765 ) ) ;
#66164 = CARTESIAN_POINT ( 'NONE',  ( 15.08554537508427629, 5.152774720514429418, -26.79085230644757232 ) ) ;
#66165 = TOROIDAL_SURFACE ( 'NONE', #11033, 25.90800000000000125, 2.040000000000000036 ) ;
#66166 = DIRECTION ( 'NONE',  ( -3.773278334453079030E-23, 0.9999999999976377785, 2.173523156925979128E-06 ) ) ;
#66167 = ORIENTED_EDGE ( 'NONE', *, *, #40054, .T. ) ;
#66168 = CARTESIAN_POINT ( 'NONE',  ( -79.37676797629123371, -25.29665582273151614, 5.684420612865764610 ) ) ;
#66169 = CARTESIAN_POINT ( 'NONE',  ( -1.836964591723098117, -5.876774720514409189, 19.23384392940399223 ) ) ;
#66170 = CARTESIAN_POINT ( 'NONE',  ( -13.75281105048956576, 14.62798779934380811, -1.500000000000002220 ) ) ;
#66171 = CARTESIAN_POINT ( 'NONE',  ( 20.15827220212406701, 6.050813824765241655, 11.49999999999999645 ) ) ;
#66172 = CARTESIAN_POINT ( 'NONE',  ( -48.87380231474225667, -29.50249632652208476, 6.137082770844160429 ) ) ;
#66173 = CARTESIAN_POINT ( 'NONE',  ( -70.59772795895749198, -24.15602025860896518, 10.28564288303534724 ) ) ;
#66174 = CARTESIAN_POINT ( 'NONE',  ( -14.46940225681120396, -16.66540133702554272, 11.49999999999998934 ) ) ;
#66175 = AXIS2_PLACEMENT_3D ( 'NONE', #40601, #2045, #64963 ) ;
#66176 = CARTESIAN_POINT ( 'NONE',  ( -39.51244657141699435, -25.27805987054186687, 4.531907366321720865 ) ) ;
#66177 = LINE ( 'NONE', #44320, #11158 ) ;
#66178 = CARTESIAN_POINT ( 'NONE',  ( -64.58953762381673869, -23.47596703998600276, 11.44779298504227505 ) ) ;
#66179 = ORIENTED_EDGE ( 'NONE', *, *, #86875, .F. ) ;
#66180 = CARTESIAN_POINT ( 'NONE',  ( -72.49894236110185375, -24.51314013834316796, 0.6176544820404143987 ) ) ;
#66181 = DIRECTION ( 'NONE',  ( 0.9975640502598241977, -0.06975647374412546897, -0.000000000000000000 ) ) ;
#66182 = EDGE_LOOP ( 'NONE', ( #44108, #77728, #16594, #43161 ) ) ;
#66183 = CIRCLE ( 'NONE', #22384, 252.4458649670781085 ) ;
#66184 = ORIENTED_EDGE ( 'NONE', *, *, #76159, .T. ) ;
#66185 = FACE_OUTER_BOUND ( 'NONE', #33121, .T. ) ;
#66186 = CARTESIAN_POINT ( 'NONE',  ( -72.58953762381671027, -23.48786465467241058, 11.44779295918254647 ) ) ;
#66187 = CARTESIAN_POINT ( 'NONE',  ( -76.60092789896461341, -23.73766607897670866, -1.055555164236452681 ) ) ;
#66188 = CARTESIAN_POINT ( 'NONE',  ( 17.30552477474510908, -11.17933342135444086, -1.500000000000002220 ) ) ;
#66189 = CARTESIAN_POINT ( 'NONE',  ( -0.8555947871142663974, 21.52075748220454798, 11.49999999999999645 ) ) ;
#66190 = EDGE_LOOP ( 'NONE', ( #30831, #58933, #4996, #69503 ) ) ;
#66191 = CYLINDRICAL_SURFACE ( 'NONE', #4036, 0.8500000000000017542 ) ;
#66192 = DIRECTION ( 'NONE',  ( 0.000000000000000000, 1.478457507934778393E-16, -1.000000000000000000 ) ) ;
#66193 = CARTESIAN_POINT ( 'NONE',  ( 0.3910256410256418014, -6.376774720514418959, 20.67377804487179915 ) ) ;
#66194 = CARTESIAN_POINT ( 'NONE',  ( 4.697571063781373013, 21.84268702631108994, -1.500000000000002220 ) ) ;
#66195 = CYLINDRICAL_SURFACE ( 'NONE', #5926, 0.3000000000000016542 ) ;
#66196 = CARTESIAN_POINT ( 'NONE',  ( -124.6228709571500701, -24.34917612406838927, 0.1852690917426691730 ) ) ;
#66197 = ORIENTED_EDGE ( 'NONE', *, *, #6823, .T. ) ;
#66198 = CARTESIAN_POINT ( 'NONE',  ( 31.84105487026622683, 3.622774720514426949, -11.95870468328481984 ) ) ;
#66199 = CARTESIAN_POINT ( 'NONE',  ( 3.063121397228215859, -5.876774720514420736, 20.95210102656095685 ) ) ;
#66200 = EDGE_CURVE ( 'NONE', #69513, #77700, #45229, .T. ) ;
#66201 = CARTESIAN_POINT ( 'NONE',  ( 20.57277012135545036, 3.371850554975475145, -1.500000000000002220 ) ) ;
#66202 = EDGE_CURVE ( 'NONE', #21579, #80276, #38436, .T. ) ;
#66203 = ORIENTED_EDGE ( 'NONE', *, *, #21354, .F. ) ;
#66205 = ORIENTED_EDGE ( 'NONE', *, *, #83242, .F. ) ;
#66204 = CARTESIAN_POINT ( 'NONE',  ( 30.53060340732035982, -1.682774720514426114, -1.272392034746785860 ) ) ;
#66206 = EDGE_LOOP ( 'NONE', ( #87625, #55763, #25129, #82396 ) ) ;
#66207 = CARTESIAN_POINT ( 'NONE',  ( -100.5044678508139810, -25.00182538069147142, 7.747789668545045139 ) ) ;
#66208 = CARTESIAN_POINT ( 'NONE',  ( 11.07546443054301655, -17.96822238807187233, -1.500000000000002220 ) ) ;
#66209 = VERTEX_POINT ( 'NONE', #5487 ) ;
#66210 = CARTESIAN_POINT ( 'NONE',  ( -53.62287095715005592, -29.50248528299804818, 1.056150453629033370 ) ) ;
#66211 = CARTESIAN_POINT ( 'NONE',  ( -110.6228709571500559, -24.99132157543166954, 2.256160258750667502 ) ) ;
#66212 = CARTESIAN_POINT ( 'NONE',  ( -129.5228709571500758, -23.48786465467242479, 11.44779295918253581 ) ) ;
#66213 = FACE_OUTER_BOUND ( 'NONE', #43498, .T. ) ;
#66214 = DIRECTION ( 'NONE',  ( -0.9890158633619158257, -0.1478094111296165414, -0.000000000000000000 ) ) ;
#66215 = CARTESIAN_POINT ( 'NONE',  ( -2.129050106866105185, 21.58297100922832357, -1.500000000000002220 ) ) ;
#66216 = CARTESIAN_POINT ( 'NONE',  ( -63.52287095715003318, -23.73934037231756022, 11.05740245334328797 ) ) ;
#66218 = ORIENTED_EDGE ( 'NONE', *, *, #99973, .T. ) ;
#66217 = CARTESIAN_POINT ( 'NONE',  ( -19.03210976516136554, 11.49075778266564107, 11.49999999999999645 ) ) ;
#66219 = EDGE_CURVE ( 'NONE', #41736, #53720, #27366, .T. ) ;
#66220 = CARTESIAN_POINT ( 'NONE',  ( -50.61185169649064619, -25.31441726102578116, 5.215440883357011614 ) ) ;
#66221 = CARTESIAN_POINT ( 'NONE',  ( 14.61581677259038692, 3.466180823938291855, -27.35847992067005308 ) ) ;
#66222 = DIRECTION ( 'NONE',  ( -1.000000000000000000, 0.000000000000000000, 0.000000000000000000 ) ) ;
#66223 = VERTEX_POINT ( 'NONE', #69389 ) ;
#66225 = EDGE_LOOP ( 'NONE', ( #99454, #69123, #4074, #82591 ) ) ;
#66224 = LINE ( 'NONE', #97145, #19926 ) ;
#66226 = ORIENTED_EDGE ( 'NONE', *, *, #39662, .T. ) ;
#66227 = CARTESIAN_POINT ( 'NONE',  ( -101.1409834047034906, -25.16687399051181018, 6.899440319863159310 ) ) ;
#66228 = CARTESIAN_POINT ( 'NONE',  ( -108.8968792378192063, -25.15277794460069316, 6.986250878905963191 ) ) ;
#66229 = CARTESIAN_POINT ( 'NONE',  ( -43.62287095715002749, -24.33927499327853639, 9.819080762295822495 ) ) ;
#66230 = CARTESIAN_POINT ( 'NONE',  ( 8.971512145086503409, -1.028487854913504362, -6.500000000000000000 ) ) ;
#66231 = CARTESIAN_POINT ( 'NONE',  ( -10.24059822343757808, -5.876774720514426953, 22.08128695274315945 ) ) ;
#66232 = ORIENTED_EDGE ( 'NONE', *, *, #46228, .T. ) ;
#66233 = CARTESIAN_POINT ( 'NONE',  ( -19.23900614489824079, 2.250179475969715348, 11.49999999999999645 ) ) ;
#66234 = DIRECTION ( 'NONE',  ( 0.000000000000000000, 0.000000000000000000, -1.000000000000000000 ) ) ;
#66235 = CARTESIAN_POINT ( 'NONE',  ( 22.31695869535024102, -2.478243017838637652, -1.500000000000002220 ) ) ;
#66236 = ORIENTED_EDGE ( 'NONE', *, *, #55333, .F. ) ;
#66237 = CARTESIAN_POINT ( 'NONE',  ( -101.6292210487389269, -24.15620529776628800, 10.23563542870660292 ) ) ;
#66238 = LINE ( 'NONE', #5306, #47448 ) ;
#66239 = CARTESIAN_POINT ( 'NONE',  ( -116.5228709571500474, -23.94994826722564696, -0.6494450866342714734 ) ) ;
#66240 = VECTOR ( 'NONE', #34920, 1000.000000000000000 ) ;
#66241 = CARTESIAN_POINT ( 'NONE',  ( -63.92537901004148893, -24.57143472585066490, 0.8294870405985537154 ) ) ;
#66242 = EDGE_CURVE ( 'NONE', #40322, #26067, #30661, .T. ) ;
#66243 = CARTESIAN_POINT ( 'NONE',  ( 16.73968668634701729, 10.17700309559984717, 11.49999999999998934 ) ) ;
#66244 = CARTESIAN_POINT ( 'NONE',  ( -46.54049122901287916, -24.34968618360933235, 0.1864209137778778391 ) ) ;
#66245 = ORIENTED_EDGE ( 'NONE', *, *, #61716, .F. ) ;
#66246 = CARTESIAN_POINT ( 'NONE',  ( -21.46803524902295024, 1.580295693706654347, -1.500000000000002220 ) ) ;
#66247 = CARTESIAN_POINT ( 'NONE',  ( -129.5228709571500758, -24.64965694238408034, 8.947790433994189385 ) ) ;
#66248 = CARTESIAN_POINT ( 'NONE',  ( -80.64958649024407578, -25.31572648974913164, 4.980655863047315890 ) ) ;
#66249 = DIRECTION ( 'NONE',  ( -1.000000000000000000, -3.773278334444166432E-23, -8.201307841325785021E-29 ) ) ;
#66250 = DIRECTION ( 'NONE',  ( -3.773278334453079030E-23, 0.9999999999976377785, 2.173523156925979128E-06 ) ) ;
#66251 = CARTESIAN_POINT ( 'NONE',  ( 8.272623322502495213, 21.45567517505680044, -1.500000000000002220 ) ) ;
#66252 = EDGE_CURVE ( 'NONE', #87707, #43715, #6326, .T. ) ;
#66253 = B_SPLINE_CURVE_WITH_KNOTS ( 'NONE', 3,
 ( #2870, #81481, #95699, #79471, #27694, #88098 ),
 .UNSPECIFIED., .F., .F.,
 ( 4, 2, 4 ),
 ( 6.391158118975501388E-06, 0.001387004593080795036, 0.002767618028042614572 ),
 .UNSPECIFIED. ) ;
#66254 = PERSON_AND_ORGANIZATION ( #70597, #27821 ) ;
#66255 = LINE ( 'NONE', #93538, #98498 ) ;
#66256 = CARTESIAN_POINT ( 'NONE',  ( -49.62828767225136062, -24.51314013834316086, 0.6176544820404115121 ) ) ;
#66257 = CARTESIAN_POINT ( 'NONE',  ( -14.05898297266747221, -14.31596314050798568, 11.49999999999999645 ) ) ;
#66258 = CARTESIAN_POINT ( 'NONE',  ( -108.9545715455115129, -25.10927687032588906, 4.170145204219119606 ) ) ;
#66259 = CARTESIAN_POINT ( 'NONE',  ( -31.52287095715004739, -23.48783264083373723, -1.443836473376154617 ) ) ;
#66260 = AXIS2_PLACEMENT_3D ( 'NONE', #87212, #475, #8596 ) ;
#66261 = CARTESIAN_POINT ( 'NONE',  ( -4.213970605900704491, -5.876774720514416295, 20.02963804100705758 ) ) ;
#66262 = DIRECTION ( 'NONE',  ( 0.000000000000000000, 1.000000000000000000, 0.000000000000000000 ) ) ;
#66263 = CARTESIAN_POINT ( 'NONE',  ( -95.62287095715005592, -23.47596703998600631, 11.44779298504227860 ) ) ;
#66264 = CARTESIAN_POINT ( 'NONE',  ( -13.97081141688431138, 14.13901428111770819, 11.49999999999998934 ) ) ;
#66265 = CARTESIAN_POINT ( 'NONE',  ( -109.5228709571500616, -24.64898659630530275, 1.056161002820831474 ) ) ;
#66266 = CARTESIAN_POINT ( 'NONE',  ( 17.05426814964238957, 9.943002105365778220, -1.500000000000002220 ) ) ;
#66267 = DIRECTION ( 'NONE',  ( -0.06486421869277853025, 0.000000000000000000, 0.9978940991575084851 ) ) ;
#66268 = CARTESIAN_POINT ( 'NONE',  ( -110.5228709571501184, -24.91570333825771755, 8.075032458260348989 ) ) ;
#66269 = DIRECTION ( 'NONE',  ( 0.000000000000000000, 0.000000000000000000, -1.000000000000000000 ) ) ;
#66270 = CARTESIAN_POINT ( 'NONE',  ( 20.45670835789597319, 2.398913822417158226, 11.49999999999999645 ) ) ;
#66271 = ADVANCED_FACE ( 'NONE', ( #68394 ), #84609, .F. ) ;
#66272 = CARTESIAN_POINT ( 'NONE',  ( 22.81105451610979173, -1.475225279485572916, -18.46691820600746681 ) ) ;
#66273 = CARTESIAN_POINT ( 'NONE',  ( 16.59953334139655468, -15.42474913338910980, 11.49999999999999645 ) ) ;
#66274 = ORIENTED_EDGE ( 'NONE', *, *, #24573, .F. ) ;
#66275 = CARTESIAN_POINT ( 'NONE',  ( -62.52287095715006160, -24.64965694238406613, 8.947790433994201820 ) ) ;
#66276 = LINE ( 'NONE', #74362, #85706 ) ;
#66277 = CARTESIAN_POINT ( 'NONE',  ( -110.5228709571500332, -24.92579138211018730, 1.929029949965659352 ) ) ;
#66278 = CARTESIAN_POINT ( 'NONE',  ( 26.37445894957760473, 1.477225279485574028, -11.69480419648520986 ) ) ;
#66279 = EDGE_CURVE ( 'NONE', #37096, #100315, #30943, .T. ) ;
#66280 = ORIENTED_EDGE ( 'NONE', *, *, #26170, .T. ) ;
#66281 = ORIENTED_EDGE ( 'NONE', *, *, #14774, .F. ) ;
#66282 = LINE ( 'NONE', #82967, #30633 ) ;
#66283 = CARTESIAN_POINT ( 'NONE',  ( -21.29394331855728240, -8.360804490491451801, 11.49999999999998934 ) ) ;
#66284 = CARTESIAN_POINT ( 'NONE',  ( -74.62287095715005592, -24.65952944569304606, 1.056160979905696351 ) ) ;
#66285 = CARTESIAN_POINT ( 'NONE',  ( 15.64208908530913256, 14.88810259432246852, -1.500000000000002220 ) ) ;
#66286 = PLANE ( 'NONE',  #44719 ) ;
#66287 = CARTESIAN_POINT ( 'NONE',  ( -65.52287095715004739, -23.85196035786901092, -0.8779234886475200117 ) ) ;
#66288 = CARTESIAN_POINT ( 'NONE',  ( -0.06565682164858396841, -22.51586213336150166, 11.49999999999999645 ) ) ;
#66289 = VERTEX_POINT ( 'NONE', #29821 ) ;
#66290 = CARTESIAN_POINT ( 'NONE',  ( -86.62287095715004170, -23.47593901973091235, -1.443836447539002865 ) ) ;
#66291 = CARTESIAN_POINT ( 'NONE',  ( -18.27885182143903720, 12.20952002138517045, 11.49999999999998934 ) ) ;
#66292 = CARTESIAN_POINT ( 'NONE',  ( -111.5222191420114370, -23.48783264082477018, -1.443836473390086805 ) ) ;
#66293 = LINE ( 'NONE', #43449, #76196 ) ;
#66294 = ORIENTED_EDGE ( 'NONE', *, *, #31083, .T. ) ;
#66295 = DIRECTION ( 'NONE',  ( 0.000000000000000000, 0.9999999999976377785, 2.173523156925979975E-06 ) ) ;
#66296 = DIRECTION ( 'NONE',  ( 0.000000000000000000, -1.000000000000000000, 0.000000000000000000 ) ) ;
#66297 = EDGE_LOOP ( 'NONE', ( #47874, #43244, #3643, #4661 ) ) ;
#66298 = DIRECTION ( 'NONE',  ( -2.682707457723910108E-15, 0.000000000000000000, -1.000000000000000000 ) ) ;
#66299 = CIRCLE ( 'NONE', #48472, 6.119803529381341534 ) ;
#66300 = EDGE_LOOP ( 'NONE', ( #84240, #79129, #96385, #46696 ) ) ;
#66301 = VECTOR ( 'NONE', #56043, 999.9999999999998863 ) ;
#66302 = ORIENTED_EDGE ( 'NONE', *, *, #13972, .T. ) ;
#66303 = EDGE_CURVE ( 'NONE', #84371, #1776, #69889, .T. ) ;
#66304 = ORIENTED_EDGE ( 'NONE', *, *, #81869, .F. ) ;
#66305 = EDGE_CURVE ( 'NONE', #36107, #13848, #16384, .T. ) ;
#66306 = LINE ( 'NONE', #75377, #79372 ) ;
#66307 = CARTESIAN_POINT ( 'NONE',  ( -115.5228709571500616, -29.50248528299804818, 1.056150453629045360 ) ) ;
#66308 = CARTESIAN_POINT ( 'NONE',  ( 14.75122623597950700, 4.701663563191169182, -27.79036425924726217 ) ) ;
#66309 = CARTESIAN_POINT ( 'NONE',  ( -14.48729221511043441, 14.40292172154154926, -1.500000000000002220 ) ) ;
#66310 = EDGE_LOOP ( 'NONE', ( #93354, #66950, #47974, #24127 ) ) ;
#66311 = DIRECTION ( 'NONE',  ( 0.000000000000000000, 0.000000000000000000, 1.000000000000000000 ) ) ;
#66312 = AXIS2_PLACEMENT_3D ( 'NONE', #80018, #83503, #43467 ) ;
#66313 = CARTESIAN_POINT ( 'NONE',  ( -51.61964320672224460, -25.23391071228556370, 3.593176832712704716 ) ) ;
#66314 = CARTESIAN_POINT ( 'NONE',  ( -105.5221828617972619, -23.48783264082477018, -1.443836473390094355 ) ) ;
#66315 = CARTESIAN_POINT ( 'NONE',  ( -71.31671495077925726, -25.03149765108591751, 7.173522054403384196 ) ) ;
#66316 = VERTEX_POINT ( 'NONE', #8492 ) ;
#66317 = CARTESIAN_POINT ( 'NONE',  ( -28.94548163072471425, -24.76881035311403423, 3.108274031987006136 ) ) ;
#66318 = CARTESIAN_POINT ( 'NONE',  ( -27.85310238079214784, -25.26248076281864741, 8.249330725495340744 ) ) ;
#66319 = ORIENTED_EDGE ( 'NONE', *, *, #12471, .T. ) ;
#66320 = AXIS2_PLACEMENT_3D ( 'NONE', #94575, #25057, #72757 ) ;
#66321 = CARTESIAN_POINT ( 'NONE',  ( -16.26442346200556344, 12.93145763113255775, 11.49999999999998934 ) ) ;
#66322 = EDGE_CURVE ( 'NONE', #70795, #6012, #84110, .T. ) ;
#66323 = ORIENTED_EDGE ( 'NONE', *, *, #81691, .F. ) ;
#66325 = ORIENTED_EDGE ( 'NONE', *, *, #52356, .F. ) ;
#66324 = CARTESIAN_POINT ( 'NONE',  ( -40.17256793773198353, -25.30544673913221487, 5.061440930064124544 ) ) ;
#66326 = ADVANCED_FACE ( 'NONE', ( #23198 ), #8985, .T. ) ;
#66327 = CARTESIAN_POINT ( 'NONE',  ( -29.49875734969026198, 5.965225279485572685, 0.1180228001186258285 ) ) ;
#66328 = DIRECTION ( 'NONE',  ( 3.491481338843133355E-15, -1.000000000000000000, 2.352173255807804438E-16 ) ) ;
#66329 = VERTEX_POINT ( 'NONE', #78990 ) ;
#66330 = ORIENTED_EDGE ( 'NONE', *, *, #19452, .T. ) ;
#66331 = CARTESIAN_POINT ( 'NONE',  ( -33.52287095715006160, -24.50321055353803956, 9.387540953477525818 ) ) ;
#66332 = AXIS2_PLACEMENT_3D ( 'NONE', #64927, #34944, #49686 ) ;
#66333 = CARTESIAN_POINT ( 'NONE',  ( -116.6228709571500417, -24.66019654487199730, 8.947790411086121054 ) ) ;
#66334 = CARTESIAN_POINT ( 'NONE',  ( -113.5895376238167245, -23.47593901973091235, -1.443836447538999312 ) ) ;
#66335 = CARTESIAN_POINT ( 'NONE',  ( -71.26908920811321480, -25.24515179469667814, 5.945032366209153984 ) ) ;
#66337 = ORIENTED_EDGE ( 'NONE', *, *, #86197, .F. ) ;
#66336 = CARTESIAN_POINT ( 'NONE',  ( 22.05266032001784637, -1.487345182339283367, 11.49999999999999645 ) ) ;
#66338 = EDGE_CURVE ( 'NONE', #49051, #66356, #62802, .T. ) ;
#66339 = CARTESIAN_POINT ( 'NONE',  ( -72.62287095715009855, -24.34917612406838217, 0.1852690917426622341 ) ) ;
#66340 = CARTESIAN_POINT ( 'NONE',  ( 21.71239400539012721, -6.292901409244172406, -1.500000000000002220 ) ) ;
#66341 = EDGE_CURVE ( 'NONE', #85588, #17471, #39938, .T. ) ;
#66343 = ORIENTED_EDGE ( 'NONE', *, *, #74495, .T. ) ;
#66342 = CARTESIAN_POINT ( 'NONE',  ( -99.55486036248895232, -25.30557962015589979, 4.972970070441952828 ) ) ;
#66344 = B_SPLINE_CURVE_WITH_KNOTS ( 'NONE', 3,
 ( #59679, #20095, #34835, #50065 ),
 .UNSPECIFIED., .F., .F.,
 ( 4, 4 ),
 ( 0.000000000000000000, 9.999999999998897304E-05 ),
 .UNSPECIFIED. ) ;
#66345 = ORIENTED_EDGE ( 'NONE', *, *, #1955, .F. ) ;
#66346 = CARTESIAN_POINT ( 'NONE',  ( -80.51775687497260492, -25.31554036629395554, 4.968850436570557250 ) ) ;
#66347 = AXIS2_PLACEMENT_3D ( 'NONE', #6199, #97551, #43777 ) ;
#66348 = B_SPLINE_SURFACE_WITH_KNOTS ( 'NONE', 3, 1, ( 
 ( #43124, #88804 ),
 ( #81683, #42636 ),
 ( #10672, #33504 ),
 ( #64490, #42142 ),
 ( #74073, #27398 ),
 ( #73574, #25893 ),
 ( #80181, #34012 ),
 ( #26397, #56866 ),
 ( #87797, #57369 ),
 ( #18770, #41634 ),
 ( #19269, #50240 ),
 ( #81180, #11658 ),
 ( #4062, #35007 ),
 ( #65987, #96904 ),
 ( #89294, #19763 ),
 ( #50739, #37501 ),
 ( #5051, #66972 ),
 ( #83164, #37000 ),
 ( #68454, #99391 ) ),
 .UNSPECIFIED., .F., .F., .F.,
 ( 4, 1, 1, 1, 1, 1, 1, 1, 1, 1, 1, 1, 1, 1, 1, 1, 4 ),
 ( 2, 2 ),
 ( 0.000000000000000000, 0.06629491280198847314, 0.1301311164811693732, 0.1928622251726082593, 0.2543600042042246101, 0.3159098460813289933, 0.3773381393463554612, 0.4402052628879283280, 0.5041751317708966784, 0.5680336324132717607, 0.6302277217668702525, 0.6908614774070669373, 0.7514218176484559475, 0.8114657367408623090, 0.8727504667961283324, 0.9353907348444668868, 1.000000000000000000 ),
 ( 0.000000000000000000, 1.000000000000000000 ),
 .UNSPECIFIED. ) ;
#66349 = CARTESIAN_POINT ( 'NONE',  ( -78.62287095715007013, -23.95044443724992078, 10.65354141964649237 ) ) ;
#66350 = ORIENTED_EDGE ( 'NONE', *, *, #11572, .T. ) ;
#66351 = CARTESIAN_POINT ( 'NONE',  ( -21.15187133135857422, -0.9709546189074961253, 11.49999999999998934 ) ) ;
#66352 = CARTESIAN_POINT ( 'NONE',  ( -49.62287095715005592, -29.50250243563736774, 8.947779886222146928 ) ) ;
#66353 = DIRECTION ( 'NONE',  ( 0.1478094111296165691, -0.9890158633619158257, -6.377659838150018832E-17 ) ) ;
#66354 = CARTESIAN_POINT ( 'NONE',  ( 22.30035941410032763, -0.3387204123245128873, -1.500000000000002220 ) ) ;
#66355 = DIRECTION ( 'NONE',  ( 0.000000000000000000, 0.000000000000000000, 1.000000000000000000 ) ) ;
#66356 = VERTEX_POINT ( 'NONE', #40449 ) ;
#66357 = CARTESIAN_POINT ( 'NONE',  ( -5.238752036864926964, -6.376774720514410077, 19.51517878119694061 ) ) ;
#66358 = CARTESIAN_POINT ( 'NONE',  ( 0.000000000000000000, 1.477225279485574028, 19.84760796525321425 ) ) ;
#66359 = DIRECTION ( 'NONE',  ( 0.6599726524652350657, 0.000000000000000000, -0.7512896232465892110 ) ) ;
#66360 = CARTESIAN_POINT ( 'NONE',  ( -83.62287095715005592, -24.64965695001468404, 8.947790433994182280 ) ) ;
#66361 = CARTESIAN_POINT ( 'NONE',  ( -3.338044803349280443, -19.22079736023769669, -1.500000000000002220 ) ) ;
#66362 = CARTESIAN_POINT ( 'NONE',  ( -13.24026558610970916, 16.85365899302435722, 11.49999999999998934 ) ) ;
#66363 = CARTESIAN_POINT ( 'NONE',  ( -0.5830141525297981575, -6.376774720514411854, 19.15054976246387497 ) ) ;
#66364 = DIRECTION ( 'NONE',  ( 3.773278334444167608E-23, -1.000000000000000000, 0.000000000000000000 ) ) ;
#66365 = PLANE ( 'NONE',  #97643 ) ;
#66366 = CARTESIAN_POINT ( 'NONE',  ( 7.682656365740156090, -21.48159684637525046, -1.500000000000002220 ) ) ;
#66367 = EDGE_CURVE ( 'NONE', #55585, #15484, #7985, .T. ) ;
#66368 = PERSON_AND_ORGANIZATION ( #70597, #27821 ) ;
#66369 = CARTESIAN_POINT ( 'NONE',  ( -106.5551925487616671, -23.96169478059714564, 10.65365249895717170 ) ) ;
#66370 = CARTESIAN_POINT ( 'NONE',  ( -128.5228709571500758, -23.94994826722564696, -0.6494450866342721396 ) ) ;
#66371 = CARTESIAN_POINT ( 'NONE',  ( -13.68957358570155769, -14.46295258127404892, 11.49999999999999645 ) ) ;
#66372 = FACE_OUTER_BOUND ( 'NONE', #55803, .T. ) ;
#66373 = AXIS2_PLACEMENT_3D ( 'NONE', #52730, #12658, #30382 ) ;
#66374 = CARTESIAN_POINT ( 'NONE',  ( -39.64153524556972741, -24.15620529776628089, 10.23563542870661180 ) ) ;
#66375 = CARTESIAN_POINT ( 'NONE',  ( -98.58953762381672448, -23.47593901973091235, -1.443836447539001089 ) ) ;
#66376 = EDGE_LOOP ( 'NONE', ( #26618, #41631, #24980, #59462 ) ) ;
#66377 = B_SPLINE_CURVE_WITH_KNOTS ( 'NONE', 3,
 ( #92300, #30400, #21774, #5569 ),
 .UNSPECIFIED., .F., .F.,
 ( 4, 4 ),
 ( 0.000000000000000000, 9.999999999998900014E-05 ),
 .UNSPECIFIED. ) ;
#66378 = FACE_OUTER_BOUND ( 'NONE', #23390, .T. ) ;
#66379 = CARTESIAN_POINT ( 'NONE',  ( -32.42024351695030759, -24.87479601683088148, 8.247789944647561100 ) ) ;
#66380 = CARTESIAN_POINT ( 'NONE',  ( 21.38347125639554136, -3.707035686939989638, 11.49999999999998934 ) ) ;
#66381 = LINE ( 'NONE', #97310, #65890 ) ;
#66382 = AXIS2_PLACEMENT_3D ( 'NONE', #49231, #80159, #25366 ) ;
#66383 = CARTESIAN_POINT ( 'NONE',  ( 16.94836550497923966, -9.742303593519430649, -1.500000000000002220 ) ) ;
#66384 = DIRECTION ( 'NONE',  ( 0.000000000000000000, 0.000000000000000000, -1.000000000000000000 ) ) ;
#66386 = ORIENTED_EDGE ( 'NONE', *, *, #81764, .T. ) ;
#66385 = VECTOR ( 'NONE', #70516, 1000.000000000000000 ) ;
#66387 = PERSON_AND_ORGANIZATION ( #70597, #27821 ) ;
#66388 = VECTOR ( 'NONE', #20313, 1000.000000000000000 ) ;
#66389 = CARTESIAN_POINT ( 'NONE',  ( -69.62287095715009855, -24.33927499327854704, 9.819080762295822495 ) ) ;
#66390 = CARTESIAN_POINT ( 'NONE',  ( -12.74120943341865342, -16.01528480738631899, 11.49999999999999645 ) ) ;
#66391 = CARTESIAN_POINT ( 'NONE',  ( 13.82660648177921914, -6.475225279485573360, -27.21585177491302332 ) ) ;
#66392 = B_SPLINE_CURVE_WITH_KNOTS ( 'NONE', 3,
 ( #66412, #90718, #13078, #97332, #65914, #21192, #27820, #58774, #98819, #5976, #75974, #52158, #98315, #89726 ),
 .UNSPECIFIED., .F., .F.,
 ( 4, 2, 2, 2, 2, 2, 4 ),
 ( 7.059813062317230268E-18, 0.0003111425035767722246, 0.0006222850071535374018, 0.0007778562589419200446, 0.0009334275107303025790, 0.001088998762518685222, 0.001244570014307067865 ),
 .UNSPECIFIED. ) ;
#66393 = CARTESIAN_POINT ( 'NONE',  ( -86.58953762381672448, -24.64965694238406968, 8.947790433994656567 ) ) ;
#66394 = EDGE_CURVE ( 'NONE', #38489, #21579, #46253, .T. ) ;
#66395 = AXIS2_PLACEMENT_3D ( 'NONE', #25999, #48350, #63078 ) ;
#66396 = ORIENTED_EDGE ( 'NONE', *, *, #91821, .T. ) ;
#66397 = CARTESIAN_POINT ( 'NONE',  ( 1.999999999999998224, 0.000000000000000000, 0.000000000000000000 ) ) ;
#66398 = CARTESIAN_POINT ( 'NONE',  ( 33.61456970919608978, 3.316774720514426900, -11.35828564741662738 ) ) ;
#66399 = CARTESIAN_POINT ( 'NONE',  ( -10.34999999999999254, 4.999999999999999112, 2.100000000000000089 ) ) ;
#66400 = EDGE_CURVE ( 'NONE', #25949, #58927, #25170, .T. ) ;
#66401 = DIRECTION ( 'NONE',  ( -0.000000000000000000, -1.000000000000000000, -0.000000000000000000 ) ) ;
#66402 = ORIENTED_EDGE ( 'NONE', *, *, #74230, .T. ) ;
#66403 = ADVANCED_FACE ( 'NONE', ( #70390 ), #86111, .F. ) ;
#66404 = CARTESIAN_POINT ( 'NONE',  ( 5.654871928786437074, -6.376774720514420736, 20.64717925217163952 ) ) ;
#66405 = EDGE_CURVE ( 'NONE', #20944, #63660, #32326, .T. ) ;
#66406 = EDGE_CURVE ( 'NONE', #8499, #15369, #64961, .T. ) ;
#66407 = B_SPLINE_CURVE_WITH_KNOTS ( 'NONE', 3,
 ( #77941, #47024, #7948, #30791 ),
 .UNSPECIFIED., .F., .F.,
 ( 4, 4 ),
 ( 0.000000000000000000, 9.999999999998206125E-05 ),
 .UNSPECIFIED. ) ;
#66408 = CARTESIAN_POINT ( 'NONE',  ( 17.37538969058663696, -15.08583811485692117, 11.49999999999999645 ) ) ;
#66409 = CARTESIAN_POINT ( 'NONE',  ( -16.34568771794417685, -15.85656593008108750, -1.500000000000002220 ) ) ;
#66410 = CARTESIAN_POINT ( 'NONE',  ( -110.5570691414250746, -23.85049219812686161, 10.88485053497526778 ) ) ;
#66411 = PLANE ( 'NONE',  #971 ) ;
#66412 = CARTESIAN_POINT ( 'NONE',  ( -50.40445135320379677, -25.19502912051677868, 3.293943094755626078 ) ) ;
#66413 = EDGE_CURVE ( 'NONE', #56484, #88974, #63298, .T. ) ;
#66414 = LINE ( 'NONE', #19695, #18794 ) ;
#66415 = CARTESIAN_POINT ( 'NONE',  ( -70.32380231474228083, -25.13313949306887096, 7.101635536975467566 ) ) ;
#66416 = CARTESIAN_POINT ( 'NONE',  ( -11.18773875818744656, -18.78983145652188469, -1.500000000000002220 ) ) ;
#66417 = CARTESIAN_POINT ( 'NONE',  ( -31.52287095715006160, -24.65952944569304606, 1.056160979905690134 ) ) ;
#66418 = DIRECTION ( 'NONE',  ( -3.773278334453079618E-23, 0.9999999999976377785, 2.173523156925979975E-06 ) ) ;
#66419 = CARTESIAN_POINT ( 'NONE',  ( 10.54059822343757880, -5.876774720514426953, 23.12308057603841149 ) ) ;
#66420 = CARTESIAN_POINT ( 'NONE',  ( -48.52287095715007581, -23.47593901973090524, -1.443836447538997314 ) ) ;
#66421 = ORIENTED_EDGE ( 'NONE', *, *, #90589, .T. ) ;
#66422 = CARTESIAN_POINT ( 'NONE',  ( 13.37706023731332827, -15.40713922116925616, 11.49999999999998934 ) ) ;
#66423 = EDGE_LOOP ( 'NONE', ( #83358, #79522, #56832, #52105 ) ) ;
#66424 = VERTEX_POINT ( 'NONE', #55683 ) ;
#66425 = ORIENTED_EDGE ( 'NONE', *, *, #46680, .T. ) ;
#66426 = ORIENTED_EDGE ( 'NONE', *, *, #89465, .F. ) ;
#66427 = ADVANCED_FACE ( 'NONE', ( #1884 ), #24703, .T. ) ;
#66428 = EDGE_CURVE ( 'NONE', #84887, #38539, #33282, .T. ) ;
#66429 = CARTESIAN_POINT ( 'NONE',  ( -7.156825135384894843, 21.90021990432103038, -1.500000000000002220 ) ) ;
#66430 = CARTESIAN_POINT ( 'NONE',  ( 15.14080536460164517, -5.152774720514427642, -26.62908960815038384 ) ) ;
#66431 = CARTESIAN_POINT ( 'NONE',  ( 7.037473118728134303, -18.94123407977296480, -1.500000000000002220 ) ) ;
#66432 = EDGE_LOOP ( 'NONE', ( #76939, #70008, #13956, #68801, #62932 ) ) ;
#66433 = CARTESIAN_POINT ( 'NONE',  ( -98.62287095715009855, -23.95044443724991012, 10.65354141964649592 ) ) ;
#66434 = CARTESIAN_POINT ( 'NONE',  ( 6.650000000000004796, 0.000000000000000000, 18.35000000000000142 ) ) ;
#66435 = B_SPLINE_CURVE_WITH_KNOTS ( 'NONE', 3,
 ( #23658, #38893, #54631, #16048, #1348, #56140, #32283, #95188 ),
 .UNSPECIFIED., .F., .F.,
 ( 4, 2, 2, 4 ),
 ( -0.001224554619866351050, -0.0002241820295893694366, 0.0007761905606876121771, 0.002776935741241578874 ),
 .UNSPECIFIED. ) ;
#66436 = DIRECTION ( 'NONE',  ( -0.000000000000000000, 0.000000000000000000, -1.000000000000000000 ) ) ;
#66437 = DIRECTION ( 'NONE',  ( 0.000000000000000000, -0.9999999999976377785, -2.173523156925979975E-06 ) ) ;
#66439 = ORIENTED_EDGE ( 'NONE', *, *, #9734, .F. ) ;
#66438 = CARTESIAN_POINT ( 'NONE',  ( -21.34312709018487553, 1.176582458498846462, 11.49999999999999645 ) ) ;
#66440 = CARTESIAN_POINT ( 'NONE',  ( 6.403846153846157740, -5.876774720514425177, 21.48076923076922995 ) ) ;
#66441 = ORIENTED_EDGE ( 'NONE', *, *, #2828, .T. ) ;
#66442 = CARTESIAN_POINT ( 'NONE',  ( -19.27636426328722763, -11.15942449563467775, 11.49999999999998934 ) ) ;
#66443 = CARTESIAN_POINT ( 'NONE',  ( -13.01863806243235899, 16.06808769575019014, 11.49999999999998934 ) ) ;
#66444 = AXIS2_PLACEMENT_3D ( 'NONE', #20023, #19022, #49998 ) ;
#66445 = EDGE_CURVE ( 'NONE', #99197, #1165, #9987, .T. ) ;
#66446 = ORIENTED_EDGE ( 'NONE', *, *, #70764, .T. ) ;
#66447 = EDGE_CURVE ( 'NONE', #55725, #49833, #71903, .T. ) ;
#66448 = CARTESIAN_POINT ( 'NONE',  ( -113.5228709571500616, -24.65952944569304961, 1.056160979905704123 ) ) ;
#66449 = ORIENTED_EDGE ( 'NONE', *, *, #75818, .F. ) ;
#66450 = DIRECTION ( 'NONE',  ( 0.000000000000000000, 0.000000000000000000, -1.000000000000000000 ) ) ;
#66451 = VECTOR ( 'NONE', #83346, 1000.000000000000227 ) ;
#66452 = ORIENTED_EDGE ( 'NONE', *, *, #67709, .F. ) ;
#66453 = B_SPLINE_CURVE_WITH_KNOTS ( 'NONE', 3,
 ( #17975, #81870, #33703, #3763 ),
 .UNSPECIFIED., .F., .F.,
 ( 4, 4 ),
 ( 0.000000000000000000, 9.999999999998897304E-05 ),
 .UNSPECIFIED. ) ;
#66454 = CARTESIAN_POINT ( 'NONE',  ( 8.205893897551582938, 6.475225279485575136, -27.11136772256261196 ) ) ;
#66455 = CARTESIAN_POINT ( 'NONE',  ( -20.92377055399060737, -0.003182555231893603818, -1.500000000000002220 ) ) ;
#66456 = CARTESIAN_POINT ( 'NONE',  ( -13.81295463269534096, 17.03802364079049525, 11.49999999999999645 ) ) ;
#66457 = ADVANCED_FACE ( 'NONE', ( #10484 ), #64306, .T. ) ;
#66458 = PLANE ( 'NONE',  #22029 ) ;
#66459 = CARTESIAN_POINT ( 'NONE',  ( -18.95691745938505335, -12.16397891629814865, -1.500000000000002220 ) ) ;
#66460 = VECTOR ( 'NONE', #46973, 1000.000000000000114 ) ;
#66461 = CARTESIAN_POINT ( 'NONE',  ( 13.96602909953038640, 15.60522523583095200, 11.49999999999998934 ) ) ;
#66462 = ADVANCED_FACE ( 'NONE', ( #72902 ), #50063, .F. ) ;
#66463 = CARTESIAN_POINT ( 'NONE',  ( -92.62357510551103701, -24.66019654487200441, 8.947790411086112172 ) ) ;
#66464 = CARTESIAN_POINT ( 'NONE',  ( -27.96875734969026084, 3.316774720514426456, 0.7300228001186309656 ) ) ;
#66465 = CARTESIAN_POINT ( 'NONE',  ( 11.62916340711181284, 0.3587747205144265483, 28.75961759920349792 ) ) ;
#66466 = CYLINDRICAL_SURFACE ( 'NONE', #29665, 0.3000000000000016542 ) ;
#66467 = VERTEX_POINT ( 'NONE', #96234 ) ;
#66468 = EDGE_CURVE ( 'NONE', #85639, #97920, #11484, .T. ) ;
#66469 = AXIS2_PLACEMENT_3D ( 'NONE', #41836, #86983, #55555 ) ;
#66470 = ORIENTED_EDGE ( 'NONE', *, *, #33430, .F. ) ;
#66471 = AXIS2_PLACEMENT_3D ( 'NONE', #55042, #91712, #47927 ) ;
#66472 = ORIENTED_EDGE ( 'NONE', *, *, #89532, .T. ) ;
#66473 = CARTESIAN_POINT ( 'NONE',  ( -66.51586562461079666, -23.73766607897669800, -1.055555164236460897 ) ) ;
#66474 = AXIS2_PLACEMENT_3D ( 'NONE', #58351, #73565, #97396 ) ;
#66475 = CARTESIAN_POINT ( 'NONE',  ( 17.68986881342592454, -12.14045624799103962, -1.500000000000002220 ) ) ;
#66476 = ADVANCED_FACE ( 'NONE', ( #34833 ), #45881, .T. ) ;
#66477 = CARTESIAN_POINT ( 'NONE',  ( -59.52287095715006870, -24.51283580621364067, 0.6167428607019767028 ) ) ;
#66478 = ORIENTED_EDGE ( 'NONE', *, *, #93919, .F. ) ;
#66479 = CARTESIAN_POINT ( 'NONE',  ( -20.42954818520503935, 5.180689535515515587, 11.49999999999998934 ) ) ;
#66480 = CARTESIAN_POINT ( 'NONE',  ( -99.52764846858842418, -25.27419814425944011, 3.999772249604663710 ) ) ;
#66481 = CARTESIAN_POINT ( 'NONE',  ( 2.880689065218799083, -6.376774720514426065, 21.31732089891691828 ) ) ;
#66482 = CARTESIAN_POINT ( 'NONE',  ( -87.62287095715007013, -23.73907113216990439, -1.053371485793227258 ) ) ;
#66483 = B_SPLINE_CURVE_WITH_KNOTS ( 'NONE', 3,
 ( #82834, #75224, #90455, #84834, #67632, #6711 ),
 .UNSPECIFIED., .F., .F.,
 ( 4, 2, 4 ),
 ( 0.000000000000000000, 0.001380764517854769519, 0.002761529035709539039 ),
 .UNSPECIFIED. ) ;
#66484 = CARTESIAN_POINT ( 'NONE',  ( -102.5228709571500758, -29.50250786944525672, 11.44777988621623166 ) ) ;
#66485 = DIRECTION ( 'NONE',  ( 0.000000000000000000, 0.000000000000000000, 1.000000000000000000 ) ) ;
#66486 = CARTESIAN_POINT ( 'NONE',  ( 22.05266032001784637, -1.487345182339283367, -1.500000000000002220 ) ) ;
#66487 = CARTESIAN_POINT ( 'NONE',  ( -91.62287095715004170, -24.64898659630368627, 1.056161002820827921 ) ) ;
#66488 = DIRECTION ( 'NONE',  ( 1.000000000000000000, -0.000000000000000000, -0.000000000000000000 ) ) ;
#66489 = CARTESIAN_POINT ( 'NONE',  ( -60.62371844064301030, -25.00158670708909980, 2.256160236439220146 ) ) ;
#66490 = CARTESIAN_POINT ( 'NONE',  ( -25.52711720098805870, -24.43591384941821332, 1.590605884330588360 ) ) ;
#66491 = CARTESIAN_POINT ( 'NONE',  ( -63.52287095715004739, -24.51283580621364067, 0.6167428607019723730 ) ) ;
#66492 = CARTESIAN_POINT ( 'NONE',  ( 17.14628872753620215, 12.71262973326862245, 11.49999999999998934 ) ) ;
#66493 = DIRECTION ( 'NONE',  ( 1.000000000000000000, 3.773278334444166432E-23, 8.201307841325785021E-29 ) ) ;
#66494 = LINE ( 'NONE', #20765, #62479 ) ;
#66495 = B_SPLINE_CURVE_WITH_KNOTS ( 'NONE', 3,
 ( #78798, #78303, #93527, #24522 ),
 .UNSPECIFIED., .F., .F.,
 ( 4, 4 ),
 ( 2.176968243509707518E-15, 0.0001007173067907758126 ),
 .UNSPECIFIED. ) ;
#66496 = DIRECTION ( 'NONE',  ( 4.838869102739856157E-16, 0.000000000000000000, -1.000000000000000000 ) ) ;
#66497 = CARTESIAN_POINT ( 'NONE',  ( -68.52287095715006160, -23.48783264082476308, -1.443836473390092356 ) ) ;
#66498 = CARTESIAN_POINT ( 'NONE',  ( 22.31954755298990278, 3.869410565987296380, -1.500000000000002220 ) ) ;
#66499 = DIRECTION ( 'NONE',  ( -1.000000000000000000, -3.773278334444166432E-23, -8.201307841325785021E-29 ) ) ;
#66500 = ORIENTED_EDGE ( 'NONE', *, *, #84017, .F. ) ;
#66501 = LINE ( 'NONE', #91299, #57980 ) ;
#66502 = CARTESIAN_POINT ( 'NONE',  ( -25.92875734969026524, -5.356774720514425603, -0.08597719988137648983 ) ) ;
#66503 = CARTESIAN_POINT ( 'NONE',  ( -16.05533900033903549, 11.45903963230415101, 11.49999999999999645 ) ) ;
#66504 = FACE_OUTER_BOUND ( 'NONE', #91713, .T. ) ;
#66505 = CARTESIAN_POINT ( 'NONE',  ( -67.50570964152612419, -24.15543982623906416, -0.2315651400026651485 ) ) ;
#66506 = ORIENTED_EDGE ( 'NONE', *, *, #12946, .T. ) ;
#66507 = CARTESIAN_POINT ( 'NONE',  ( 10.40578984036287302, -5.965225279485572685, -28.04626194901324965 ) ) ;
#66508 = CARTESIAN_POINT ( 'NONE',  ( -110.5228709571500758, -23.47593901973090524, -1.443836447538996204 ) ) ;
#66509 = LINE ( 'NONE', #27913, #44760 ) ;
#66510 = CARTESIAN_POINT ( 'NONE',  ( -21.34238180412542718, 3.497892552127677135, 11.49999999999998934 ) ) ;
#66511 = DIRECTION ( 'NONE',  ( -0.000000000000000000, 1.000000000000000000, -0.000000000000000000 ) ) ;
#66512 = CARTESIAN_POINT ( 'NONE',  ( 14.52268490272241408, 12.84546865777419455, -1.500000000000002220 ) ) ;
#66513 = CARTESIAN_POINT ( 'NONE',  ( -109.5895376238167245, -23.47593901973091235, -1.443836447538999312 ) ) ;
#66514 = CARTESIAN_POINT ( 'NONE',  ( -80.59913673259377731, -25.04344369319006702, 7.561456861807408281 ) ) ;
#66515 = CARTESIAN_POINT ( 'NONE',  ( -19.57314199983870751, -2.777824058246878280, 11.49999999999998934 ) ) ;
#66516 = VERTEX_POINT ( 'NONE', #3398 ) ;
#66517 = CARTESIAN_POINT ( 'NONE',  ( 19.35245777310151993, -6.127589836641541332, 11.49999999999999645 ) ) ;
#66518 = PLANE ( 'NONE',  #44040 ) ;
#66519 = VECTOR ( 'NONE', #35713, 1000.000000000000000 ) ;
#66520 = CARTESIAN_POINT ( 'NONE',  ( 5.696197030082937651, -5.876774720514421624, 21.05387829558662816 ) ) ;
#66521 = EDGE_CURVE ( 'NONE', #82927, #53278, #26098, .T. ) ;
#66522 = ORIENTED_EDGE ( 'NONE', *, *, #72539, .F. ) ;
#66523 = CARTESIAN_POINT ( 'NONE',  ( -37.52287095715006870, -23.48786465467240347, 11.44779295918255180 ) ) ;
#66524 = CARTESIAN_POINT ( 'NONE',  ( -107.2228709571500644, -23.47596703998600631, 11.44779298504227860 ) ) ;
#66525 = LINE ( 'NONE', #46157, #48359 ) ;
#66526 = EDGE_CURVE ( 'NONE', #72403, #86308, #88620, .T. ) ;
#66527 = DIRECTION ( 'NONE',  ( -0.000000000000000000, -1.000000000000000000, -0.000000000000000000 ) ) ;
#66528 = EDGE_CURVE ( 'NONE', #61101, #50459, #14048, .T. ) ;
#66529 = CARTESIAN_POINT ( 'NONE',  ( -33.52287095715007581, -23.48783264083359512, -1.443836473376374441 ) ) ;
#66530 = CARTESIAN_POINT ( 'NONE',  ( -15.86121933104946535, 12.22609501325904624, 11.49999999999998934 ) ) ;
#66531 = EDGE_CURVE ( 'NONE', #93563, #72639, #86467, .T. ) ;
#66532 = CARTESIAN_POINT ( 'NONE',  ( -67.52287095715009002, -23.48783264082477018, -1.443836473390090802 ) ) ;
#66533 = EDGE_LOOP ( 'NONE', ( #25334, #82742, #1124, #61254 ) ) ;
#66534 = EDGE_CURVE ( 'NONE', #9124, #40720, #36472, .T. ) ;
#66535 = EDGE_CURVE ( 'NONE', #88108, #98244, #4111, .T. ) ;
#66536 = VECTOR ( 'NONE', #17152, 1000.000000000000000 ) ;
#66537 = LINE ( 'NONE', #41174, #6460 ) ;
#66538 = DIRECTION ( 'NONE',  ( 0.000000000000000000, -1.000000000000000000, 0.000000000000000000 ) ) ;
#66539 = DIRECTION ( 'NONE',  ( 0.000000000000000000, 0.9999999999976377785, 2.173523156925979128E-06 ) ) ;
#66541 = EDGE_CURVE ( 'NONE', #69177, #67333, #10546, .T. ) ;
#66540 = VECTOR ( 'NONE', #50421, 1000.000000000000000 ) ;
#66542 = CARTESIAN_POINT ( 'NONE',  ( -10.34999999999999254, -1.517883041479705813E-15, 3.499999999999998224 ) ) ;
#66543 = VECTOR ( 'NONE', #18171, 1000.000000000000114 ) ;
#66544 = FACE_OUTER_BOUND ( 'NONE', #76799, .T. ) ;
#66545 = CIRCLE ( 'NONE', #60006, 28.45799999999999486 ) ;
#66546 = DIRECTION ( 'NONE',  ( -0.000000000000000000, 1.000000000000000000, -0.000000000000000000 ) ) ;
#66547 = EDGE_LOOP ( 'NONE', ( #4635, #6648, #26760, #7258 ) ) ;
#66548 = CARTESIAN_POINT ( 'NONE',  ( -17.48930418531667996, -10.34094407820366612, -1.500000000000002220 ) ) ;
#66549 = ORIENTED_EDGE ( 'NONE', *, *, #7544, .T. ) ;
#66550 = EDGE_CURVE ( 'NONE', #65344, #37472, #25709, .T. ) ;
#66551 = CARTESIAN_POINT ( 'NONE',  ( 22.43992371924722917, 4.826111843257130829, 11.49999999999998934 ) ) ;
#66552 = CARTESIAN_POINT ( 'NONE',  ( -32.64292742023518912, -24.15543982623907127, -0.2315651400026567941 ) ) ;
#66553 = EDGE_LOOP ( 'NONE', ( #85522, #6641, #55715, #51603 ) ) ;
#66554 = CARTESIAN_POINT ( 'NONE',  ( -49.56947780960053507, -25.30465585254130190, 4.839518961770515659 ) ) ;
#66555 = CARTESIAN_POINT ( 'NONE',  ( 15.18017043975972058, 3.555325937910594813, -27.25057598448095675 ) ) ;
#66556 = ADVANCED_FACE ( 'NONE', ( #87620 ), #75871, .T. ) ;
#66557 = CARTESIAN_POINT ( 'NONE',  ( 22.81105451610979173, -6.475225279485573360, -17.31691820600746823 ) ) ;
#66558 = CARTESIAN_POINT ( 'NONE',  ( -4.955175619359221351, 20.59750927568439138, 11.49999999999999645 ) ) ;
#66559 = ORIENTED_EDGE ( 'NONE', *, *, #48525, .F. ) ;
#66560 = CARTESIAN_POINT ( 'NONE',  ( 15.99899278244174639, -15.33069297701436184, -1.500000000000002220 ) ) ;
#66561 = CARTESIAN_POINT ( 'NONE',  ( 19.39738937107077632, -6.937168198526852514, -1.500000000000002220 ) ) ;
#66562 = ORIENTED_EDGE ( 'NONE', *, *, #38482, .T. ) ;
#66563 = ORIENTED_EDGE ( 'NONE', *, *, #61110, .F. ) ;
#66564 = CARTESIAN_POINT ( 'NONE',  ( -82.62287095715005592, -29.50250786944525672, 11.44777988621623521 ) ) ;
#66565 = DIRECTION ( 'NONE',  ( -0.000000000000000000, 1.000000000000000000, -0.000000000000000000 ) ) ;
#66566 = ORIENTED_EDGE ( 'NONE', *, *, #48557, .T. ) ;
#66567 = ORIENTED_EDGE ( 'NONE', *, *, #20096, .F. ) ;
#66568 = ORIENTED_EDGE ( 'NONE', *, *, #10614, .T. ) ;
#66569 = PLANE ( 'NONE',  #12950 ) ;
#66570 = CARTESIAN_POINT ( 'NONE',  ( -71.58953762381672448, -24.64965694238407323, 8.947790433994656567 ) ) ;
#66571 = CARTESIAN_POINT ( 'NONE',  ( 14.43441819133218296, -3.316774720514428232, -28.36222020317221038 ) ) ;
#66572 = CARTESIAN_POINT ( 'NONE',  ( 14.12806351585482112, -15.20395780304818523, -1.500000000000002220 ) ) ;
#66573 = CARTESIAN_POINT ( 'NONE',  ( 3.708801897538985148, -21.39311272803122321, 11.49999999999999645 ) ) ;
#66574 = ORIENTED_EDGE ( 'NONE', *, *, #25073, .T. ) ;
#66575 = CARTESIAN_POINT ( 'NONE',  ( -121.9228709571500957, -23.47593901973090524, -1.443836447538996204 ) ) ;
#66576 = CARTESIAN_POINT ( 'NONE',  ( -119.6228709571500701, -23.48786465467241769, 11.44779295918253759 ) ) ;
#66577 = CARTESIAN_POINT ( 'NONE',  ( -20.53624283083718893, 9.024085183690161216, -1.500000000000002220 ) ) ;
#66578 = ADVANCED_FACE ( 'NONE', ( #36827 ), #90113, .F. ) ;
#66579 = CARTESIAN_POINT ( 'NONE',  ( -93.22287095715005023, -23.47593901973090524, -1.443836447538996870 ) ) ;
#66580 = CARTESIAN_POINT ( 'NONE',  ( -65.63298288181091777, -24.63355581998386867, 0.9682620441943842193 ) ) ;
#66581 = ORIENTED_EDGE ( 'NONE', *, *, #10198, .T. ) ;
#66582 = CARTESIAN_POINT ( 'NONE',  ( -59.52287095715005449, -24.50321055353803601, 9.387540953477529371 ) ) ;
#66583 = CARTESIAN_POINT ( 'NONE',  ( -89.81226385320383088, -25.05712135967894838, 7.447789548357302891 ) ) ;
#66584 = ORIENTED_EDGE ( 'NONE', *, *, #89968, .T. ) ;
#66585 = ORIENTED_EDGE ( 'NONE', *, *, #36513, .T. ) ;
#66587 = ADVANCED_FACE ( 'NONE', ( #83989 ), #27990, .T. ) ;
#66586 = AXIS2_PLACEMENT_3D ( 'NONE', #86392, #1666, #10776 ) ;
#66588 = CARTESIAN_POINT ( 'NONE',  ( -75.52287095715007581, -29.50247984919015209, -1.443849546365053582 ) ) ;
#66589 = ORIENTED_EDGE ( 'NONE', *, *, #85284, .F. ) ;
#66590 = CARTESIAN_POINT ( 'NONE',  ( -13.45305159987462851, 16.49040971879131234, -1.500000000000002220 ) ) ;
#66591 = ORIENTED_EDGE ( 'NONE', *, *, #23659, .F. ) ;
#66592 = CARTESIAN_POINT ( 'NONE',  ( -101.0861487085838206, -25.15054751950415124, 6.938118937714361500 ) ) ;
#66593 = CARTESIAN_POINT ( 'NONE',  ( 19.95399986947220583, -8.914707708046476498, 11.49999999999998934 ) ) ;
#66594 = CARTESIAN_POINT ( 'NONE',  ( -51.04357394935764347, -25.30543060587211812, 4.940877950953177056 ) ) ;
#66595 = CARTESIAN_POINT ( 'NONE',  ( 20.21490908150494192, 10.32750977814155391, 11.49999999999998934 ) ) ;
#66596 = CARTESIAN_POINT ( 'NONE',  ( -41.01720553446741491, -25.18430903175909208, 3.440463593108834317 ) ) ;
#66597 = FACE_OUTER_BOUND ( 'NONE', #76355, .T. ) ;
#66598 = CARTESIAN_POINT ( 'NONE',  ( -5.132426408838210108, -21.30661980433056968, -1.500000000000002220 ) ) ;
#66599 = LINE ( 'NONE', #27515, #59282 ) ;
#66600 = ORIENTED_EDGE ( 'NONE', *, *, #40417, .F. ) ;
#66601 = CARTESIAN_POINT ( 'NONE',  ( 29.62646972375975096, -5.339663449004302009, 28.46301402826327731 ) ) ;
#66602 = DIRECTION ( 'NONE',  ( 3.773278334444167608E-23, -1.000000000000000000, 0.000000000000000000 ) ) ;
#66603 = VERTEX_POINT ( 'NONE', #37819 ) ;
#66604 = CARTESIAN_POINT ( 'NONE',  ( -32.52287095715006870, -24.50321055353803956, 9.387540953477529371 ) ) ;
#66605 = AXIS2_PLACEMENT_3D ( 'NONE', #63735, #57612, #17530 ) ;
#66606 = CARTESIAN_POINT ( 'NONE',  ( -40.94688081444584782, -25.03284417894045788, 7.563176522466704910 ) ) ;
#66607 = AXIS2_PLACEMENT_3D ( 'NONE', #83868, #99083, #98084 ) ;
#66608 = CARTESIAN_POINT ( 'NONE',  ( -20.43227410087897056, -23.69217786884635402, 0.5637492489085929037 ) ) ;
#66609 = CARTESIAN_POINT ( 'NONE',  ( -4.916304867406160461, -20.68799595667769964, 11.49999999999998934 ) ) ;
#66610 = CARTESIAN_POINT ( 'NONE',  ( -112.5204660179142024, -23.73766607897671577, -1.055555164236427368 ) ) ;
#66611 = DIRECTION ( 'NONE',  ( -3.773278334453080206E-23, 0.9999999999976377785, 2.173523156925979975E-06 ) ) ;
#66612 = DIRECTION ( 'NONE',  ( -0.5656310827093756766, 0.8246584009594636333, 1.161164194647626880E-16 ) ) ;
#66613 = CARTESIAN_POINT ( 'NONE',  ( 29.73860345376319003, -1.477225279485574028, 19.84760796525321780 ) ) ;
#66614 = CARTESIAN_POINT ( 'NONE',  ( -84.52287095715006160, -23.48786465467241769, 11.44779295918254469 ) ) ;
#66615 = ORIENTED_EDGE ( 'NONE', *, *, #996, .T. ) ;
#66616 = CARTESIAN_POINT ( 'NONE',  ( 16.73968668634701729, 10.17700309559984717, 11.49999999999999645 ) ) ;
#66617 = CARTESIAN_POINT ( 'NONE',  ( -58.62287095715003460, -23.73934037231756378, 11.05740245334329153 ) ) ;
#66618 = CARTESIAN_POINT ( 'NONE',  ( -68.62287095715005592, -24.64898659630367916, 1.056161002820824368 ) ) ;
#66619 = VERTEX_POINT ( 'NONE', #21578 ) ;
#66620 = CARTESIAN_POINT ( 'NONE',  ( 4.261846905714947731, -5.876774720514426953, 21.73176331363731251 ) ) ;
#66621 = CARTESIAN_POINT ( 'NONE',  ( -85.52287095715009002, -23.47593901973090524, -1.443836447538996648 ) ) ;
#66622 = CARTESIAN_POINT ( 'NONE',  ( -122.6228709571500417, -23.47593901973091235, -1.443836447538997536 ) ) ;
#66623 = B_SPLINE_CURVE_WITH_KNOTS ( 'NONE', 3,
 ( #14738, #82756, #7131, #5138, #67061, #97969, #44212, #71214, #78799, #53995, #63618, #193, #9297, #76795 ),
 .UNSPECIFIED., .F., .F.,
 ( 4, 2, 2, 2, 2, 2, 4 ),
 ( 1.411962612463446054E-17, 0.0001548496297124576687, 0.0003096992594249011886, 0.0006193985188498282897, 0.0007742481485622923010, 0.0009290977782747563123, 0.001238797037699685202 ),
 .UNSPECIFIED. ) ;
#66624 = CARTESIAN_POINT ( 'NONE',  ( -106.5228709571500332, -23.48783264082477018, -1.443836473390085695 ) ) ;
#66625 = CARTESIAN_POINT ( 'NONE',  ( -9.385407830382300531, 17.29636241635495608, 11.49999999999998934 ) ) ;
#66626 = ORIENTED_EDGE ( 'NONE', *, *, #19167, .T. ) ;
#66627 = DIRECTION ( 'NONE',  ( -3.773278334453079030E-23, 0.9999999999976377785, 2.173523156925979128E-06 ) ) ;
#66628 = DIRECTION ( 'NONE',  ( 3.773278334444167608E-23, -1.000000000000000000, 0.000000000000000000 ) ) ;
#66629 = EDGE_CURVE ( 'NONE', #13594, #19685, #13973, .T. ) ;
#66630 = APPROVAL_ROLE ( '' ) ;
#66631 = VERTEX_POINT ( 'NONE', #53560 ) ;
#66632 = CARTESIAN_POINT ( 'NONE',  ( 9.021150247049410709, -0.9126213611645739299, 3.707288619710387589 ) ) ;
#66633 = CARTESIAN_POINT ( 'NONE',  ( -1.428094109758638819, -6.376774720514415407, 20.04104409779160179 ) ) ;
#66634 = CARTESIAN_POINT ( 'NONE',  ( -47.60694479324835271, -23.73766607897670866, -1.055555164236438914 ) ) ;
#66635 = DIRECTION ( 'NONE',  ( -3.773278334444166432E-23, 1.000000000000000000, 0.000000000000000000 ) ) ;
#66636 = CARTESIAN_POINT ( 'NONE',  ( -115.6228709571500559, -23.47596703998600631, 11.44779298504227860 ) ) ;
#66637 = EDGE_CURVE ( 'NONE', #27461, #21243, #99674, .T. ) ;
#66638 = CARTESIAN_POINT ( 'NONE',  ( -31.52166505407126706, -24.86441978397624553, 8.247789967200544581 ) ) ;
#66639 = B_SPLINE_CURVE_WITH_KNOTS ( 'NONE', 3,
 ( #40831, #57080, #72294, #88015 ),
 .UNSPECIFIED., .F., .F.,
 ( 4, 4 ),
 ( 0.000000000000000000, 9.999999999998897304E-05 ),
 .UNSPECIFIED. ) ;
#66640 = LINE ( 'NONE', #90442, #18680 ) ;
#66641 = CARTESIAN_POINT ( 'NONE',  ( -8.813339738934139689, -17.91118242276673911, 11.49999999999998934 ) ) ;
#66642 = ADVANCED_FACE ( 'NONE', ( #76853 ), #35828, .F. ) ;
#66643 = CARTESIAN_POINT ( 'NONE',  ( -41.62287095715006302, -24.66019654487199020, 8.947790411086135265 ) ) ;
#66644 = CARTESIAN_POINT ( 'NONE',  ( -0.003591441230561016797, -23.00350597096012351, 6.154653013508758264 ) ) ;
#66645 = EDGE_LOOP ( 'NONE', ( #60431, #59289, #42946, #36746 ) ) ;
#66646 = CARTESIAN_POINT ( 'NONE',  ( -117.5228709571500758, -29.50250786944525672, 11.44777988621622811 ) ) ;
#66647 = PLANE ( 'NONE',  #27892 ) ;
#66648 = EDGE_CURVE ( 'NONE', #96543, #14119, #67271, .T. ) ;
#66649 = EDGE_CURVE ( 'NONE', #81670, #13730, #24829, .T. ) ;
#66650 =( NAMED_UNIT ( * ) SI_UNIT ( $, .STERADIAN. ) SOLID_ANGLE_UNIT ( ) );
#66651 = CARTESIAN_POINT ( 'NONE',  ( 11.40529837385589218, -6.376774720514345240, -28.07356074678033409 ) ) ;
#66652 = CARTESIAN_POINT ( 'NONE',  ( -126.7286271109977775, -25.23514665191783735, 6.311484830854977801 ) ) ;
#66653 = LINE ( 'NONE', #23413, #45172 ) ;
#66654 = EDGE_CURVE ( 'NONE', #31048, #47313, #85144, .T. ) ;
#66655 = AXIS2_PLACEMENT_3D ( 'NONE', #68216, #36765, #28157 ) ;
#66656 = CARTESIAN_POINT ( 'NONE',  ( -26.09636659181000340, -24.96935267319560126, 4.940287552382958580 ) ) ;
#66657 = DIRECTION ( 'NONE',  ( -0.000000000000000000, 0.000000000000000000, 1.000000000000000000 ) ) ;
#66658 = ORIENTED_EDGE ( 'NONE', *, *, #22805, .T. ) ;
#66659 = DIRECTION ( 'NONE',  ( 1.000000000000000000, -0.000000000000000000, -0.000000000000000000 ) ) ;
#66660 = CARTESIAN_POINT ( 'NONE',  ( 6.274899854645557440, -6.376774720514429617, 21.83451738260096775 ) ) ;
#66661 = ORIENTED_EDGE ( 'NONE', *, *, #42349, .F. ) ;
#66662 = CARTESIAN_POINT ( 'NONE',  ( 14.48468284575590204, 14.13777120147990729, 11.49999999999998934 ) ) ;
#66663 = CARTESIAN_POINT ( 'NONE',  ( -122.6256512063165189, -23.96119346886880663, -0.6495511937832028071 ) ) ;
#66664 = CARTESIAN_POINT ( 'NONE',  ( -129.6228709571498996, -24.33832256527048798, 0.1851278514138701703 ) ) ;
#66665 = CARTESIAN_POINT ( 'NONE',  ( -6.660000000000001030, -10.15233964170348457, -1.303165529866009420 ) ) ;
#66666 = ORIENTED_EDGE ( 'NONE', *, *, #8092, .F. ) ;
#66667 = DIRECTION ( 'NONE',  ( 0.000000000000000000, 0.000000000000000000, -1.000000000000000000 ) ) ;
#66668 = DIRECTION ( 'NONE',  ( 0.000000000000000000, -2.173523156925980399E-06, 0.9999999999976378895 ) ) ;
#66669 = VECTOR ( 'NONE', #63120, 1000.000000000000114 ) ;
#66670 = CARTESIAN_POINT ( 'NONE',  ( 0.1258803491696451060, 20.03332480481931199, -1.500000000000002220 ) ) ;
#66671 = B_SPLINE_CURVE_WITH_KNOTS ( 'NONE', 3,
 ( #69067, #557, #46741, #16781 ),
 .UNSPECIFIED., .F., .F.,
 ( 4, 4 ),
 ( 0.000000000000000000, 0.0001002978978731602401 ),
 .UNSPECIFIED. ) ;
#66672 = CARTESIAN_POINT ( 'NONE',  ( 20.75205275252385206, -3.532026382766447536, 11.49999999999999645 ) ) ;
#66673 = AXIS2_PLACEMENT_3D ( 'NONE', #2966, #3958, #33899 ) ;
#66674 = CARTESIAN_POINT ( 'NONE',  ( -27.97342827235127061, -24.83868590882142868, 7.574733681428329923 ) ) ;
#66675 = CARTESIAN_POINT ( 'NONE',  ( -111.6228709571500843, -23.95044443724992433, 10.65354141964650481 ) ) ;
#66676 = CARTESIAN_POINT ( 'NONE',  ( -4.445301477617020325, 21.63612927058290936, -1.500000000000002220 ) ) ;
#66677 = B_SPLINE_CURVE_WITH_KNOTS ( 'NONE', 3,
 ( #3544, #49727, #42116, #9139 ),
 .UNSPECIFIED., .F., .F.,
 ( 4, 4 ),
 ( 2.830056797201531266E-06, 0.0004722118875754793095 ),
 .UNSPECIFIED. ) ;
#66678 = CARTESIAN_POINT ( 'NONE',  ( -39.85544541354917669, -25.27806075124410157, 4.937103068824292507 ) ) ;
#66679 = DIRECTION ( 'NONE',  ( 0.000000000000000000, -1.000000000000000000, 0.000000000000000000 ) ) ;
#66680 = CARTESIAN_POINT ( 'NONE',  ( -50.40445135320380388, -25.18440101920884189, 3.293943117856050762 ) ) ;
#66681 = VERTEX_POINT ( 'NONE', #94598 ) ;
#66682 = CARTESIAN_POINT ( 'NONE',  ( -35.52287095715008292, -25.00182538069144655, 7.747789668545105535 ) ) ;
#66683 = CARTESIAN_POINT ( 'NONE',  ( -31.60165242513933492, -23.96119346886880663, -0.6495511937832003646 ) ) ;
#66684 = ORIENTED_EDGE ( 'NONE', *, *, #59236, .F. ) ;
#66685 = ORIENTED_EDGE ( 'NONE', *, *, #3045, .F. ) ;
#66686 = CARTESIAN_POINT ( 'NONE',  ( 2.100208336950355914, 0.000000000000000000, 1.249999999999996003 ) ) ;
#66687 = CARTESIAN_POINT ( 'NONE',  ( -6.660000000000001030, -2.191226316053958875E-18, 2.701633758479787833E-17 ) ) ;
#66688 = CARTESIAN_POINT ( 'NONE',  ( -76.60617745381290433, -23.48783264082477373, -1.443836473390089026 ) ) ;
#66689 = CARTESIAN_POINT ( 'NONE',  ( -0.003042231299257275486, -20.61035990087709635, -1.500000000000002220 ) ) ;
#66690 = CARTESIAN_POINT ( 'NONE',  ( -8.857468890034409625, -19.66367526556523870, 11.49999999999999645 ) ) ;
#66691 = EDGE_LOOP ( 'NONE', ( #38671, #40035, #19425, #6733 ) ) ;
#66692 = CARTESIAN_POINT ( 'NONE',  ( -83.62287095715008434, -23.72773821059536559, 11.05748984161097503 ) ) ;
#66693 = LINE ( 'NONE', #60563, #95275 ) ;
#66694 = CARTESIAN_POINT ( 'NONE',  ( -114.6228709571500559, -29.50250786944525672, 11.44777988621622988 ) ) ;
#66695 = CARTESIAN_POINT ( 'NONE',  ( 16.92800457317958518, -14.60656088873787262, 11.49999999999998934 ) ) ;
#66696 = CARTESIAN_POINT ( 'NONE',  ( 29.76209104404536987, -5.356774720514427379, 26.42884784083909366 ) ) ;
#66697 = DIRECTION ( 'NONE',  ( 0.000000000000000000, -1.000000000000000000, 0.000000000000000000 ) ) ;
#66698 = ORIENTED_EDGE ( 'NONE', *, *, #43043, .F. ) ;
#66699 = CARTESIAN_POINT ( 'NONE',  ( -94.52287095715011844, -23.48783264082477373, -1.443836473390087027 ) ) ;
#66700 = DIRECTION ( 'NONE',  ( 0.000000000000000000, 1.000000000000000000, -0.000000000000000000 ) ) ;
#66701 = CARTESIAN_POINT ( 'NONE',  ( 12.60132613692001691, 16.66296579206088069, 11.49999999999998934 ) ) ;
#66702 = ORIENTED_EDGE ( 'NONE', *, *, #87931, .F. ) ;
#66703 = ADVANCED_FACE ( 'NONE', ( #55553 ), #25079, .F. ) ;
#66705 = VERTEX_POINT ( 'NONE', #55049 ) ;
#66704 = CARTESIAN_POINT ( 'NONE',  ( -39.18367763993130382, -25.22434093780323394, 3.596805738460790547 ) ) ;
#66706 = EDGE_LOOP ( 'NONE', ( #2699, #11845, #72430, #51242 ) ) ;
#66707 = CARTESIAN_POINT ( 'NONE',  ( -100.6369782943210254, -23.85049219812686161, 10.88485053497527133 ) ) ;
#66708 = CARTESIAN_POINT ( 'NONE',  ( -16.97324839047195866, 12.58421825509937442, -1.500000000000002220 ) ) ;
#66709 = ADVANCED_FACE ( 'NONE', ( #61673 ), #54543, .F. ) ;
#66710 = VERTEX_POINT ( 'NONE', #8363 ) ;
#66711 = CARTESIAN_POINT ( 'NONE',  ( -96.22287095715009286, -23.47593901973090524, -1.443836447538997314 ) ) ;
#66712 = CARTESIAN_POINT ( 'NONE',  ( -8.160000000000000142, 2.888964624466060727, -0.2527516539682188590 ) ) ;
#66713 = PLANE ( 'NONE',  #5965 ) ;
#66714 = CARTESIAN_POINT ( 'NONE',  ( -68.52287095715006160, -23.48786465467241058, 11.44779295918254647 ) ) ;
#66715 = FACE_OUTER_BOUND ( 'NONE', #98924, .T. ) ;
#66716 = CARTESIAN_POINT ( 'NONE',  ( -21.05831370385527990, 5.553659732266172711, -1.500000000000002220 ) ) ;
#66717 = DIRECTION ( 'NONE',  ( 0.000000000000000000, 0.000000000000000000, -1.000000000000000000 ) ) ;
#66719 = VERTEX_POINT ( 'NONE', #70768 ) ;
#66718 = CARTESIAN_POINT ( 'NONE',  ( -21.99995728619510516, 3.820703864638951952, 11.49999999999999645 ) ) ;
#66720 = CARTESIAN_POINT ( 'NONE',  ( -45.62287095715004881, -25.00158670708908915, 2.256160236439166855 ) ) ;
#66721 = CARTESIAN_POINT ( 'NONE',  ( -97.62287095715005592, -24.66019654487200086, 8.947790411086124607 ) ) ;
#66722 = CARTESIAN_POINT ( 'NONE',  ( 9.940598223437577374, -5.876774720514426953, 22.08128695274315945 ) ) ;
#66723 = VERTEX_POINT ( 'NONE', #62669 ) ;
#66725 = ORIENTED_EDGE ( 'NONE', *, *, #48073, .T. ) ;
#66724 = CARTESIAN_POINT ( 'NONE',  ( -56.62287095715005592, -23.48783264082478084, -1.443836473390068820 ) ) ;
#66726 = ORIENTED_EDGE ( 'NONE', *, *, #85655, .F. ) ;
#66727 = LINE ( 'NONE', #4309, #1088 ) ;
#66728 = VECTOR ( 'NONE', #71356, 1000.000000000000000 ) ;
#66729 = CARTESIAN_POINT ( 'NONE',  ( 6.600000000000001421, 0.000000000000000000, 0.000000000000000000 ) ) ;
#66730 = CARTESIAN_POINT ( 'NONE',  ( 30.61643171304412903, -3.316774720514426456, 27.37433008668283207 ) ) ;
#66731 = CARTESIAN_POINT ( 'NONE',  ( -49.17860766247945747, -25.30062163087967519, 4.391665315653317414 ) ) ;
#66732 = CARTESIAN_POINT ( 'NONE',  ( 10.86264265030973952, 0.3587747205144257157, -27.62597719988137612 ) ) ;
#66733 = CARTESIAN_POINT ( 'NONE',  ( -7.749999999999996447, 25.69999999999999574, 2.100000000000000089 ) ) ;
#66734 = ORIENTED_EDGE ( 'NONE', *, *, #17882, .T. ) ;
#66735 = CARTESIAN_POINT ( 'NONE',  ( -19.00951991574052968, 3.723548053296564575, 11.49999999999999645 ) ) ;
#66736 = CARTESIAN_POINT ( 'NONE',  ( -115.5228709571500048, -24.15516710230294350, 10.28746687063725851 ) ) ;
#66737 = EDGE_LOOP ( 'NONE', ( #58785, #71828, #95858, #2881 ) ) ;
#66738 = CARTESIAN_POINT ( 'NONE',  ( 2.932009311892267434, -5.876774720514410077, 19.53174284846577891 ) ) ;
#66739 = CARTESIAN_POINT ( 'NONE',  ( 2.677564053859940341, -5.876774720514407413, 19.16116138973293559 ) ) ;
#66740 = DIRECTION ( 'NONE',  ( -1.000000000000000000, -3.773278334444167608E-23, -8.201307833595939069E-29 ) ) ;
#66741 = CARTESIAN_POINT ( 'NONE',  ( -30.63240354163743717, -23.78087380709146004, 10.97511746239721298 ) ) ;
#66742 = VECTOR ( 'NONE', #95551, 1000.000000000000000 ) ;
#66743 = CARTESIAN_POINT ( 'NONE',  ( 5.347671334029483248, -18.86178030415664963, -1.500000000000002220 ) ) ;
#66744 = CARTESIAN_POINT ( 'NONE',  ( -116.6228709571500559, -24.65952944569305316, 1.056160979905706121 ) ) ;
#66746 = VERTEX_POINT ( 'NONE', #77856 ) ;
#66745 = CC_DESIGN_APPROVAL ( #29008, ( #69913 ) ) ;
#66747 = CARTESIAN_POINT ( 'NONE',  ( -4.138935798035190849, -21.16376344109877294, -1.500000000000002220 ) ) ;
#66748 = CARTESIAN_POINT ( 'NONE',  ( -33.53806327265973408, -24.35071581493542325, 9.817618358456039473 ) ) ;
#66749 = CARTESIAN_POINT ( 'NONE',  ( -81.14580165399679856, -25.30394787373862187, 5.096590184867776152 ) ) ;
#66750 = CARTESIAN_POINT ( 'NONE',  ( -40.62513263387344864, -23.48783264082477018, -1.443836473390102570 ) ) ;
#66751 = CARTESIAN_POINT ( 'NONE',  ( 0.000000000000000000, -6.376774720514426953, 15.00000000000000178 ) ) ;
#66752 = CARTESIAN_POINT ( 'NONE',  ( -19.99251892732797486, -11.32171818645973538, -1.500000000000002220 ) ) ;
#66753 = CALENDAR_DATE ( 2026, 9, 10 ) ;
#66754 = PLANE ( 'NONE',  #32087 ) ;
#66755 = DIRECTION ( 'NONE',  ( 0.6599726524652365089, 0.000000000000000000, -0.7512896232465879898 ) ) ;
#66756 = CARTESIAN_POINT ( 'NONE',  ( 16.24926901856429140, 11.90123039513101411, 11.49999999999999645 ) ) ;
#66757 = CARTESIAN_POINT ( 'NONE',  ( 0.000000000000000000, -5.876774720514426953, 0.000000000000000000 ) ) ;
#66758 = CARTESIAN_POINT ( 'NONE',  ( -32.51245690601021465, -23.73791477778911485, 11.05961554403171299 ) ) ;
#66759 = PLANE ( 'NONE',  #11705 ) ;
#66760 = CARTESIAN_POINT ( 'NONE',  ( -126.5228709571500616, -23.47596703998600631, 11.44779298504227683 ) ) ;
#66761 = CARTESIAN_POINT ( 'NONE',  ( -95.92287095715005307, -23.47596703998600276, 11.44779298504227860 ) ) ;
#66762 = CARTESIAN_POINT ( 'NONE',  ( -7.150643268323968904, -18.52920452239153448, 11.49999999999998934 ) ) ;
#66763 = B_SPLINE_CURVE_WITH_KNOTS ( 'NONE', 3,
 ( #80093, #47657, #80591, #40544 ),
 .UNSPECIFIED., .F., .F.,
 ( 4, 4 ),
 ( 0.000000000000000000, 0.0001000000000000167422 ),
 .UNSPECIFIED. ) ;
#66764 = EDGE_CURVE ( 'NONE', #86336, #42928, #39309, .T. ) ;
#66765 = LINE ( 'NONE', #90076, #62603 ) ;
#66766 = CARTESIAN_POINT ( 'NONE',  ( 6.578723047037327909, -18.57437435983987584, -1.500000000000002220 ) ) ;
#66767 = CARTESIAN_POINT ( 'NONE',  ( -126.5204122989497222, -24.66019654487200796, 8.947790411086103290 ) ) ;
#66768 = EDGE_CURVE ( 'NONE', #76458, #44866, #16462, .T. ) ;
#66769 = EDGE_CURVE ( 'NONE', #38340, #35617, #27183, .T. ) ;
#66770 = LINE ( 'NONE', #97688, #30557 ) ;
#66771 = CARTESIAN_POINT ( 'NONE',  ( 3.051095722660301934, -6.376774720514410077, 19.07493897947323092 ) ) ;
#66772 = CARTESIAN_POINT ( 'NONE',  ( 7.914317726235799100, 19.11507755054979896, 11.49999999999999645 ) ) ;
#66773 = CARTESIAN_POINT ( 'NONE',  ( 7.460332110455646593, -6.376774720514418959, 20.55293369838740247 ) ) ;
#66774 = EDGE_CURVE ( 'NONE', #84269, #87661, #31192, .T. ) ;
#66775 = CARTESIAN_POINT ( 'NONE',  ( 3.252401863874210264, -5.965225279485592225, -29.35688408629928858 ) ) ;
#66776 = CARTESIAN_POINT ( 'NONE',  ( -16.57510365746454184, 15.48777146884464884, 11.49999999999999645 ) ) ;
#66777 = CIRCLE ( 'NONE', #21314, 2.499999999999998668 ) ;
#66778 = EDGE_LOOP ( 'NONE', ( #15594, #6721, #91144, #39228 ) ) ;
#66779 = DIRECTION ( 'NONE',  ( -3.773278334453079618E-23, 0.9999999999976377785, 2.173523156925979975E-06 ) ) ;
#66780 = DIRECTION ( 'NONE',  ( 1.000000000000000000, 0.000000000000000000, -0.000000000000000000 ) ) ;
#66781 = ADVANCED_FACE ( 'NONE', ( #32193 ), #1264, .F. ) ;
#66782 = CARTESIAN_POINT ( 'NONE',  ( -36.62287095715006302, -24.65952944569303895, 1.056160979905693909 ) ) ;
#66783 = CARTESIAN_POINT ( 'NONE',  ( 2.499999999999988454, 22.00000000000000000, 0.000000000000000000 ) ) ;
#66784 = ORIENTED_EDGE ( 'NONE', *, *, #15121, .T. ) ;
#66785 = VERTEX_POINT ( 'NONE', #78857 ) ;
#66786 = CARTESIAN_POINT ( 'NONE',  ( 0.3910256410256418569, -5.876774720514419847, 20.67377804487180271 ) ) ;
#66787 = CARTESIAN_POINT ( 'NONE',  ( -15.36296916364455711, -16.94538937337987150, 11.49999999999998934 ) ) ;
#66788 = LINE ( 'NONE', #51048, #81068 ) ;
#66789 = CARTESIAN_POINT ( 'NONE',  ( -0.8629811567608781653, -21.54619324973139172, -1.500000000000002220 ) ) ;
#66790 = CARTESIAN_POINT ( 'NONE',  ( -113.5917734516337561, -23.96169478059713853, 10.65365249895717348 ) ) ;
#66791 = DIRECTION ( 'NONE',  ( 1.000000000000000000, 3.773278334444167608E-23, 8.201307833595939069E-29 ) ) ;
#66792 = CARTESIAN_POINT ( 'NONE',  ( 21.78986343443989071, 5.811249688775594002, 11.49999999999999645 ) ) ;
#66793 = VERTEX_POINT ( 'NONE', #94092 ) ;
#66794 = CARTESIAN_POINT ( 'NONE',  ( -27.96875734969026084, 6.143225279485574397, 24.50402280011861933 ) ) ;
#66795 = CARTESIAN_POINT ( 'NONE',  ( 5.346615758220810477, 21.33151429383102382, 11.49999999999998934 ) ) ;
#66796 = CARTESIAN_POINT ( 'NONE',  ( -111.5553612508262376, -23.96119346886881019, -0.6495511937832035843 ) ) ;
#66797 = CARTESIAN_POINT ( 'NONE',  ( 29.73860345376319003, -5.356471260711259674, 19.84760796525321425 ) ) ;
#66798 = ORIENTED_EDGE ( 'NONE', *, *, #95878, .F. ) ;
#66799 = CARTESIAN_POINT ( 'NONE',  ( 8.160000000000000142, 0.000000000000000000, 0.000000000000000000 ) ) ;
#66800 = CARTESIAN_POINT ( 'NONE',  ( -49.62287095715005592, -29.50248528299804818, 1.056150453629033370 ) ) ;
#66801 = ORIENTED_EDGE ( 'NONE', *, *, #794, .T. ) ;
#66802 = CARTESIAN_POINT ( 'NONE',  ( -84.62287095715005592, -23.47593901973091235, -1.443836447539004642 ) ) ;
#66803 = EDGE_LOOP ( 'NONE', ( #98858, #41713, #96924, #60226 ) ) ;
#66804 = ORIENTED_EDGE ( 'NONE', *, *, #46440, .F. ) ;
#66805 = DIRECTION ( 'NONE',  ( 0.000000000000000000, -1.000000000000000000, 0.000000000000000000 ) ) ;
#66806 = DIRECTION ( 'NONE',  ( 0.7071067811865476838, 0.000000000000000000, -0.7071067811865474617 ) ) ;
#66807 = CARTESIAN_POINT ( 'NONE',  ( -103.5228709571501042, -23.47593901973090524, -1.443836447538996204 ) ) ;
#66808 = CARTESIAN_POINT ( 'NONE',  ( -6.584652030910324250, 19.34213596296284265, -1.500000000000002220 ) ) ;
#66809 = ORIENTED_EDGE ( 'NONE', *, *, #92720, .F. ) ;
#66810 = CARTESIAN_POINT ( 'NONE',  ( -71.70841769935766763, -25.24715640642683923, 6.192981443001071895 ) ) ;
#66811 = CARTESIAN_POINT ( 'NONE',  ( 13.91401389203221406, -5.965225279485572685, 158.0376437107427137 ) ) ;
#66812 = EDGE_CURVE ( 'NONE', #47230, #92103, #70520, .T. ) ;
#66814 = FACE_OUTER_BOUND ( 'NONE', #16329, .T. ) ;
#66813 = AXIS2_PLACEMENT_3D ( 'NONE', #67585, #44245, #75173 ) ;
#66815 = CARTESIAN_POINT ( 'NONE',  ( -5.265981236333618470E-16, -2.056774720514426669, -4.299999999999999822 ) ) ;
#66816 = ORIENTED_EDGE ( 'NONE', *, *, #3327, .T. ) ;
#66817 = CARTESIAN_POINT ( 'NONE',  ( -50.52287095715006160, -23.47596703998600631, 11.44779298504229104 ) ) ;
#66818 = CARTESIAN_POINT ( 'NONE',  ( -97.58953762381671027, -24.66019654487199730, 8.947790411086122830 ) ) ;
#66819 = CC_DESIGN_APPROVAL ( #68642, ( #78135 ) ) ;
#66820 = ORIENTED_EDGE ( 'NONE', *, *, #39416, .T. ) ;
#66821 = CARTESIAN_POINT ( 'NONE',  ( 2.677173591928626806, -20.63698567995287902, -1.500000000000002220 ) ) ;
#66823 = ADVANCED_FACE ( 'NONE', ( #86486, #7861 ), #16970, .F. ) ;
#66822 = ORIENTED_EDGE ( 'NONE', *, *, #43649, .T. ) ;
#66825 = ORIENTED_EDGE ( 'NONE', *, *, #90390, .T. ) ;
#66824 = PLANE ( 'NONE',  #70201 ) ;
#66826 = CARTESIAN_POINT ( 'NONE',  ( -44.58953762381671737, -23.47596703998600276, 11.44779298504227505 ) ) ;
#66827 = CARTESIAN_POINT ( 'NONE',  ( -33.52287095715007581, -23.94994826722564696, -0.6494450866342740269 ) ) ;
#66828 = EDGE_LOOP ( 'NONE', ( #83406, #65051, #25655, #83209 ) ) ;
#66829 = ORIENTED_EDGE ( 'NONE', *, *, #88267, .T. ) ;
#66830 = CARTESIAN_POINT ( 'NONE',  ( -114.6228709571500701, -23.73907113216991860, -1.053371485793227480 ) ) ;
#66831 = DIRECTION ( 'NONE',  ( -1.000000000000000000, 0.000000000000000000, 0.000000000000000000 ) ) ;
#66832 = DIRECTION ( 'NONE',  ( 0.000000000000000000, 0.000000000000000000, 1.000000000000000000 ) ) ;
#66833 = CARTESIAN_POINT ( 'NONE',  ( -70.90175588921343319, -25.31201622164140019, 5.458926420340825203 ) ) ;
#66835 = ORIENTED_EDGE ( 'NONE', *, *, #67835, .F. ) ;
#66834 = CARTESIAN_POINT ( 'NONE',  ( -8.753671783739276790, -20.25744411100385634, 11.49999999999999645 ) ) ;
#66836 = CARTESIAN_POINT ( 'NONE',  ( -72.62287095715008434, -24.51283580621364067, 0.6167428607019815878 ) ) ;
#66837 = CARTESIAN_POINT ( 'NONE',  ( 22.41689761077644860, -2.907977976681301424, -1.500000000000002220 ) ) ;
#66839 = ORIENTED_EDGE ( 'NONE', *, *, #26105, .F. ) ;
#66838 = LINE ( 'NONE', #59717, #11740 ) ;
#66840 = VERTEX_POINT ( 'NONE', #71269 ) ;
#66841 = CARTESIAN_POINT ( 'NONE',  ( -10.12789510953808758, -4.109924279452578766, 30.41617935552199370 ) ) ;
#66842 = APPROVAL ( #56133, 'UNSPECIFIED' ) ;
#66843 = AXIS2_PLACEMENT_3D ( 'NONE', #88050, #9408, #95156 ) ;
#66844 = CARTESIAN_POINT ( 'NONE',  ( -57.49752954236778635, -24.35071581493543036, 9.817618358456028815 ) ) ;
#66845 = ORIENTED_EDGE ( 'NONE', *, *, #100353, .F. ) ;
#66846 = FACE_OUTER_BOUND ( 'NONE', #66553, .T. ) ;
#66847 = CARTESIAN_POINT ( 'NONE',  ( -20.55991158545366204, 8.586518200734140294, -1.500000000000002220 ) ) ;
#66848 = B_SPLINE_CURVE_WITH_KNOTS ( 'NONE', 3,
 ( #24433, #93437, #85327, #54899, #91946, #7709 ),
 .UNSPECIFIED., .F., .F.,
 ( 4, 2, 4 ),
 ( 6.391158118959991367E-06, 0.001387004593080781592, 0.002767618028042603297 ),
 .UNSPECIFIED. ) ;
#66849 = CARTESIAN_POINT ( 'NONE',  ( -45.52287095715006160, -29.50247984919015209, -1.443849546365058689 ) ) ;
#66850 = ORIENTED_EDGE ( 'NONE', *, *, #3275, .T. ) ;
#66851 = LINE ( 'NONE', #97772, #90263 ) ;
#66852 = FACE_OUTER_BOUND ( 'NONE', #11248, .T. ) ;
#66853 = CARTESIAN_POINT ( 'NONE',  ( 32.66876533700882845, -5.965225279485572685, -12.58926540598385557 ) ) ;
#66854 = CARTESIAN_POINT ( 'NONE',  ( -49.58953762381673158, -24.66019654487199020, 8.947790411086131712 ) ) ;
#66855 = CARTESIAN_POINT ( 'NONE',  ( -11.52932745282126703, -15.74164922852205173, 11.49999999999998934 ) ) ;
#66856 = VECTOR ( 'NONE', #89075, 1000.000000000000114 ) ;
#66857 = CARTESIAN_POINT ( 'NONE',  ( -7.526967427842778946, 20.06989004931119425, -1.500000000000002220 ) ) ;
#66858 = CARTESIAN_POINT ( 'NONE',  ( -0.8460708837923186509, -6.376774720514411854, 19.21968329462762526 ) ) ;
#66859 = DIRECTION ( 'NONE',  ( -0.000000000000000000, -1.000000000000000000, -0.000000000000000000 ) ) ;
#66860 = CARTESIAN_POINT ( 'NONE',  ( -52.62287095715005592, -24.64965695001467694, 8.947790433994185832 ) ) ;
#66861 = CARTESIAN_POINT ( 'NONE',  ( -15.12447472116105729, 17.10960193589383849, -1.500000000000002220 ) ) ;
#66862 = DIRECTION ( 'NONE',  ( -1.000000000000000000, -0.000000000000000000, -0.000000000000000000 ) ) ;
#66863 = DIRECTION ( 'NONE',  ( -1.000000000000000000, -0.000000000000000000, -0.000000000000000000 ) ) ;
#66864 = CARTESIAN_POINT ( 'NONE',  ( -7.409219584043468920, -18.53548363135739052, 11.49999999999999645 ) ) ;
#66865 = CARTESIAN_POINT ( 'NONE',  ( -69.52287095715007581, -24.34917612406836440, 0.1852690917426526862 ) ) ;
#66866 = CARTESIAN_POINT ( 'NONE',  ( -57.62287095715004881, -24.64898659630367916, 1.056161002820822592 ) ) ;
#66867 = CARTESIAN_POINT ( 'NONE',  ( -48.56040139242229969, -23.73766607897670866, -1.055555164236436028 ) ) ;
#66868 = EDGE_CURVE ( 'NONE', #4203, #53932, #80226, .T. ) ;
#66869 = ORIENTED_EDGE ( 'NONE', *, *, #20827, .F. ) ;
#66870 = CARTESIAN_POINT ( 'NONE',  ( -25.53098197642538736, -24.92569209777881056, 4.942811685741776984 ) ) ;
#66871 = CARTESIAN_POINT ( 'NONE',  ( 10.59058046163345423, -3.703784075859317682, -26.99573265033922453 ) ) ;
#66872 = CARTESIAN_POINT ( 'NONE',  ( 0.4029737066630413311, -21.70969715354747009, 11.49999999999998934 ) ) ;
#66873 = DIRECTION ( 'NONE',  ( -0.000000000000000000, 1.000000000000000000, -0.000000000000000000 ) ) ;
#66874 = CARTESIAN_POINT ( 'NONE',  ( -9.627943313441900131, 16.98966435471970726, -1.500000000000002220 ) ) ;
#66875 = CARTESIAN_POINT ( 'NONE',  ( -34.52287095715005449, -24.34917612407030063, 0.1852690917476900179 ) ) ;
#66876 = AXIS2_PLACEMENT_3D ( 'NONE', #68831, #46489, #37385 ) ;
#66877 = VERTEX_POINT ( 'NONE', #62166 ) ;
#66878 = COORDINATED_UNIVERSAL_TIME_OFFSET ( 0, 0, .AHEAD. ) ;
#66879 = APPROVAL_PERSON_ORGANIZATION ( #45267, #59956, #22889 ) ;
#66880 = ADVANCED_FACE ( 'NONE', ( #93090 ), #23573, .T. ) ;
#66881 = LINE ( 'NONE', #4964, #27319 ) ;
#66882 = CARTESIAN_POINT ( 'NONE',  ( -12.12210191164509965, 16.44476101713275185, 11.49999999999999645 ) ) ;
#66883 = CARTESIAN_POINT ( 'NONE',  ( -47.52287095715005449, -24.35013146730202749, 9.818937971375104823 ) ) ;
#66884 = ADVANCED_FACE ( 'NONE', ( #26597 ), #91207, .T. ) ;
#66885 = DIRECTION ( 'NONE',  ( 1.000000000000000000, 0.000000000000000000, 0.000000000000000000 ) ) ;
#66886 = AXIS2_PLACEMENT_3D ( 'NONE', #10431, #40392, #80449 ) ;
#66887 = ORIENTED_EDGE ( 'NONE', *, *, #53452, .F. ) ;
#66888 = DIRECTION ( 'NONE',  ( -0.9952638024365005887, -0.000000000000000000, -0.09721092304694052555 ) ) ;
#66889 = LINE ( 'NONE', #12071, #86581 ) ;
#66890 = DIRECTION ( 'NONE',  ( 0.000000000000000000, 1.000000000000000000, 0.000000000000000000 ) ) ;
#66891 = AXIS2_PLACEMENT_3D ( 'NONE', #80421, #1306, #47478 ) ;
#66892 = EDGE_CURVE ( 'NONE', #4780, #31601, #97100, .T. ) ;
#66893 = FACE_OUTER_BOUND ( 'NONE', #45170, .T. ) ;
#66894 = ORIENTED_EDGE ( 'NONE', *, *, #41886, .T. ) ;
#66895 = CARTESIAN_POINT ( 'NONE',  ( 0.000000000000000000, -5.876774720514426953, 0.000000000000000000 ) ) ;
#66896 = B_SPLINE_CURVE_WITH_KNOTS ( 'NONE', 3,
 ( #29729, #273, #68298, #45471, #92121, #36852 ),
 .UNSPECIFIED., .F., .F.,
 ( 4, 2, 4 ),
 ( 0.000000000000000000, 0.001380764517853247083, 0.002761529035706494165 ),
 .UNSPECIFIED. ) ;
#66897 = CARTESIAN_POINT ( 'NONE',  ( 20.85440106035463970, 9.703512019146668166, 11.49999999999999645 ) ) ;
#66898 = CARTESIAN_POINT ( 'NONE',  ( -9.230423729802735622, -20.81519635545753033, -1.500000000000002220 ) ) ;
#66899 = CARTESIAN_POINT ( 'NONE',  ( 3.362030615038681169, -6.376774720514424288, 21.34376340489846413 ) ) ;
#66900 = B_SPLINE_SURFACE_WITH_KNOTS ( 'NONE', 3, 3, ( 
 ( #20124, #5402, #51086, #28741 ),
 ( #11161, #73567, #4057, #65479 ),
 ( #78775, #35001, #86406, #24501 ),
 ( #57860, #50235, #97398, #12653 ),
 ( #80673, #65981, #96899, #26391 ),
 ( #81172, #42136, #42629, #49747 ),
 ( #73076, #3561, #43617, #55469 ) ),
 .UNSPECIFIED., .F., .F., .F.,
 ( 4, 3, 4 ),
 ( 4, 4 ),
 ( 0.7945040050992239200, 0.8970133687736496775, 0.9995227324480754350 ),
 ( 0.009496410415874824429, 0.01051351914406330537 ),
 .UNSPECIFIED. ) ;
#66901 = CARTESIAN_POINT ( 'NONE',  ( -122.6228709571500417, -24.64898659630368627, 1.056161002820833028 ) ) ;
#66902 = CARTESIAN_POINT ( 'NONE',  ( -120.5228709571500474, -24.62285846331434058, 9.038163153548365969 ) ) ;
#66903 = DIRECTION ( 'NONE',  ( 0.000000000000000000, 0.000000000000000000, 1.000000000000000000 ) ) ;
#66904 = CARTESIAN_POINT ( 'NONE',  ( -110.5858259164890569, -25.00158670708910336, 2.256160236439218814 ) ) ;
#66905 = CARTESIAN_POINT ( 'NONE',  ( 21.76694381678408519, 2.417257996116004115, 11.49999999999998934 ) ) ;
#66906 = LINE ( 'NONE', #89731, #88333 ) ;
#66907 = VECTOR ( 'NONE', #24148, 1000.000000000000114 ) ;
#66908 = CARTESIAN_POINT ( 'NONE',  ( -103.5562042904834072, -24.66019654487199730, 8.947790411086124607 ) ) ;
#66909 = DIRECTION ( 'NONE',  ( 0.000000000000000000, -1.000000000000000000, 0.000000000000000000 ) ) ;
#66910 = CARTESIAN_POINT ( 'NONE',  ( 0.000000000000000000, 1.477225279485574028, 19.84760796525321425 ) ) ;
#66911 = ORIENTED_EDGE ( 'NONE', *, *, #21172, .F. ) ;
#66912 = CARTESIAN_POINT ( 'NONE',  ( 19.60162835767302880, 5.811842276320244416, 11.49999999999998934 ) ) ;
#66913 = ORIENTED_EDGE ( 'NONE', *, *, #56999, .T. ) ;
#66914 = ORIENTED_EDGE ( 'NONE', *, *, #46979, .T. ) ;
#66915 = ORIENTED_EDGE ( 'NONE', *, *, #73619, .T. ) ;
#66916 = VERTEX_POINT ( 'NONE', #58548 ) ;
#66917 = EDGE_CURVE ( 'NONE', #85527, #10916, #28422, .T. ) ;
#66918 = CARTESIAN_POINT ( 'NONE',  ( -11.96207688724106610, 19.68918167733909641, 11.49999999999998934 ) ) ;
#66919 = CARTESIAN_POINT ( 'NONE',  ( -61.53495354322418365, -24.65952944569304606, 1.056160979905699682 ) ) ;
#66920 = CARTESIAN_POINT ( 'NONE',  ( -13.29518446780263119, -15.22762515321373478, -1.500000000000002220 ) ) ;
#66921 = VECTOR ( 'NONE', #22214, 1000.000000000000114 ) ;
#66922 = VERTEX_POINT ( 'NONE', #81376 ) ;
#66923 = FACE_OUTER_BOUND ( 'NONE', #13476, .T. ) ;
#66924 = CARTESIAN_POINT ( 'NONE',  ( -127.5562042904833646, -24.64965694238575722, 8.947790433994185832 ) ) ;
#66925 = CARTESIAN_POINT ( 'NONE',  ( -95.58393195655612828, -24.92564183028979841, 1.928384488918254425 ) ) ;
#66926 = CARTESIAN_POINT ( 'NONE',  ( -53.65128113065046733, -23.73791477778911485, 11.05961554403170766 ) ) ;
#66928 = EDGE_LOOP ( 'NONE', ( #78674, #87698, #77766, #50796, #902, #75169, #86839, #58583, #29963, #95150, #92474, #22563, #60203, #85661, #100058, #66452, #30832, #46329, #81783, #92461, #57965, #47425, #82353, #100113 ) ) ;
#66927 = CARTESIAN_POINT ( 'NONE',  ( 11.41860910855227829, 18.14899599152127152, 11.49999999999999645 ) ) ;
#66929 = CARTESIAN_POINT ( 'NONE',  ( -113.6228709571500559, -23.47593901973091235, -1.443836447538999312 ) ) ;
#66930 = AXIS2_PLACEMENT_3D ( 'NONE', #29029, #60007, #52381 ) ;
#66931 = VERTEX_POINT ( 'NONE', #10361 ) ;
#66932 = CARTESIAN_POINT ( 'NONE',  ( 15.88595335714125589, -15.59144682577495189, 11.49999999999998934 ) ) ;
#66933 = CARTESIAN_POINT ( 'NONE',  ( -1.398219401198234957, 20.63772364298462847, 11.49999999999998934 ) ) ;
#66934 = ORIENTED_EDGE ( 'NONE', *, *, #92479, .T. ) ;
#66935 = EDGE_CURVE ( 'NONE', #68864, #99512, #87743, .T. ) ;
#66936 = CARTESIAN_POINT ( 'NONE',  ( -29.58953762381671382, -24.58200030392595892, 8.947790445854003849 ) ) ;
#66937 = EDGE_LOOP ( 'NONE', ( #87234, #16606, #58667, #32681 ) ) ;
#66938 = B_SPLINE_CURVE_WITH_KNOTS ( 'NONE', 3,
 ( #31648, #99645, #701, #60630 ),
 .UNSPECIFIED., .F., .F.,
 ( 4, 4 ),
 ( 0.4390812836509193628, 0.4400820306916847779 ),
 .UNSPECIFIED. ) ;
#66939 = FACE_OUTER_BOUND ( 'NONE', #58194, .T. ) ;
#66940 = EDGE_LOOP ( 'NONE', ( #100389, #61461, #35981, #67721 ) ) ;
#66941 = CARTESIAN_POINT ( 'NONE',  ( -16.12721948686093754, -13.32240427740599564, -1.500000000000002220 ) ) ;
#66942 = CARTESIAN_POINT ( 'NONE',  ( -9.563806973793814947, 19.74097577964120376, 11.49999999999999645 ) ) ;
#66943 = CARTESIAN_POINT ( 'NONE',  ( -37.61807812461461964, -23.48786465467240703, 11.44779295918255180 ) ) ;
#66944 = CARTESIAN_POINT ( 'NONE',  ( -12.86601690267178100, 18.50254183665605012, -1.500000000000002220 ) ) ;
#66945 = CARTESIAN_POINT ( 'NONE',  ( 17.97375762979478253, -10.76934015532128797, 11.49999999999998934 ) ) ;
#66946 = CARTESIAN_POINT ( 'NONE',  ( 6.431189903846153300, -5.876774720514415407, 20.08974358974358765 ) ) ;
#66947 = CARTESIAN_POINT ( 'NONE',  ( -91.62287095715004170, -23.48783264082478794, -1.443836473390063713 ) ) ;
#66948 = AXIS2_PLACEMENT_3D ( 'NONE', #16178, #85189, #55263 ) ;
#66949 = LINE ( 'NONE', #36476, #49178 ) ;
#66950 = ORIENTED_EDGE ( 'NONE', *, *, #79038, .F. ) ;
#66951 = SECURITY_CLASSIFICATION ( '', '', #77449 ) ;
#66952 = ORIENTED_EDGE ( 'NONE', *, *, #38419, .T. ) ;
#66953 = EDGE_LOOP ( 'NONE', ( #91838, #15253, #85062, #20373 ) ) ;
#66954 = DIRECTION ( 'NONE',  ( 0.000000000000000000, 0.000000000000000000, 1.000000000000000000 ) ) ;
#66955 = B_SPLINE_CURVE_WITH_KNOTS ( 'NONE', 3,
 ( #87023, #86022, #16498, #47470, #32231, #17007, #23607, #25114 ),
 .UNSPECIFIED., .F., .F.,
 ( 4, 2, 2, 4 ),
 ( -0.001224554619866347364, -0.0002241820295893631482, 0.0007761905606876210676, 0.002776935741241580609 ),
 .UNSPECIFIED. ) ;
#66956 = ADVANCED_FACE ( 'NONE', ( #4260 ), #35209, .F. ) ;
#66957 = CARTESIAN_POINT ( 'NONE',  ( 18.57079561221590325, -10.74342183689097574, -1.500000000000002220 ) ) ;
#66958 = VECTOR ( 'NONE', #99640, 1000.000000000000000 ) ;
#66959 = DIRECTION ( 'NONE',  ( 3.773278334444166432E-23, -1.000000000000000000, 0.000000000000000000 ) ) ;
#66960 = ORIENTED_EDGE ( 'NONE', *, *, #21122, .T. ) ;
#66961 = CARTESIAN_POINT ( 'NONE',  ( -6.733481718715807141, 19.98004043397084928, 11.49999999999998934 ) ) ;
#66962 = CARTESIAN_POINT ( 'NONE',  ( -99.56332528172060847, -25.25520022910753326, 3.790695193615264635 ) ) ;
#66963 = CARTESIAN_POINT ( 'NONE',  ( -28.47875734969025885, -5.965225279485572685, -0.08597719988136941216 ) ) ;
#66964 = EDGE_CURVE ( 'NONE', #55779, #76974, #95601, .T. ) ;
#66965 = DIRECTION ( 'NONE',  ( -0.000000000000000000, -1.000000000000000000, -0.000000000000000000 ) ) ;
#66966 = CARTESIAN_POINT ( 'NONE',  ( 10.22568704553358643, 3.316774720514425567, -27.02513721610328901 ) ) ;
#66967 = CARTESIAN_POINT ( 'NONE',  ( -0.9988807608215116707, -5.876774720514410966, 19.30497968945844889 ) ) ;
#66968 = CARTESIAN_POINT ( 'NONE',  ( 0.6065052782250800467, 22.08157775750015617, -1.500000000000002220 ) ) ;
#66969 = VECTOR ( 'NONE', #52723, 1000.000000000000114 ) ;
#66970 = CARTESIAN_POINT ( 'NONE',  ( -103.5228709571501042, -23.48783264082477018, -1.443836473390087916 ) ) ;
#66971 = CARTESIAN_POINT ( 'NONE',  ( -70.62287095715005592, -29.50249982740957577, 7.747779886224967605 ) ) ;
#66972 = CARTESIAN_POINT ( 'NONE',  ( -41.86646858058957577, -25.27955811415035470, 4.347424021778468095 ) ) ;
#66973 = ADVANCED_FACE ( 'NONE', ( #11858 ), #87996, .F. ) ;
#66974 = EDGE_CURVE ( 'NONE', #65146, #78010, #10869, .T. ) ;
#66975 = CARTESIAN_POINT ( 'NONE',  ( -100.5511821681996878, -24.40034930558991633, 0.3402023900116076804 ) ) ;
#66976 = CARTESIAN_POINT ( 'NONE',  ( -2.795030477444873540, 19.22867370847827573, 11.49999999999998934 ) ) ;
#66977 = EDGE_CURVE ( 'NONE', #55307, #78770, #65680, .T. ) ;
#66978 = CARTESIAN_POINT ( 'NONE',  ( 9.194277187580093269, -19.27880637823015419, -1.500000000000002220 ) ) ;
#66979 = CYLINDRICAL_SURFACE ( 'NONE', #49887, 2.399999999999999911 ) ;
#66980 = CARTESIAN_POINT ( 'NONE',  ( -89.80423082004377022, -25.26266127311082954, 3.981777872396911278 ) ) ;
#66981 = CARTESIAN_POINT ( 'NONE',  ( -70.52287095715007581, -24.99156044556120548, 7.747789690856173195 ) ) ;
#66982 = CARTESIAN_POINT ( 'NONE',  ( 30.77564450787169292, -1.682774720514426114, -9.689394075852828081 ) ) ;
#66983 = CARTESIAN_POINT ( 'NONE',  ( 21.71957326813621592, -6.446789169762093152, -1.500000000000002220 ) ) ;
#66984 = B_SPLINE_SURFACE_WITH_KNOTS ( 'NONE', 3, 1, ( 
 ( #51653, #58761 ),
 ( #82593, #5468 ),
 ( #42057, #96324 ),
 ( #26813, #88717 ),
 ( #19188, #50160 ),
 ( #81097, #22671 ),
 ( #350, #30804 ),
 ( #22173, #31298 ),
 ( #21183, #92193 ),
 ( #83581, #53657 ),
 ( #46531, #13567 ),
 ( #29801, #7958 ),
 ( #85084, #6471 ),
 ( #29301, #62265 ),
 ( #44537, #60274 ),
 ( #68866, #67878 ),
 ( #52148, #99786 ),
 ( #83074, #60768 ),
 ( #37425, #75462 ) ),
 .UNSPECIFIED., .F., .F., .F.,
 ( 4, 1, 1, 1, 1, 1, 1, 1, 1, 1, 1, 1, 1, 1, 1, 1, 4 ),
 ( 2, 2 ),
 ( 0.000000000000000000, 0.06076009704672557382, 0.1197352241628591996, 0.1777568621302152985, 0.2359989679007910846, 0.2940703618108028161, 0.3537332155261553868, 0.4159726195849062780, 0.4801398374083836740, 0.5450760546750318403, 0.6087348974468034246, 0.6721778698820234377, 0.7354527509796394691, 0.7991115937514117196, 0.8642836660180990282, 0.9308370508155386913, 1.000000000000000000 ),
 ( 0.000000000000000000, 1.000000000000000000 ),
 .UNSPECIFIED. ) ;
#66985 = ORIENTED_EDGE ( 'NONE', *, *, #74622, .T. ) ;
#66986 = DIRECTION ( 'NONE',  ( 0.000000000000000000, 0.000000000000000000, -1.000000000000000000 ) ) ;
#66987 = CARTESIAN_POINT ( 'NONE',  ( -79.58492028048088684, -24.51314013834315375, 0.6176544820404122893 ) ) ;
#66988 = CARTESIAN_POINT ( 'NONE',  ( 14.33573519231038063, 13.56928687979844561, 11.49999999999999645 ) ) ;
#66989 = PLANE ( 'NONE',  #21290 ) ;
#66990 = CARTESIAN_POINT ( 'NONE',  ( -104.6228709571500559, -29.50248528299804818, 1.056150453629042030 ) ) ;
#66991 = EDGE_CURVE ( 'NONE', #95233, #90367, #51432, .T. ) ;
#66992 = ORIENTED_EDGE ( 'NONE', *, *, #23866, .T. ) ;
#66993 = CARTESIAN_POINT ( 'NONE',  ( -59.52287095715006870, -24.50216790748205042, 0.6166512839542541702 ) ) ;
#66994 = CARTESIAN_POINT ( 'NONE',  ( -29.61081252053125112, -25.26026626986611134, 3.196430263304397279 ) ) ;
#66995 = VECTOR ( 'NONE', #40605, 1000.000000000000000 ) ;
#66996 = CARTESIAN_POINT ( 'NONE',  ( -100.4799102492508780, -25.17353343721469372, 7.101073737836308908 ) ) ;
#66997 = CARTESIAN_POINT ( 'NONE',  ( -17.57154585214776077, 12.61476001598989782, -1.500000000000002220 ) ) ;
#66998 = CARTESIAN_POINT ( 'NONE',  ( -49.11088876609831289, -25.10935348367436504, 3.850712044224722685 ) ) ;
#66999 = CARTESIAN_POINT ( 'NONE',  ( -14.46832242630667942, -12.86894606327920876, -1.500000000000002220 ) ) ;
#67000 = CARTESIAN_POINT ( 'NONE',  ( -19.37210865224160017, 0.3587747205143967943, -21.60955166348796297 ) ) ;
#67001 = CARTESIAN_POINT ( 'NONE',  ( -48.62287095715004881, -29.50250786944525672, 11.44777988621624054 ) ) ;
#67002 = CARTESIAN_POINT ( 'NONE',  ( 14.04693994163893578, -13.95676237773968609, -1.500000000000002220 ) ) ;
#67003 = EDGE_LOOP ( 'NONE', ( #61028, #19801, #38800, #58590 ) ) ;
#67004 = VECTOR ( 'NONE', #44530, 1000.000000000000000 ) ;
#67005 = CARTESIAN_POINT ( 'NONE',  ( 17.32893120472914816, 10.46255702124672027, 11.49999999999999645 ) ) ;
#67006 = DIRECTION ( 'NONE',  ( 0.000000000000000000, 0.9999999999976377785, 2.173523156925979128E-06 ) ) ;
#67007 = EDGE_CURVE ( 'NONE', #85588, #58867, #22295, .T. ) ;
#67008 = CARTESIAN_POINT ( 'NONE',  ( 5.864225667603142789, -5.876774720514423400, 21.27837265517432996 ) ) ;
#67009 = EDGE_CURVE ( 'NONE', #67625, #48223, #20460, .T. ) ;
#67010 = ORIENTED_EDGE ( 'NONE', *, *, #30893, .T. ) ;
#67011 = DIRECTION ( 'NONE',  ( -0.9951627101165078093, -0.09824042138329590335, 0.000000000000000000 ) ) ;
#67012 = DIRECTION ( 'NONE',  ( 1.334402673828313339E-16, -0.000000000000000000, -1.000000000000000000 ) ) ;
#67013 = FACE_OUTER_BOUND ( 'NONE', #57065, .T. ) ;
#67014 = FACE_OUTER_BOUND ( 'NONE', #83859, .T. ) ;
#67015 = DIRECTION ( 'NONE',  ( 0.000000000000000000, 1.000000000000000000, 0.000000000000000000 ) ) ;
#67016 = CARTESIAN_POINT ( 'NONE',  ( -11.36185547594953249, 16.55520930037988592, 11.49999999999998934 ) ) ;
#67017 = EDGE_CURVE ( 'NONE', #25101, #53541, #90979, .T. ) ;
#67018 = CARTESIAN_POINT ( 'NONE',  ( 8.160000000000000142, -11.08332949055823846, -0.7794760011071779626 ) ) ;
#67019 = ORIENTED_EDGE ( 'NONE', *, *, #52540, .T. ) ;
#67020 = EDGE_CURVE ( 'NONE', #39091, #10813, #43815, .T. ) ;
#67021 = CIRCLE ( 'NONE', #71866, 6.594667762285749468 ) ;
#67022 = ADVANCED_FACE ( 'NONE', ( #5743 ), #51931, .F. ) ;
#67023 = CARTESIAN_POINT ( 'NONE',  ( -50.05252738782304789, -25.26258873067627775, 4.679464405298413787 ) ) ;
#67024 = LINE ( 'NONE', #97932, #67259 ) ;
#67025 = CARTESIAN_POINT ( 'NONE',  ( -53.62287095715005592, -23.47593901973091235, -1.443836447539009749 ) ) ;
#67026 = CARTESIAN_POINT ( 'NONE',  ( -43.58953762381672448, -24.64965694238406613, 8.947790433994661896 ) ) ;
#67027 = ADVANCED_BREP_SHAPE_REPRESENTATION ( '', ( #10173, #37391 ), #14765 ) ;
#67028 = CARTESIAN_POINT ( 'NONE',  ( -118.6228709571500559, -24.51387760970725083, 9.387446482453411178 ) ) ;
#67029 = VECTOR ( 'NONE', #14528, 1000.000000000000114 ) ;
#67030 = CARTESIAN_POINT ( 'NONE',  ( -17.72129891523481149, -13.73837202384828515, 11.49999999999999645 ) ) ;
#67031 = CARTESIAN_POINT ( 'NONE',  ( -93.62287095715005592, -24.64898659630367916, 1.056161002820827921 ) ) ;
#67032 = VERTEX_POINT ( 'NONE', #89986 ) ;
#67033 = CARTESIAN_POINT ( 'NONE',  ( -7.038884989605349141, -19.10714869031923513, 11.49999999999998934 ) ) ;
#67034 = VECTOR ( 'NONE', #33372, 1000.000000000000114 ) ;
#67035 = ORIENTED_EDGE ( 'NONE', *, *, #97795, .T. ) ;
#67036 = CARTESIAN_POINT ( 'NONE',  ( -8.204236019480731557, -21.45505762417899831, -1.500000000000002220 ) ) ;
#67037 = CARTESIAN_POINT ( 'NONE',  ( -89.62287095715004170, -23.47593901973091235, -1.443836447539002865 ) ) ;
#67038 = EDGE_LOOP ( 'NONE', ( #73078, #51064, #8025, #57844 ) ) ;
#67039 = DIRECTION ( 'NONE',  ( -1.000000000000000000, 0.000000000000000000, 1.895872651340772790E-16 ) ) ;
#67040 = CARTESIAN_POINT ( 'NONE',  ( -77.52212609141741950, -23.48786465467240703, 11.44779295918254647 ) ) ;
#67041 = CARTESIAN_POINT ( 'NONE',  ( -77.52287095715007581, -23.48783264082476308, -1.443836473390091912 ) ) ;
#67043 = EDGE_LOOP ( 'NONE', ( #66350, #70473 ) ) ;
#67042 = CARTESIAN_POINT ( 'NONE',  ( 21.18767802922067034, -0.7184367399587067160, 11.49999999999999645 ) ) ;
#67044 = VERTEX_POINT ( 'NONE', #21448 ) ;
#67045 = CARTESIAN_POINT ( 'NONE',  ( 7.527104757430762128, -20.84474501729809859, 11.49999999999998934 ) ) ;
#67046 = CARTESIAN_POINT ( 'NONE',  ( 14.24201292913401140, 14.87178044790754328, -1.500000000000002220 ) ) ;
#67047 = EDGE_LOOP ( 'NONE', ( #3130, #5532, #92715, #34258 ) ) ;
#67048 = VERTEX_POINT ( 'NONE', #14340 ) ;
#67049 = LINE ( 'NONE', #74145, #56041 ) ;
#67050 = CARTESIAN_POINT ( 'NONE',  ( -49.62287095715004881, -24.33832256526968862, 0.1851278514119874263 ) ) ;
#67051 = ORIENTED_EDGE ( 'NONE', *, *, #6852, .T. ) ;
#67052 = ORIENTED_EDGE ( 'NONE', *, *, #65203, .T. ) ;
#67053 = ORIENTED_EDGE ( 'NONE', *, *, #73786, .T. ) ;
#67054 = CARTESIAN_POINT ( 'NONE',  ( 1.305682803664691249, 5.965225279485572685, 29.57950906855421991 ) ) ;
#67055 = CARTESIAN_POINT ( 'NONE',  ( -108.5228709571500616, -24.65952944569304961, 1.056160979905704123 ) ) ;
#67056 = CARTESIAN_POINT ( 'NONE',  ( 14.62889129739783556, -4.326482771707137687, -28.09837290214700545 ) ) ;
#67057 = CARTESIAN_POINT ( 'NONE',  ( -15.22196369898608737, 14.14466773073655581, -1.500000000000002220 ) ) ;
#67058 = CARTESIAN_POINT ( 'NONE',  ( 14.05712878599199200, -16.60762996970646199, 11.49999999999999645 ) ) ;
#67059 = ORIENTED_EDGE ( 'NONE', *, *, #66252, .F. ) ;
#67060 = VECTOR ( 'NONE', #48861, 1000.000000000000000 ) ;
#67061 = CARTESIAN_POINT ( 'NONE',  ( -100.6903391770916016, -25.18886833083715970, 3.321861835454170464 ) ) ;
#67062 = CARTESIAN_POINT ( 'NONE',  ( -34.62287095715007013, -23.47596703998600276, 11.44779298504227505 ) ) ;
#67063 = CARTESIAN_POINT ( 'NONE',  ( -115.5895851036066944, -24.52300882791528736, 0.6510814631126266017 ) ) ;
#67064 = CARTESIAN_POINT ( 'NONE',  ( 6.649717926671450563, 21.43536518531312396, -1.500000000000002220 ) ) ;
#67065 = CARTESIAN_POINT ( 'NONE',  ( -24.90875734969025501, 6.376774720514426953, 26.43402280011862615 ) ) ;
#67066 = CARTESIAN_POINT ( 'NONE',  ( -65.55177604255820256, -24.15503026093916361, -0.2815557561904382111 ) ) ;
#67067 = ORIENTED_EDGE ( 'NONE', *, *, #41680, .T. ) ;
#67068 = CARTESIAN_POINT ( 'NONE',  ( -71.60141483542169283, -25.30054065008881636, 5.617309697255326029 ) ) ;
#67069 = CARTESIAN_POINT ( 'NONE',  ( -119.4728709571500502, -25.21113200442379565, 5.000950862978366551 ) ) ;
#67070 = VECTOR ( 'NONE', #78989, 1000.000000000000000 ) ;
#67071 = EDGE_LOOP ( 'NONE', ( #31839, #37246, #88128, #51780 ) ) ;
#67072 = ORIENTED_EDGE ( 'NONE', *, *, #93361, .T. ) ;
#67073 = DIRECTION ( 'NONE',  ( 0.000000000000000000, -1.000000000000000000, 0.000000000000000000 ) ) ;
#67074 = EDGE_LOOP ( 'NONE', ( #39350, #6035 ) ) ;
#67075 = EDGE_CURVE ( 'NONE', #53340, #63553, #98583, .T. ) ;
#67076 = CARTESIAN_POINT ( 'NONE',  ( 21.27783752795556538, -0.9766432368044721812, -1.500000000000002220 ) ) ;
#67077 = VERTEX_POINT ( 'NONE', #67663 ) ;
#67078 = CARTESIAN_POINT ( 'NONE',  ( -5.366453405989236813, 0.000000000000000000, 0.000000000000000000 ) ) ;
#67079 = CARTESIAN_POINT ( 'NONE',  ( 12.58402814888991372, -17.87355554032721372, 11.49999999999998934 ) ) ;
#67080 = DIRECTION ( 'NONE',  ( 0.000000000000000000, -2.173523156925980399E-06, 0.9999999999976378895 ) ) ;
#67081 = CARTESIAN_POINT ( 'NONE',  ( 22.47986593085892437, -3.190245585651162230, 11.49999999999998934 ) ) ;
#67082 = CARTESIAN_POINT ( 'NONE',  ( -87.62287095715004170, -29.50250786944525672, 11.44777988621623344 ) ) ;
#67083 = FACE_OUTER_BOUND ( 'NONE', #44518, .T. ) ;
#67084 = CARTESIAN_POINT ( 'NONE',  ( 16.22650188657148362, -14.79325693486936188, -1.500000000000002220 ) ) ;
#67085 = CARTESIAN_POINT ( 'NONE',  ( -39.52287095715008292, -23.48783264082476308, -1.443836473390098574 ) ) ;
#67086 = VERTEX_POINT ( 'NONE', #52428 ) ;
#67087 = CARTESIAN_POINT ( 'NONE',  ( 29.58888977143521970, -4.303425171653743497, 29.06172452911802750 ) ) ;
#67088 = DIRECTION ( 'NONE',  ( -3.773278334453079030E-23, 0.9999999999976377785, 2.173523156925979128E-06 ) ) ;
#67089 = B_SPLINE_CURVE_WITH_KNOTS ( 'NONE', 3,
 ( #29928, #76094, #54287, #69500, #39547, #78087 ),
 .UNSPECIFIED., .F., .F.,
 ( 4, 2, 4 ),
 ( 0.000000000000000000, 0.001380764517854760629, 0.002761529035709521258 ),
 .UNSPECIFIED. ) ;
#67090 = EDGE_CURVE ( 'NONE', #37715, #55534, #29077, .T. ) ;
#67091 = EDGE_CURVE ( 'NONE', #75143, #77563, #93844, .T. ) ;
#67092 = ORIENTED_EDGE ( 'NONE', *, *, #54912, .F. ) ;
#67093 = EDGE_CURVE ( 'NONE', #64682, #44287, #57574, .T. ) ;
#67094 = CARTESIAN_POINT ( 'NONE',  ( -84.64454908083816065, -23.48786465467241413, 11.44779295918254469 ) ) ;
#67095 = CARTESIAN_POINT ( 'NONE',  ( -39.58953762381672448, -23.48783264082477373, -1.443836473390072594 ) ) ;
#67096 = EDGE_CURVE ( 'NONE', #92960, #64351, #63499, .T. ) ;
#67097 = FACE_BOUND ( 'NONE', #38136, .T. ) ;
#67098 = CARTESIAN_POINT ( 'NONE',  ( -16.85803360905838488, 12.98640638483674259, 11.49999999999998934 ) ) ;
#67099 = CARTESIAN_POINT ( 'NONE',  ( -98.50937779290613605, -24.51419770103155926, 9.386484678747176957 ) ) ;
#67100 = DIRECTION ( 'NONE',  ( 8.334928612639484546E-17, -1.000000000000000000, 7.321843366904296032E-17 ) ) ;
#67101 = CARTESIAN_POINT ( 'NONE',  ( -85.63005396505535316, -24.63355581998386157, 0.9682620441943895484 ) ) ;
#67102 = CARTESIAN_POINT ( 'NONE',  ( -33.65005778919723411, -23.96119346886880308, -0.6495511937832006977 ) ) ;
#67103 = CARTESIAN_POINT ( 'NONE',  ( -90.52287095715006160, -24.99132157543165889, 2.256160258750667502 ) ) ;
#67104 = VERTEX_POINT ( 'NONE', #36204 ) ;
#67105 = CARTESIAN_POINT ( 'NONE',  ( -10.82925958622295859, 16.30987832687952022, 11.49999999999999645 ) ) ;
#67106 = CARTESIAN_POINT ( 'NONE',  ( -66.62287095715002749, -23.96177878511307568, 10.65340807706330217 ) ) ;
#67107 = CARTESIAN_POINT ( 'NONE',  ( 31.59111626279633711, -6.376774720514426953, 16.27760796525321751 ) ) ;
#67108 = EDGE_CURVE ( 'NONE', #38334, #20641, #6677, .T. ) ;
#67109 = ORIENTED_EDGE ( 'NONE', *, *, #37866, .T. ) ;
#67110 = CARTESIAN_POINT ( 'NONE',  ( -97.52287095715001897, -24.34917612406837861, 0.1852690917426576545 ) ) ;
#67111 = CARTESIAN_POINT ( 'NONE',  ( -99.33961253015885973, -25.31506754800236791, 5.119446277803796796 ) ) ;
#67112 = CARTESIAN_POINT ( 'NONE',  ( 0.8635838190919263857, -3.990505948720460605, -8.999999999999998224 ) ) ;
#67113 = CARTESIAN_POINT ( 'NONE',  ( -40.62287095715003460, -24.51254535404254398, 9.355368623467652966 ) ) ;
#67115 = ADVANCED_FACE ( 'NONE', ( #97593 ), #61545, .F. ) ;
#67114 = CARTESIAN_POINT ( 'NONE',  ( -18.83419513347712737, -5.836681878196540829, -1.500000000000002220 ) ) ;
#67116 = VERTEX_POINT ( 'NONE', #92464 ) ;
#67117 = DIRECTION ( 'NONE',  ( 0.000000000000000000, -2.173523156925979975E-06, 0.9999999999976378895 ) ) ;
#67118 = CARTESIAN_POINT ( 'NONE',  ( -57.52287095715005449, -23.47596703998600631, 11.44779298504228926 ) ) ;
#67119 = ADVANCED_FACE ( 'NONE', ( #93969 ), #24462, .T. ) ;
#67120 = CALENDAR_DATE ( 2026, 9, 10 ) ;
#67121 = ORIENTED_EDGE ( 'NONE', *, *, #29868, .T. ) ;
#67122 = CARTESIAN_POINT ( 'NONE',  ( -103.5228709571500758, -29.50250243563736774, 8.947779886222138046 ) ) ;
#67123 = CARTESIAN_POINT ( 'NONE',  ( -84.52287095715007581, -23.48783264082477018, -1.443836473390090802 ) ) ;
#67124 = CARTESIAN_POINT ( 'NONE',  ( -69.62287095715004170, -23.72747288104441665, -1.053458166803662444 ) ) ;
#67125 = CARTESIAN_POINT ( 'NONE',  ( -84.52287095715006160, -29.50248528299804818, 1.056150453629038477 ) ) ;
#67126 = CARTESIAN_POINT ( 'NONE',  ( -6.815415664272417295, -6.376774720514410077, 19.46427715384223234 ) ) ;
#67127 = CARTESIAN_POINT ( 'NONE',  ( -70.35895856474228083, -25.24515042133736031, 5.313173755051356473 ) ) ;
#67128 = CARTESIAN_POINT ( 'NONE',  ( -91.52287095715000476, -24.33927499327855060, 9.819080762295806508 ) ) ;
#67129 = CARTESIAN_POINT ( 'NONE',  ( 19.20567810191101898, 5.375360269454119155, 11.49999999999998934 ) ) ;
#67130 = B_SPLINE_CURVE_WITH_KNOTS ( 'NONE', 3,
 ( #85927, #39742, #70700, #76786, #1195, #7289 ),
 .UNSPECIFIED., .F., .F.,
 ( 4, 2, 4 ),
 ( 0.000000000000000000, 0.001380901958385383774, 0.002761803916770767548 ),
 .UNSPECIFIED. ) ;
#67131 = AXIS2_PLACEMENT_3D ( 'NONE', #18459, #41818, #49431 ) ;
#67132 = CARTESIAN_POINT ( 'NONE',  ( -71.55620429048337883, -23.47593901973091235, -1.443836447539006196 ) ) ;
#67133 = CARTESIAN_POINT ( 'NONE',  ( -0.0004653795375827224552, -23.04397529616130313, 5.579469812630287073 ) ) ;
#67134 = VERTEX_POINT ( 'NONE', #8746 ) ;
#67135 = DIRECTION ( 'NONE',  ( -0.7071067811865507924, -0.000000000000000000, -0.7071067811865442421 ) ) ;
#67136 = CARTESIAN_POINT ( 'NONE',  ( 4.647438682898014761, -5.876774720514417183, 20.26932200457894950 ) ) ;
#67137 = EDGE_CURVE ( 'NONE', #18856, #94609, #63048, .T. ) ;
#67138 = VECTOR ( 'NONE', #73758, 1000.000000000000000 ) ;
#67139 = CARTESIAN_POINT ( 'NONE',  ( -119.5920062970955087, -23.73766607897670511, -1.055555164236450238 ) ) ;
#67140 = CARTESIAN_POINT ( 'NONE',  ( -80.60939578119689486, -23.48786465467241413, 11.44779295918254824 ) ) ;
#67141 = CARTESIAN_POINT ( 'NONE',  ( -49.74369414166533687, -25.31543073408252909, 4.940877929217667663 ) ) ;
#67142 = CARTESIAN_POINT ( 'NONE',  ( -81.51309679017218457, -23.96119346886881019, -0.6495511937831893734 ) ) ;
#67143 = EDGE_CURVE ( 'NONE', #79632, #36107, #39684, .T. ) ;
#67144 = CARTESIAN_POINT ( 'NONE',  ( 8.160000000000000142, -2.191226316053958875E-18, 2.701633758479787833E-17 ) ) ;
#67145 = B_SPLINE_CURVE_WITH_KNOTS ( 'NONE', 3,
 ( #21117, #44980, #37854, #75905 ),
 .UNSPECIFIED., .F., .F.,
 ( 4, 4 ),
 ( 0.6492381622116810691, 0.6502389092524463177 ),
 .UNSPECIFIED. ) ;
#67146 = CARTESIAN_POINT ( 'NONE',  ( -1.428094109758638819, -6.376774720514415407, 20.04104409779160179 ) ) ;
#67147 = ORIENTED_EDGE ( 'NONE', *, *, #8547, .F. ) ;
#67148 = CARTESIAN_POINT ( 'NONE',  ( -2.243088942307695177, -5.876774720514409189, 19.14743589743590491 ) ) ;
#67149 = CARTESIAN_POINT ( 'NONE',  ( 5.864177746775673050, -5.876774720514425177, 21.69926562011473337 ) ) ;
#67150 = ORIENTED_EDGE ( 'NONE', *, *, #21732, .T. ) ;
#67151 = CARTESIAN_POINT ( 'NONE',  ( -11.13811422090317294, 16.88724661786912762, -1.500000000000002220 ) ) ;
#67152 = CARTESIAN_POINT ( 'NONE',  ( -69.45360722279276899, -25.31510505358946261, 5.121476220657646294 ) ) ;
#67153 = FACE_OUTER_BOUND ( 'NONE', #90106, .T. ) ;
#67154 = DIRECTION ( 'NONE',  ( 1.000000000000000000, 0.000000000000000000, -0.000000000000000000 ) ) ;
#67155 = ORIENTED_EDGE ( 'NONE', *, *, #21262, .F. ) ;
#67156 = CARTESIAN_POINT ( 'NONE',  ( -79.10627061423527095, -25.31353510145896024, 5.240107987869434325 ) ) ;
#67157 = DIRECTION ( 'NONE',  ( -3.773278334453079618E-23, 0.9999999999976377785, 2.173523156925979975E-06 ) ) ;
#67158 = CARTESIAN_POINT ( 'NONE',  ( 12.62869658624171976, -15.57725692549414376, -1.500000000000002220 ) ) ;
#67159 = CARTESIAN_POINT ( 'NONE',  ( 19.96068868648078620, -6.529529906025321573, 11.49999999999999645 ) ) ;
#67160 = FACE_OUTER_BOUND ( 'NONE', #93114, .T. ) ;
#67161 = CARTESIAN_POINT ( 'NONE',  ( -70.63765949830232671, -24.40133493613049964, 9.663955038902802386 ) ) ;
#67162 = CARTESIAN_POINT ( 'NONE',  ( 11.82310115920509830, 18.66461490495635545, -1.500000000000002220 ) ) ;
#67163 = DIRECTION ( 'NONE',  ( 0.000000000000000000, 0.000000000000000000, 1.000000000000000000 ) ) ;
#67164 = DIRECTION ( 'NONE',  ( -1.000000000000000000, -3.773278334444166432E-23, -8.201307841325785021E-29 ) ) ;
#67165 = CARTESIAN_POINT ( 'NONE',  ( -50.02027282914984596, -25.27344770931672358, 3.346181230627190306 ) ) ;
#67166 = VERTEX_POINT ( 'NONE', #71150 ) ;
#67167 = CARTESIAN_POINT ( 'NONE',  ( -99.80308396037207785, -25.14437514330485257, 2.967792536799680470 ) ) ;
#67168 = B_SPLINE_SURFACE_WITH_KNOTS ( 'NONE', 3, 1, ( 
 ( #65331, #3418 ),
 ( #27735, #33846 ),
 ( #26236, #19610 ),
 ( #33337, #73907 ),
 ( #35356, #89137 ),
 ( #12003, #64834 ),
 ( #96743, #2916 ),
 ( #72423, #50573 ),
 ( #25733, #95745 ),
 ( #57209, #88142 ),
 ( #18611, #4405 ),
 ( #3913, #66317 ),
 ( #20113, #49585 ),
 ( #42481, #80519 ),
 ( #10006, #26735 ),
 ( #11011, #40964 ),
 ( #41978, #71924 ),
 ( #72920, #2408 ),
 ( #96251, #57697 ),
 ( #88642, #19112 ),
 ( #50084, #81024 ),
 ( #64329, #95246 ),
 ( #56707, #87639 ) ),
 .UNSPECIFIED., .F., .F., .F.,
 ( 4, 1, 1, 1, 1, 1, 1, 1, 1, 1, 1, 1, 1, 1, 1, 1, 1, 1, 1, 1, 4 ),
 ( 2, 2 ),
 ( 0.000000000000000000, 0.06038661931106217851, 0.1208832485859971800, 0.1827546186251399196, 0.2478110297583515365, 0.2812991000432492061, 0.3150876241506573860, 0.3497023955502753800, 0.3848565811185556962, 0.4209661972261026786, 0.4585111882611394019, 0.4971747221273126738, 0.5376020478662696389, 0.5805030184200120624, 0.6274675400267047953, 0.6783882095592436157, 0.7339832205925607145, 0.7937467045508352914, 0.8577136721607322434, 0.9266978643613863476, 1.000000000000000000 ),
 ( 0.000000000000000000, 1.000000000000000000 ),
 .UNSPECIFIED. ) ;
#67169 = DIRECTION ( 'NONE',  ( 0.000000000000000000, 0.000000000000000000, -1.000000000000000000 ) ) ;
#67170 = ORIENTED_EDGE ( 'NONE', *, *, #7791, .F. ) ;
#67171 = ORIENTED_EDGE ( 'NONE', *, *, #47078, .F. ) ;
#67172 = CARTESIAN_POINT ( 'NONE',  ( -55.52287095715009002, -24.63287334234179582, 0.9662140553045320823 ) ) ;
#67173 = CARTESIAN_POINT ( 'NONE',  ( -44.52287095715006160, -29.50250243563736774, 8.947779886222148704 ) ) ;
#67174 = CARTESIAN_POINT ( 'NONE',  ( -89.62287095715002749, -23.48783264082478439, -1.443836473390063713 ) ) ;
#67175 = CARTESIAN_POINT ( 'NONE',  ( 10.47388184937329214, 17.72644800832989986, -1.500000000000002220 ) ) ;
#67176 = CARTESIAN_POINT ( 'NONE',  ( 5.689979955356517571, -20.79666814084963278, 11.49999999999999645 ) ) ;
#67177 = ORIENTED_EDGE ( 'NONE', *, *, #40260, .T. ) ;
#67178 = CARTESIAN_POINT ( 'NONE',  ( -91.62826352414620601, -24.34968618360934656, 0.1864209137778843617 ) ) ;
#67179 = CARTESIAN_POINT ( 'NONE',  ( -53.62287095715005592, -23.47596703998600276, 11.44779298504227683 ) ) ;
#67180 = CARTESIAN_POINT ( 'NONE',  ( -129.6228709571500133, -23.96127896941632685, -0.6493128931037762674 ) ) ;
#67181 = CARTESIAN_POINT ( 'NONE',  ( 10.24050353823403192, -19.87907451059620456, 11.49999999999998934 ) ) ;
#67182 = CARTESIAN_POINT ( 'NONE',  ( -34.52287095715005449, -23.73934037231755312, 11.05740245334329153 ) ) ;
#67183 = CARTESIAN_POINT ( 'NONE',  ( -84.59526730009702078, -23.96119346886880663, -0.6495511937832096905 ) ) ;
#67184 = VERTEX_POINT ( 'NONE', #1135 ) ;
#67185 = DIRECTION ( 'NONE',  ( -3.773278334453079030E-23, 0.9999999999976377785, 2.173523156925979128E-06 ) ) ;
#67186 = CARTESIAN_POINT ( 'NONE',  ( 31.24279708945211098, 4.510509370595455536, 1.827416827591516357 ) ) ;
#67187 = CARTESIAN_POINT ( 'NONE',  ( 14.99592430652175956, 14.54719766626331889, -1.500000000000002220 ) ) ;
#67188 = ORIENTED_EDGE ( 'NONE', *, *, #3748, .F. ) ;
#67189 = VECTOR ( 'NONE', #88223, 1000.000000000000000 ) ;
#67191 = EDGE_LOOP ( 'NONE', ( #72906, #9647 ) ) ;
#67190 = CARTESIAN_POINT ( 'NONE',  ( 6.660000000000001030, -9.074990544709798712, -0.7360493640965781736 ) ) ;
#67192 = ORIENTED_EDGE ( 'NONE', *, *, #85544, .F. ) ;
#67193 = CARTESIAN_POINT ( 'NONE',  ( -100.5869784172404877, -24.73531770709095312, 8.716586749053508498 ) ) ;
#67194 = CARTESIAN_POINT ( 'NONE',  ( -21.09505027744838657, -1.104435277493458045, -1.500000000000002220 ) ) ;
#67195 = ORIENTED_EDGE ( 'NONE', *, *, #42780, .T. ) ;
#67196 = CARTESIAN_POINT ( 'NONE',  ( -94.52287095715003318, -24.66019654487199730, 8.947790411086124607 ) ) ;
#67198 = EDGE_CURVE ( 'NONE', #12570, #65127, #83546, .T. ) ;
#67197 = CARTESIAN_POINT ( 'NONE',  ( -102.6228709571500701, -24.50321055353805377, 9.387540953477524042 ) ) ;
#67199 = LINE ( 'NONE', #52962, #20518 ) ;
#67200 = EDGE_CURVE ( 'NONE', #39942, #77983, #81627, .T. ) ;
#67201 = CARTESIAN_POINT ( 'NONE',  ( -76.50396469980680081, -24.35071581493543036, 9.817618358456028815 ) ) ;
#67202 = CARTESIAN_POINT ( 'NONE',  ( 7.275731542451676859, -6.376774720514415407, 20.06332870126568224 ) ) ;
#67203 = CARTESIAN_POINT ( 'NONE',  ( 17.47290450027814757, -12.96279059203284767, -1.500000000000002220 ) ) ;
#67204 = DIRECTION ( 'NONE',  ( 0.000000000000000000, 0.000000000000000000, -1.000000000000000000 ) ) ;
#67206 = EDGE_LOOP ( 'NONE', ( #80899, #33832, #48573, #92144 ) ) ;
#67205 = CARTESIAN_POINT ( 'NONE',  ( 13.76814385225720372, 17.53657229028232223, 11.49999999999999645 ) ) ;
#67207 = FACE_OUTER_BOUND ( 'NONE', #9727, .T. ) ;
#67208 = CARTESIAN_POINT ( 'NONE',  ( -27.25988310792305214, 5.965225279485572685, 30.32664379231667695 ) ) ;
#67209 = CARTESIAN_POINT ( 'NONE',  ( -101.5228709571500758, -23.47593901973090524, -1.443836447538996426 ) ) ;
#67210 = VERTEX_POINT ( 'NONE', #22937 ) ;
#67211 = AXIS2_PLACEMENT_3D ( 'NONE', #34845, #12497, #97733 ) ;
#67212 = ADVANCED_FACE ( 'NONE', ( #55428 ), #25249, .T. ) ;
#67213 = EDGE_CURVE ( 'NONE', #39944, #16912, #69648, .T. ) ;
#67214 = VERTEX_POINT ( 'NONE', #15339 ) ;
#67215 = VERTEX_POINT ( 'NONE', #7229 ) ;
#67216 = DIRECTION ( 'NONE',  ( 1.000000000000000000, 1.734723475976806848E-16, 0.000000000000000000 ) ) ;
#67217 = FACE_OUTER_BOUND ( 'NONE', #28341, .T. ) ;
#67218 = CARTESIAN_POINT ( 'NONE',  ( -52.58953762381672448, -23.48786465467240703, 11.44779295918255002 ) ) ;
#67219 = CARTESIAN_POINT ( 'NONE',  ( -67.62287095715005592, -23.48786465467241058, 11.44779295918254647 ) ) ;
#67220 = CARTESIAN_POINT ( 'NONE',  ( -16.24122463664219396, 10.56255597858309869, 11.49999999999998934 ) ) ;
#67221 = EDGE_CURVE ( 'NONE', #74870, #396, #32575, .T. ) ;
#67222 = DIRECTION ( 'NONE',  ( 1.000000000000000000, -0.000000000000000000, -0.000000000000000000 ) ) ;
#67223 = EDGE_LOOP ( 'NONE', ( #19836, #32330, #34987, #36593 ) ) ;
#67224 = CARTESIAN_POINT ( 'NONE',  ( -12.28997142660015740, 14.97987746540053422, 11.49999999999999645 ) ) ;
#67225 = CARTESIAN_POINT ( 'NONE',  ( -47.62287095715006302, -23.47596703998600276, 11.44779298504227505 ) ) ;
#67226 = VERTEX_POINT ( 'NONE', #45807 ) ;
#67227 = FACE_OUTER_BOUND ( 'NONE', #27703, .T. ) ;
#67228 = FACE_OUTER_BOUND ( 'NONE', #53338, .T. ) ;
#67229 = CARTESIAN_POINT ( 'NONE',  ( -65.52287095715006160, -23.47596703998600631, 11.44779298504228748 ) ) ;
#67230 = CARTESIAN_POINT ( 'NONE',  ( -36.52287095715006870, -24.35013146730203815, 9.818937971375104823 ) ) ;
#67231 = CARTESIAN_POINT ( 'NONE',  ( 16.12930680145378304, -11.13525102954884893, 11.49999999999998934 ) ) ;
#67232 = CARTESIAN_POINT ( 'NONE',  ( -46.58180868254443396, -24.51314013834315020, 0.6176544820404077374 ) ) ;
#67233 = ORIENTED_EDGE ( 'NONE', *, *, #25735, .T. ) ;
#67234 = AXIS2_PLACEMENT_3D ( 'NONE', #48147, #47646, #80082 ) ;
#67235 = CARTESIAN_POINT ( 'NONE',  ( -16.67190562677319932, -13.68652177170558204, -1.500000000000002220 ) ) ;
#67236 = CARTESIAN_POINT ( 'NONE',  ( -33.62373659705630757, -24.66019654487198665, 8.947790411086133489 ) ) ;
#67237 = CARTESIAN_POINT ( 'NONE',  ( -70.78633892220865675, -25.12219122934108384, 7.001279615086478003 ) ) ;
#67238 = DIRECTION ( 'NONE',  ( -3.773278334453079030E-23, 0.9999999999976377785, 2.173523156925979128E-06 ) ) ;
#67239 = DIRECTION ( 'NONE',  ( 0.000000000000000000, -1.000000000000000000, 0.000000000000000000 ) ) ;
#67240 = CARTESIAN_POINT ( 'NONE',  ( -0.3492834940180428727, 22.98956000712751546, -1.500000000000002220 ) ) ;
#67241 = APPLICATION_PROTOCOL_DEFINITION ( 'international standard', 'config_control_design', 1994, #35596 ) ;
#67242 = CARTESIAN_POINT ( 'NONE',  ( -49.57749393427013729, -24.65952944569304606, 1.056160979905696129 ) ) ;
#67243 = CARTESIAN_POINT ( 'NONE',  ( -8.513533612778267923, 18.29693335657625042, 11.49999999999999645 ) ) ;
#67244 = CARTESIAN_POINT ( 'NONE',  ( -109.3293036055952143, -25.10927482606251715, 3.229615370203269720 ) ) ;
#67245 = DIRECTION ( 'NONE',  ( -3.773278334453079030E-23, 0.9999999999976377785, 2.173523156925979128E-06 ) ) ;
#67246 = LINE ( 'NONE', #44905, #13366 ) ;
#67247 = CARTESIAN_POINT ( 'NONE',  ( 0.000000000000000000, -1.473225279485573802, 0.000000000000000000 ) ) ;
#67248 = CARTESIAN_POINT ( 'NONE',  ( -111.2332490450528582, -25.18425693141708521, 3.802242211139469141 ) ) ;
#67249 = CARTESIAN_POINT ( 'NONE',  ( -14.63867168220055781, -13.42826565525684579, -1.500000000000002220 ) ) ;
#67250 = CARTESIAN_POINT ( 'NONE',  ( 2.449489742783178770, -16.94322527948557422, 2.499999999999999556 ) ) ;
#67251 = CARTESIAN_POINT ( 'NONE',  ( -19.69265041987409859, 1.759638296948408787, -1.500000000000002220 ) ) ;
#67252 = LINE ( 'NONE', #36297, #91271 ) ;
#67253 = EDGE_CURVE ( 'NONE', #50923, #71272, #18714, .T. ) ;
#67254 = CARTESIAN_POINT ( 'NONE',  ( -1.041963229364719634, -6.376774720514417183, 20.24089781925592746 ) ) ;
#67255 = CARTESIAN_POINT ( 'NONE',  ( -28.98875734969026396, 5.965225279485572685, 0.1180228001186258285 ) ) ;
#67256 = CARTESIAN_POINT ( 'NONE',  ( 20.67342648114324533, -1.018679444107209342, 11.49999999999999645 ) ) ;
#67257 = DIRECTION ( 'NONE',  ( -3.773278334453079618E-23, 0.9999999999976377785, 2.173523156925979975E-06 ) ) ;
#67258 = EDGE_CURVE ( 'NONE', #70398, #66681, #61156, .T. ) ;
#67259 = VECTOR ( 'NONE', #59392, 1000.000000000000000 ) ;
#67261 = B_SPLINE_CURVE_WITH_KNOTS ( 'NONE', 3,
 ( #52322, #5636, #98975, #83257, #73657, #12237 ),
 .UNSPECIFIED., .F., .F.,
 ( 4, 2, 4 ),
 ( 1.570887131794638196E-05, 0.001396322306279762591, 0.002776935741241578874 ),
 .UNSPECIFIED. ) ;
#67260 = DIRECTION ( 'NONE',  ( 0.000000000000000000, 1.000000000000000000, 0.000000000000000000 ) ) ;
#67262 = CARTESIAN_POINT ( 'NONE',  ( -44.62287095715004881, -23.47596703998600631, 11.44779298504227505 ) ) ;
#67263 = CARTESIAN_POINT ( 'NONE',  ( 20.10346781357453949, 10.43426432342431553, 11.49999999999999645 ) ) ;
#67264 = VERTEX_POINT ( 'NONE', #16345 ) ;
#67265 = CARTESIAN_POINT ( 'NONE',  ( -0.3544984435505275644, -5.876774720514409189, 19.15251819062245531 ) ) ;
#67266 = CARTESIAN_POINT ( 'NONE',  ( 30.61558003201036726, 3.638743767327229151, 27.34189434213806535 ) ) ;
#67267 = FACE_OUTER_BOUND ( 'NONE', #56291, .T. ) ;
#67268 = AXIS2_PLACEMENT_3D ( 'NONE', #30962, #53314, #69029 ) ;
#67269 = CARTESIAN_POINT ( 'NONE',  ( -0.02075734969026423599, 5.965225279485572685, -0.08597719988137648983 ) ) ;
#67270 = ORIENTED_EDGE ( 'NONE', *, *, #82922, .F. ) ;
#67271 = CIRCLE ( 'NONE', #23482, 3.060000000000000053 ) ;
#67272 = ORIENTED_EDGE ( 'NONE', *, *, #45630, .T. ) ;
#67273 = CARTESIAN_POINT ( 'NONE',  ( 8.499999999999989342, 18.74999999999999645, 2.100000000000000089 ) ) ;
#67274 = CARTESIAN_POINT ( 'NONE',  ( 22.85402955525884394, -0.1436109537974766814, 11.49999999999998934 ) ) ;
#67275 = CARTESIAN_POINT ( 'NONE',  ( -29.52199330670222110, -23.40092668919113450, -1.443836171194816886 ) ) ;
#67276 = CARTESIAN_POINT ( 'NONE',  ( -11.65619939812097527, 18.16556634249905855, -1.500000000000002220 ) ) ;
#67277 = DIRECTION ( 'NONE',  ( 0.000000000000000000, 0.000000000000000000, -1.000000000000000000 ) ) ;
#67278 = CARTESIAN_POINT ( 'NONE',  ( -65.52287095715006160, -25.00158670708909625, 2.256160236439166411 ) ) ;
#67279 = CARTESIAN_POINT ( 'NONE',  ( -20.59131556071872282, -9.131246169528550283, 11.49999999999999645 ) ) ;
#67280 = ORIENTED_EDGE ( 'NONE', *, *, #32717, .F. ) ;
#67281 = CARTESIAN_POINT ( 'NONE',  ( -70.27422298781921484, -25.24754245836512467, 4.851635288312657224 ) ) ;
#67282 = CARTESIAN_POINT ( 'NONE',  ( 17.26801960494244881, -13.64313956103151071, -1.500000000000002220 ) ) ;
#67283 = CARTESIAN_POINT ( 'NONE',  ( -64.52287095715009002, -23.72747288104470087, -1.053458166803226126 ) ) ;
#67284 = CARTESIAN_POINT ( 'NONE',  ( -27.75582626765746497, -25.21724993721676711, 7.602200292291605876 ) ) ;
#67285 = ORIENTED_EDGE ( 'NONE', *, *, #81631, .F. ) ;
#67286 = DIRECTION ( 'NONE',  ( -1.000000000000000000, 0.000000000000000000, -0.000000000000000000 ) ) ;
#67287 = CARTESIAN_POINT ( 'NONE',  ( -90.51647507451308172, -23.85049219812686871, 10.88485053497527844 ) ) ;
#67288 = ORIENTED_EDGE ( 'NONE', *, *, #24438, .T. ) ;
#67289 = CARTESIAN_POINT ( 'NONE',  ( -108.6228709571500559, -23.47593901973091235, -1.443836447538999312 ) ) ;
#67290 = VERTEX_POINT ( 'NONE', #47311 ) ;
#67291 = EDGE_LOOP ( 'NONE', ( #51974, #55374, #98749, #48320 ) ) ;
#67292 = CARTESIAN_POINT ( 'NONE',  ( -65.52287095715006160, -23.84047902841601640, -0.8780736468305708753 ) ) ;
#67293 = LINE ( 'NONE', #82990, #58318 ) ;
#67294 = CARTESIAN_POINT ( 'NONE',  ( -57.57870244156648454, -24.65952944569304606, 1.056160979905698571 ) ) ;
#67295 = CARTESIAN_POINT ( 'NONE',  ( 19.51578053514377586, 5.923290232019536639, -1.500000000000002220 ) ) ;
#67296 = ORIENTED_EDGE ( 'NONE', *, *, #99355, .F. ) ;
#67297 = CARTESIAN_POINT ( 'NONE',  ( -2.959136224476847765, -6.376774720514413630, 19.53857357749110335 ) ) ;
#67298 = CARTESIAN_POINT ( 'NONE',  ( -92.52287095715011844, -23.96177878511310055, 10.65340807706329507 ) ) ;
#67299 = LINE ( 'NONE', #73414, #51350 ) ;
#67300 = CARTESIAN_POINT ( 'NONE',  ( -44.62287095715004881, -29.50248528299804818, 1.056150453629031594 ) ) ;
#67301 = VERTEX_POINT ( 'NONE', #55934 ) ;
#67302 = DIRECTION ( 'NONE',  ( 3.773278334444167608E-23, -1.000000000000000000, 0.000000000000000000 ) ) ;
#67303 = CARTESIAN_POINT ( 'NONE',  ( -28.27652290204276042, -25.26248058196737745, 8.166124215670606645 ) ) ;
#67304 = AXIS2_PLACEMENT_3D ( 'NONE', #33548, #49794, #64534 ) ;
#67305 = CARTESIAN_POINT ( 'NONE',  ( 5.171613189315443115, 20.13430294385436881, -1.500000000000002220 ) ) ;
#67306 = VERTEX_POINT ( 'NONE', #41203 ) ;
#67308 = ORIENTED_EDGE ( 'NONE', *, *, #48405, .T. ) ;
#67307 = LINE ( 'NONE', #58691, #83160 ) ;
#67309 = FACE_OUTER_BOUND ( 'NONE', #40963, .T. ) ;
#67310 = CARTESIAN_POINT ( 'NONE',  ( -56.55620429048342146, -23.47596703998600276, 11.44779298504227505 ) ) ;
#67311 = ORIENTED_EDGE ( 'NONE', *, *, #91799, .F. ) ;
#67312 = ORIENTED_EDGE ( 'NONE', *, *, #88779, .F. ) ;
#67313 = CARTESIAN_POINT ( 'NONE',  ( 2.872281323269014752, -1.473225279485573358, 1.999999999999999556 ) ) ;
#67314 = ADVANCED_FACE ( 'NONE', ( #87363 ), #4138, .F. ) ;
#67315 = CARTESIAN_POINT ( 'NONE',  ( -64.52287095715010423, -24.51387760970724727, 9.387446482453412955 ) ) ;
#67316 = CARTESIAN_POINT ( 'NONE',  ( -22.05275734969026047, 5.965225279485572685, 31.02402280011862246 ) ) ;
#67317 = CARTESIAN_POINT ( 'NONE',  ( -70.55843555340263151, -25.31201593592794907, 5.327474662351524337 ) ) ;
#67319 = ORIENTED_EDGE ( 'NONE', *, *, #63767, .T. ) ;
#67318 = CARTESIAN_POINT ( 'NONE',  ( -12.03526013704878039, -18.61824004984164560, 11.49999999999999645 ) ) ;
#67320 = LINE ( 'NONE', #28750, #10686 ) ;
#67321 = EDGE_CURVE ( 'NONE', #20076, #92445, #75425, .T. ) ;
#67322 = CARTESIAN_POINT ( 'NONE',  ( 21.37280783159109276, 7.349196219051140844, -1.500000000000002220 ) ) ;
#67323 = ADVANCED_FACE ( 'NONE', ( #81253 ), #96003, .T. ) ;
#67325 = ORIENTED_EDGE ( 'NONE', *, *, #36031, .F. ) ;
#67324 = CARTESIAN_POINT ( 'NONE',  ( -115.5550126193648737, -24.15602025860897584, 10.28564288303533836 ) ) ;
#67326 = ADVANCED_FACE ( 'NONE', ( #11735 ), #33583, .T. ) ;
#67327 = ORIENTED_EDGE ( 'NONE', *, *, #16312, .T. ) ;
#67328 = EDGE_CURVE ( 'NONE', #69030, #75743, #42712, .T. ) ;
#67329 = CARTESIAN_POINT ( 'NONE',  ( -69.62287095715005592, -23.47593901973091235, -1.443836447539006196 ) ) ;
#67330 = AXIS2_PLACEMENT_3D ( 'NONE', #83221, #90842, #97456 ) ;
#67331 = VECTOR ( 'NONE', #32691, 1000.000000000000000 ) ;
#67332 = CARTESIAN_POINT ( 'NONE',  ( 13.91401389203221406, -6.376774720514426953, 158.0376437107427137 ) ) ;
#67333 = VERTEX_POINT ( 'NONE', #71649 ) ;
#67334 = CARTESIAN_POINT ( 'NONE',  ( -126.5228709571500332, -24.51283580621365843, 0.6167428607019861397 ) ) ;
#67335 = CARTESIAN_POINT ( 'NONE',  ( -21.62769966018443313, 5.350386031573528989, -1.500000000000002220 ) ) ;
#67336 = CIRCLE ( 'NONE', #9021, 2.249999999999998668 ) ;
#67337 = FACE_OUTER_BOUND ( 'NONE', #57459, .T. ) ;
#67338 = EDGE_CURVE ( 'NONE', #71801, #9237, #13855, .T. ) ;
#67339 = VECTOR ( 'NONE', #34737, 1000.000000000000000 ) ;
#67340 = EDGE_LOOP ( 'NONE', ( #18247, #60835, #64356, #69748 ) ) ;
#67341 = DIRECTION ( 'NONE',  ( -0.06975647374412549673, -0.9975640502598241977, 0.000000000000000000 ) ) ;
#67342 = DIRECTION ( 'NONE',  ( 0.000000000000000000, -0.000000000000000000, 1.000000000000000000 ) ) ;
#67343 = CARTESIAN_POINT ( 'NONE',  ( -103.6228709571500559, -29.50248528299804818, 1.056150453629042030 ) ) ;
#67344 = AXIS2_PLACEMENT_3D ( 'NONE', #56439, #95480, #25463 ) ;
#67345 = LINE ( 'NONE', #53990, #98171 ) ;
#67346 = PLANE ( 'NONE',  #59390 ) ;
#67347 = CARTESIAN_POINT ( 'NONE',  ( -19.51626497420292239, -0.3564122556526727048, 11.49999999999998934 ) ) ;
#67348 = CARTESIAN_POINT ( 'NONE',  ( -20.95461191387366284, 4.708766595171775649, 11.49999999999998934 ) ) ;
#67349 = B_SPLINE_CURVE_WITH_KNOTS ( 'NONE', 3,
 ( #89484, #89983, #19465, #20456, #74747, #51429 ),
 .UNSPECIFIED., .F., .F.,
 ( 4, 2, 4 ),
 ( 0.000000000000000000, 0.001380764517854761496, 0.002761529035709522992 ),
 .UNSPECIFIED. ) ;
#67350 = CARTESIAN_POINT ( 'NONE',  ( -2.599001758237162285, -6.376774720514413630, 19.60308799987317485 ) ) ;
#67351 = DIRECTION ( 'NONE',  ( -1.709749016398430297E-16, -0.7071067811865436870, 0.7071067811865513475 ) ) ;
#67352 = CARTESIAN_POINT ( 'NONE',  ( -126.6228709571500559, -29.50248528299804818, 1.056150453629047137 ) ) ;
#67353 = CARTESIAN_POINT ( 'NONE',  ( 18.64237364862239943, 13.12531859369229359, -1.500000000000002220 ) ) ;
#67354 = DATE_AND_TIME ( #59743, #53768 ) ;
#67355 = CARTESIAN_POINT ( 'NONE',  ( -39.52287095715006870, -24.64898659630528144, 1.056161002820819261 ) ) ;
#67356 = CARTESIAN_POINT ( 'NONE',  ( -29.24636659181000198, -29.50249372523856195, 4.940277699495910113 ) ) ;
#67357 = CARTESIAN_POINT ( 'NONE',  ( 10.17626895549074817, -17.22257424524772418, 11.49999999999999645 ) ) ;
#67358 = DIRECTION ( 'NONE',  ( -0.9831680378442392287, -0.000000000000000000, -0.1827036106964188000 ) ) ;
#67359 = CARTESIAN_POINT ( 'NONE',  ( -43.52287095715006160, -24.65952944569304606, 1.056160979905691910 ) ) ;
#67360 = CARTESIAN_POINT ( 'NONE',  ( 2.499999999999993783, 4.999999999999997335, 0.000000000000000000 ) ) ;
#67361 = ORIENTED_EDGE ( 'NONE', *, *, #50284, .F. ) ;
#67362 = CARTESIAN_POINT ( 'NONE',  ( -83.52287095715001897, -24.66019654487199375, 8.947790411086122830 ) ) ;
#67363 = EDGE_CURVE ( 'NONE', #46021, #42205, #17353, .T. ) ;
#67364 = DIRECTION ( 'NONE',  ( 0.000000000000000000, 0.000000000000000000, 1.000000000000000000 ) ) ;
#67365 = CARTESIAN_POINT ( 'NONE',  ( 12.24854465327799424, 17.96525243877979605, -1.500000000000002220 ) ) ;
#67366 = CARTESIAN_POINT ( 'NONE',  ( -88.88918693012689687, -25.26877915520014639, 5.947789088310639904 ) ) ;
#67367 = CARTESIAN_POINT ( 'NONE',  ( 18.72186718581493636, -5.619560887262019300, -1.500000000000002220 ) ) ;
#67368 = CARTESIAN_POINT ( 'NONE',  ( -4.495793269230770939, -6.376774720514410077, 19.27714342948718595 ) ) ;
#67369 = EDGE_CURVE ( 'NONE', #55695, #25101, #47852, .T. ) ;
#67370 = ORIENTED_EDGE ( 'NONE', *, *, #27940, .T. ) ;
#67371 = APPROVAL_DATE_TIME ( #36409, #42550 ) ;
#67372 = CIRCLE ( 'NONE', #99710, 1.699999999999999289 ) ;
#67373 = PLANE ( 'NONE',  #45148 ) ;
#67374 = LINE ( 'NONE', #98292, #49184 ) ;
#67375 = CARTESIAN_POINT ( 'NONE',  ( -19.38928925021375349, 6.733644070511561885, 11.49999999999999645 ) ) ;
#67376 = CARTESIAN_POINT ( 'NONE',  ( -49.85642534923032798, -25.30192753786928606, 5.303853196035516859 ) ) ;
#67377 = CARTESIAN_POINT ( 'NONE',  ( -40.52287095715005449, -23.48783264082476308, -1.443836473390097908 ) ) ;
#67378 = ORIENTED_EDGE ( 'NONE', *, *, #74616, .T. ) ;
#67379 = EDGE_CURVE ( 'NONE', #99263, #67734, #83743, .T. ) ;
#67380 = DIRECTION ( 'NONE',  ( -0.000000000000000000, -0.000000000000000000, 1.000000000000000000 ) ) ;
#67381 = CARTESIAN_POINT ( 'NONE',  ( 33.61456970919608978, 3.316774720514426900, -11.35828564741660962 ) ) ;
#67382 = CARTESIAN_POINT ( 'NONE',  ( 10.86264265030973952, 0.3587747205144257157, -28.64597719988137570 ) ) ;
#67383 = EDGE_CURVE ( 'NONE', #48489, #64351, #43204, .T. ) ;
#67384 = CARTESIAN_POINT ( 'NONE',  ( -61.62287095715002039, -24.33832256526968862, 0.1851278514119845120 ) ) ;
#67385 = EDGE_LOOP ( 'NONE', ( #52602, #79527, #54403, #23674 ) ) ;
#67386 = CARTESIAN_POINT ( 'NONE',  ( -109.6228709571500559, -29.50248528299804818, 1.056150453629043584 ) ) ;
#67387 = CARTESIAN_POINT ( 'NONE',  ( -22.27228905017084060, 5.866681652885556986, 11.49999999999999645 ) ) ;
#67388 = CARTESIAN_POINT ( 'NONE',  ( -10.92962168092244823, 19.99562239114850826, -1.500000000000002220 ) ) ;
#67389 = CARTESIAN_POINT ( 'NONE',  ( 3.206569032998081603, -6.376774720514424288, 21.19686455982786200 ) ) ;
#67390 = B_SPLINE_CURVE_WITH_KNOTS ( 'NONE', 3,
 ( #45808, #29079, #60053, #76241 ),
 .UNSPECIFIED., .F., .F.,
 ( 4, 4 ),
 ( 0.000000000000000000, 1.000000000000000000 ),
 .UNSPECIFIED. ) ;
#67391 = LINE ( 'NONE', #83087, #57705 ) ;
#67392 = CARTESIAN_POINT ( 'NONE',  ( 8.160000000000000142, 2.888964624466060727, -0.2527516539682188590 ) ) ;
#67393 = DIRECTION ( 'NONE',  ( 0.000000000000000000, 0.000000000000000000, 1.000000000000000000 ) ) ;
#67394 = CARTESIAN_POINT ( 'NONE',  ( -99.60147378138974261, -25.30157691793918318, 4.950471116695807972 ) ) ;
#67395 = CARTESIAN_POINT ( 'NONE',  ( 21.48171311866277122, -4.276277801222842179, -1.500000000000002220 ) ) ;
#67396 = CC_DESIGN_PERSON_AND_ORGANIZATION_ASSIGNMENT ( #29026, #59002, ( #11661 ) ) ;
#67397 = CARTESIAN_POINT ( 'NONE',  ( 6.830155907162054341, -5.876774720514427841, 21.76451523534627341 ) ) ;
#67398 = AXIS2_PLACEMENT_3D ( 'NONE', #61901, #8100, #484 ) ;
#67399 = CARTESIAN_POINT ( 'NONE',  ( -9.299999999999991829, 12.00000000000002309, 2.100000000000000089 ) ) ;
#67400 = CARTESIAN_POINT ( 'NONE',  ( -28.62287095715006657, -24.18442083929187092, 0.1849424278035973201 ) ) ;
#67401 = DIRECTION ( 'NONE',  ( -8.503546450866701308E-16, 0.000000000000000000, 1.000000000000000000 ) ) ;
#67402 = DIRECTION ( 'NONE',  ( 1.000000000000000000, -4.015979463811607402E-15, 0.000000000000000000 ) ) ;
#67403 = ORIENTED_EDGE ( 'NONE', *, *, #38222, .F. ) ;
#67404 = AXIS2_PLACEMENT_3D ( 'NONE', #49225, #57833, #18743 ) ;
#67405 = CARTESIAN_POINT ( 'NONE',  ( 1.124825640313904973, 20.40429917142216354, 11.49999999999998934 ) ) ;
#67406 = ORIENTED_EDGE ( 'NONE', *, *, #14244, .F. ) ;
#67407 = VECTOR ( 'NONE', #58504, 1000.000000000000114 ) ;
#67408 = ORIENTED_EDGE ( 'NONE', *, *, #45291, .T. ) ;
#67409 = EDGE_LOOP ( 'NONE', ( #49669, #15442, #39730, #12423 ) ) ;
#67410 = ORIENTED_EDGE ( 'NONE', *, *, #78715, .T. ) ;
#67411 = CARTESIAN_POINT ( 'NONE',  ( 15.83906049732654608, 16.74391201645830662, 11.49999999999998934 ) ) ;
#67412 = CARTESIAN_POINT ( 'NONE',  ( -88.62287095715004170, -29.50250243563736774, 8.947779886222139822 ) ) ;
#67413 = CARTESIAN_POINT ( 'NONE',  ( -3.766600276044322904, -19.90762401167813067, -1.500000000000002220 ) ) ;
#67414 = AXIS2_PLACEMENT_3D ( 'NONE', #28821, #36928, #60287 ) ;
#67415 = ORIENTED_EDGE ( 'NONE', *, *, #62332, .T. ) ;
#67416 = CARTESIAN_POINT ( 'NONE',  ( -29.27679109283166170, -24.91542385526720338, 7.636915180611340226 ) ) ;
#67417 = CARTESIAN_POINT ( 'NONE',  ( -29.49875734969026198, -0.3587747205144262708, 0.1180228001186258285 ) ) ;
#67418 = AXIS2_PLACEMENT_3D ( 'NONE', #66895, #73996, #51658 ) ;
#67419 = CARTESIAN_POINT ( 'NONE',  ( -95.58652457540902958, -24.73486907724918282, 1.287355809206966128 ) ) ;
#67420 = CARTESIAN_POINT ( 'NONE',  ( -99.54828946340249729, -24.51419770103158413, 9.386484678747176957 ) ) ;
#67422 = EDGE_LOOP ( 'NONE', ( #67308, #90323, #75989, #60301 ) ) ;
#67421 = CARTESIAN_POINT ( 'NONE',  ( 14.45597713831175035, -15.85640774750547344, 11.49999999999999645 ) ) ;
#67423 = CARTESIAN_POINT ( 'NONE',  ( -77.62287095715007013, -23.48783264082478794, -1.443836473390065933 ) ) ;
#67424 = ORIENTED_EDGE ( 'NONE', *, *, #280, .T. ) ;
#67425 = CARTESIAN_POINT ( 'NONE',  ( -10.81534556030752725, -17.66751395530895152, 11.49999999999998934 ) ) ;
#67426 = VERTEX_POINT ( 'NONE', #51815 ) ;
#67427 = CARTESIAN_POINT ( 'NONE',  ( -28.47400090564692832, -24.49516158990158843, 1.056161677404373611 ) ) ;
#67428 = ORIENTED_EDGE ( 'NONE', *, *, #65951, .T. ) ;
#67429 = DIRECTION ( 'NONE',  ( -0.000000000000000000, -1.000000000000000000, -0.000000000000000000 ) ) ;
#67430 = ORIENTED_EDGE ( 'NONE', *, *, #73979, .T. ) ;
#67431 = CARTESIAN_POINT ( 'NONE',  ( 9.933205088616889000, -18.45388779576350302, -1.500000000000002220 ) ) ;
#67432 = ADVANCED_FACE ( 'NONE', ( #97476 ), #12226, .F. ) ;
#67433 = CARTESIAN_POINT ( 'NONE',  ( 1.410849576418898632, -21.91845101833037290, 11.49999999999999645 ) ) ;
#67434 = CARTESIAN_POINT ( 'NONE',  ( -37.52201665554768795, -23.48786465467240347, 11.44779295918255357 ) ) ;
#67435 = CARTESIAN_POINT ( 'NONE',  ( -19.74168752133572724, 10.86179948771369297, -1.500000000000002220 ) ) ;
#67436 = CARTESIAN_POINT ( 'NONE',  ( -20.44905293368100985, -4.654758753755802836, -1.500000000000002220 ) ) ;
#67437 = CARTESIAN_POINT ( 'NONE',  ( 5.730633878096764278, -6.376774720514418959, 20.45679216967608838 ) ) ;
#67438 = CARTESIAN_POINT ( 'NONE',  ( -119.6284939267775798, -23.48786465467241769, 11.44779295918253581 ) ) ;
#67439 = CARTESIAN_POINT ( 'NONE',  ( 13.91401389203221406, 5.965225279485572685, 158.0376437107427137 ) ) ;
#67440 = ORIENTED_EDGE ( 'NONE', *, *, #83577, .T. ) ;
#67441 = ADVANCED_FACE ( 'NONE', ( #60435 ), #91357, .T. ) ;
#67442 = VERTEX_POINT ( 'NONE', #28960 ) ;
#67443 = VERTEX_POINT ( 'NONE', #35591 ) ;
#67444 = ADVANCED_FACE ( 'NONE', ( #6625 ), #89368, .T. ) ;
#67445 = LINE ( 'NONE', #52714, #2910 ) ;
#67446 = CARTESIAN_POINT ( 'NONE',  ( 5.543860000110784725, 20.76261553274053284, -1.500000000000002220 ) ) ;
#67447 = CARTESIAN_POINT ( 'NONE',  ( -86.62287095714999907, -23.96177878511308634, 10.65340807706329507 ) ) ;
#67448 = EDGE_LOOP ( 'NONE', ( #58998, #86652 ) ) ;
#67449 = CARTESIAN_POINT ( 'NONE',  ( -18.40674794014382698, -10.35651468716735657, 11.49999999999998934 ) ) ;
#67450 = CARTESIAN_POINT ( 'NONE',  ( -99.74569558414813741, -25.22629540225170430, 3.529807444770726388 ) ) ;
#67451 = CARTESIAN_POINT ( 'NONE',  ( -64.50991710397673273, -23.96119346886879597, -0.6495511937832134652 ) ) ;
#67452 = CARTESIAN_POINT ( 'NONE',  ( -83.54165217798484377, -24.66019654487199375, 8.947790411086122830 ) ) ;
#67453 = CARTESIAN_POINT ( 'NONE',  ( 12.99736557111424595, -6.475225279485574248, -27.13536621820933448 ) ) ;
#67454 = CARTESIAN_POINT ( 'NONE',  ( -99.41135234760463391, -25.17968299323282011, 3.254169899343974937 ) ) ;
#67455 = CARTESIAN_POINT ( 'NONE',  ( 20.41560922187292348, 8.460057656491983380, -1.500000000000002220 ) ) ;
#67456 = CARTESIAN_POINT ( 'NONE',  ( -112.6228709571500559, -29.50250786944525672, 11.44777988621622988 ) ) ;
#67457 = EDGE_CURVE ( 'NONE', #55194, #69943, #67049, .T. ) ;
#67458 = CARTESIAN_POINT ( 'NONE',  ( -51.91911984596691809, -25.24860220100267938, 5.987871812849870246 ) ) ;
#67459 = CARTESIAN_POINT ( 'NONE',  ( -59.22287095715006444, -23.47596703998600276, 11.44779298504227860 ) ) ;
#67460 = DIRECTION ( 'NONE',  ( -0.000000000000000000, -1.000000000000000000, -0.000000000000000000 ) ) ;
#67461 = VECTOR ( 'NONE', #79959, 1000.000000000000000 ) ;
#67462 = CARTESIAN_POINT ( 'NONE',  ( -5.576923076923076650, -6.376774720514418959, 20.44941907051282470 ) ) ;
#67463 = CARTESIAN_POINT ( 'NONE',  ( -16.21482014894483470, 10.69450053600103345, -1.500000000000002220 ) ) ;
#67464 = CARTESIAN_POINT ( 'NONE',  ( 11.27511198983438412, 18.17944245918264912, 11.49999999999998934 ) ) ;
#67465 = DIRECTION ( 'NONE',  ( -1.000000000000000000, 0.000000000000000000, 0.000000000000000000 ) ) ;
#67466 = CARTESIAN_POINT ( 'NONE',  ( -80.62287095715007013, -23.47596703998600631, 11.44779298504227860 ) ) ;
#67467 = CARTESIAN_POINT ( 'NONE',  ( 30.93860345374796594, 6.475225279485571583, 13.17908622612278435 ) ) ;
#67468 = CARTESIAN_POINT ( 'NONE',  ( -27.68651082257923335, -24.79949475646172630, 7.605672536963987262 ) ) ;
#67469 = CARTESIAN_POINT ( 'NONE',  ( 1.383477600506065164, -22.57338898373578218, -1.500000000000002220 ) ) ;
#67470 = VECTOR ( 'NONE', #82108, 1000.000000000000000 ) ;
#67471 = ORIENTED_EDGE ( 'NONE', *, *, #97259, .F. ) ;
#67472 = DIRECTION ( 'NONE',  ( 0.000000000000000000, -1.000000000000000000, 0.000000000000000000 ) ) ;
#67473 = FACE_OUTER_BOUND ( 'NONE', #80339, .T. ) ;
#67474 = CARTESIAN_POINT ( 'NONE',  ( -11.71124675921804403, 15.99993322257668282, 11.49999999999999645 ) ) ;
#67475 = DIRECTION ( 'NONE',  ( -0.000000000000000000, 1.000000000000000000, -0.000000000000000000 ) ) ;
#67476 = AXIS2_PLACEMENT_3D ( 'NONE', #41334, #72289, #96607 ) ;
#67477 = CARTESIAN_POINT ( 'NONE',  ( 14.76093561896379214, -6.475225279485574248, -27.37148769130089931 ) ) ;
#67478 = ORIENTED_EDGE ( 'NONE', *, *, #36328, .F. ) ;
#67479 = VECTOR ( 'NONE', #17804, 1000.000000000000114 ) ;
#67480 = CARTESIAN_POINT ( 'NONE',  ( -5.891303133519534718, -6.376774720514420736, 20.71116975788854475 ) ) ;
#67481 = CARTESIAN_POINT ( 'NONE',  ( -28.54389657640137656, -24.60093933223103235, 1.825713163565112263 ) ) ;
#67482 = CARTESIAN_POINT ( 'NONE',  ( -100.9506922656100727, -25.17353323677711785, 7.008855908370544618 ) ) ;
#67483 = CARTESIAN_POINT ( 'NONE',  ( 0.6597851148675514255, -21.60297929554585394, 11.49999999999998934 ) ) ;
#67484 = CARTESIAN_POINT ( 'NONE',  ( -49.14425558977711006, -25.27518066829780707, 3.703948608116105490 ) ) ;
#67486 = VECTOR ( 'NONE', #63903, 1000.000000000000000 ) ;
#67485 = CARTESIAN_POINT ( 'NONE',  ( 17.72857150710123619, 7.855407458714720903, -1.500000000000002220 ) ) ;
#67487 = CARTESIAN_POINT ( 'NONE',  ( 15.32643653063177958, 3.577630190450218350, -27.14485409495429380 ) ) ;
#67488 = B_SPLINE_CURVE_WITH_KNOTS ( 'NONE', 3,
 ( #11699, #79210, #33052, #56906, #11211, #18324 ),
 .UNSPECIFIED., .F., .F.,
 ( 4, 2, 4 ),
 ( 6.384118678616324667E-06, 0.001386860460828378237, 0.002767336802978140158 ),
 .UNSPECIFIED. ) ;
#67489 = CARTESIAN_POINT ( 'NONE',  ( -35.62287095715004881, -24.15431212366388536, -0.2830839119429047757 ) ) ;
#67490 = CARTESIAN_POINT ( 'NONE',  ( 9.171884637996585710, -17.55225146786146695, 11.49999999999998934 ) ) ;
#67491 = EDGE_CURVE ( 'NONE', #7626, #8365, #19837, .T. ) ;
#67492 = ORIENTED_EDGE ( 'NONE', *, *, #1100, .F. ) ;
#67493 = CARTESIAN_POINT ( 'NONE',  ( 18.17922461840205983, -9.147185827878928421, 11.49999999999999645 ) ) ;
#67494 = CARTESIAN_POINT ( 'NONE',  ( -80.64675904551151575, -25.20074414427590881, 3.409327697718777195 ) ) ;
#67495 = EDGE_CURVE ( 'NONE', #49235, #38164, #27968, .T. ) ;
#67496 = CARTESIAN_POINT ( 'NONE',  ( 33.62498039757826263, -3.398310449788993104, -11.43903334445280784 ) ) ;
#67497 = B_SPLINE_CURVE_WITH_KNOTS ( 'NONE', 3,
 ( #83284, #59463, #90406, #51854, #22366, #29993 ),
 .UNSPECIFIED., .F., .F.,
 ( 4, 2, 4 ),
 ( 0.000000000000000000, 0.001380764517854768218, 0.002761529035709536437 ),
 .UNSPECIFIED. ) ;
#67498 = ORIENTED_EDGE ( 'NONE', *, *, #31388, .F. ) ;
#67499 = CARTESIAN_POINT ( 'NONE',  ( 0.01222413314974575907, -23.20825100983049438, 6.142048374048878046 ) ) ;
#67500 = CARTESIAN_POINT ( 'NONE',  ( -111.7814946224345789, -25.29712067403330877, 4.332404411321261861 ) ) ;
#67501 = CARTESIAN_POINT ( 'NONE',  ( -64.52287095715010423, -24.66019654487200441, 8.947790411086119278 ) ) ;
#67502 = B_SPLINE_CURVE_WITH_KNOTS ( 'NONE', 3,
 ( #43668, #51782, #44673, #14196, #99435, #6597 ),
 .UNSPECIFIED., .F., .F.,
 ( 4, 2, 4 ),
 ( 0.000000000000000000, 0.001380764517854768001, 0.002761529035709536003 ),
 .UNSPECIFIED. ) ;
#67503 = CARTESIAN_POINT ( 'NONE',  ( -95.62287095715005592, -25.00158670708909625, 2.256160236439165967 ) ) ;
#67504 = LINE ( 'NONE', #36042, #41433 ) ;
#67505 = CARTESIAN_POINT ( 'NONE',  ( -20.04763853020464737, 0.9818187932333496404, 11.49999999999998934 ) ) ;
#67506 = CARTESIAN_POINT ( 'NONE',  ( -19.77875734969026311, -6.143225279485574397, 27.31649921512899937 ) ) ;
#67507 = ORIENTED_EDGE ( 'NONE', *, *, #18968, .T. ) ;
#67508 = AXIS2_PLACEMENT_3D ( 'NONE', #75385, #99705, #68289 ) ;
#67509 = CARTESIAN_POINT ( 'NONE',  ( -12.44792101662413408, -19.12764231104124946, 11.49999999999999645 ) ) ;
#67510 = CARTESIAN_POINT ( 'NONE',  ( -30.47287095715007510, -23.47593906522708451, -1.422904450652597852 ) ) ;
#67511 = CARTESIAN_POINT ( 'NONE',  ( -24.90875734969025501, 6.376774720514426953, 29.49402280011861777 ) ) ;
#67512 = CARTESIAN_POINT ( 'NONE',  ( -53.55620429048340725, -23.47593901973091235, -1.443836447539009749 ) ) ;
#67513 = CARTESIAN_POINT ( 'NONE',  ( 5.920986267150416538, -5.876774720514422512, 21.32549308339960348 ) ) ;
#67514 = ADVANCED_FACE ( 'NONE', ( #52310 ), #45198, .T. ) ;
#67515 = EDGE_CURVE ( 'NONE', #64622, #50083, #88822, .T. ) ;
#67516 = DIRECTION ( 'NONE',  ( 3.773278334444167608E-23, -1.000000000000000000, 0.000000000000000000 ) ) ;
#67517 = CARTESIAN_POINT ( 'NONE',  ( -0.1411031551986380028, 22.44022050402121948, 11.49999999999999645 ) ) ;
#67518 = CARTESIAN_POINT ( 'NONE',  ( 5.399550031317769339, 5.965225279485594001, -28.54570968858208246 ) ) ;
#67519 = EDGE_LOOP ( 'NONE', ( #70051, #99297, #96949, #53684 ) ) ;
#67520 = CARTESIAN_POINT ( 'NONE',  ( 17.42226438573850800, -10.51879874471254261, 11.49999999999998934 ) ) ;
#67521 = ORIENTED_EDGE ( 'NONE', *, *, #60163, .T. ) ;
#67522 = CARTESIAN_POINT ( 'NONE',  ( 1.269710630819723463, 22.90746787927615102, -1.500000000000002220 ) ) ;
#67523 = PLANE ( 'NONE',  #30722 ) ;
#67525 = ORIENTED_EDGE ( 'NONE', *, *, #64606, .T. ) ;
#67524 = EDGE_CURVE ( 'NONE', #36701, #24606, #74632, .T. ) ;
#67526 = LINE ( 'NONE', #36557, #687 ) ;
#67527 = EDGE_CURVE ( 'NONE', #63176, #30127, #59419, .T. ) ;
#67528 = VECTOR ( 'NONE', #46999, 1000.000000000000000 ) ;
#67529 = CARTESIAN_POINT ( 'NONE',  ( -77.64776011165024272, -23.48786465467240703, 11.44779295918254647 ) ) ;
#67530 = DIRECTION ( 'NONE',  ( -0.000000000000000000, -1.000000000000000000, 0.000000000000000000 ) ) ;
#67532 = ORIENTED_EDGE ( 'NONE', *, *, #74195, .F. ) ;
#67531 = CARTESIAN_POINT ( 'NONE',  ( -15.93125441714207646, -14.09135727244061265, 11.49999999999999645 ) ) ;
#67533 = ADVANCED_FACE ( 'NONE', ( #6123, #37075 ), #68040, .T. ) ;
#67534 = ORIENTED_EDGE ( 'NONE', *, *, #14202, .F. ) ;
#67535 = CARTESIAN_POINT ( 'NONE',  ( -21.14055147415990277, -6.693858341896442354, -1.500000000000002220 ) ) ;
#67536 = CARTESIAN_POINT ( 'NONE',  ( -13.08992234710881064, 15.94516925376868244, -1.500000000000002220 ) ) ;
#67537 = VECTOR ( 'NONE', #79195, 1000.000000000000114 ) ;
#67538 = ORIENTED_EDGE ( 'NONE', *, *, #71779, .T. ) ;
#67539 = VERTEX_POINT ( 'NONE', #45695 ) ;
#67540 = CARTESIAN_POINT ( 'NONE',  ( 6.763596848542221984, -6.376774720514426065, 21.40271460634751577 ) ) ;
#67541 = CARTESIAN_POINT ( 'NONE',  ( 2.745953332610513442, -5.876774720514418959, 21.05053573504278575 ) ) ;
#67542 = ORIENTED_EDGE ( 'NONE', *, *, #17455, .F. ) ;
#67543 = VECTOR ( 'NONE', #4155, 1000.000000000000000 ) ;
#67544 = AXIS2_PLACEMENT_3D ( 'NONE', #68804, #82033, #14001 ) ;
#67545 = EDGE_LOOP ( 'NONE', ( #65900, #73180, #85481, #53835 ) ) ;
#67546 = CARTESIAN_POINT ( 'NONE',  ( -49.52287095715007581, -24.33927499327855060, 9.819080762295818943 ) ) ;
#67547 = CARTESIAN_POINT ( 'NONE',  ( -111.5146074832896943, -24.51419770103157703, 9.386484678747162747 ) ) ;
#67548 = CARTESIAN_POINT ( 'NONE',  ( -94.52287095715006160, -24.64965694238575011, 8.947790433994196491 ) ) ;
#67549 = CARTESIAN_POINT ( 'NONE',  ( -5.109682455881146446, -20.12422286529520932, -1.500000000000002220 ) ) ;
#67550 = EDGE_CURVE ( 'NONE', #30854, #47768, #76618, .T. ) ;
#67551 = CARTESIAN_POINT ( 'NONE',  ( 10.83000837110471082, 18.85367679709202804, 11.49999999999999645 ) ) ;
#67552 = EDGE_LOOP ( 'NONE', ( #83486, #11232, #21560, #21383 ) ) ;
#67553 = CARTESIAN_POINT ( 'NONE',  ( -39.44687923781921057, -25.27828342519987359, 4.188173683033348027 ) ) ;
#67554 = CARTESIAN_POINT ( 'NONE',  ( -0.02075734969026423599, 5.866774720514426278, -0.08597719988137648983 ) ) ;
#67555 = CARTESIAN_POINT ( 'NONE',  ( -115.5155081638650643, -24.63355581998386157, 0.9682620441943915468 ) ) ;
#67556 = CARTESIAN_POINT ( 'NONE',  ( 18.78116726530667080, 12.29669497462397842, 11.49999999999998934 ) ) ;
#67557 = AXIS2_PLACEMENT_3D ( 'NONE', #72873, #35310, #50041 ) ;
#67558 = CARTESIAN_POINT ( 'NONE',  ( 6.403846153846157740, -6.376774720514426065, 21.48076923076922995 ) ) ;
#67559 = ORIENTED_EDGE ( 'NONE', *, *, #19602, .F. ) ;
#67560 = CARTESIAN_POINT ( 'NONE',  ( -87.52287095715006160, -23.48783264083352762, -1.443836473376473695 ) ) ;
#67561 = DIRECTION ( 'NONE',  ( -3.773278334444166432E-23, 1.000000000000000000, 0.000000000000000000 ) ) ;
#67562 = ORIENTED_EDGE ( 'NONE', *, *, #33869, .F. ) ;
#67563 = ORIENTED_EDGE ( 'NONE', *, *, #38780, .T. ) ;
#67565 = ADVANCED_FACE ( 'NONE', ( #85243 ), #11756, .T. ) ;
#67564 = CARTESIAN_POINT ( 'NONE',  ( -10.54059822343757880, -6.376774720514426953, 23.12308057603841149 ) ) ;
#67566 = ORIENTED_EDGE ( 'NONE', *, *, #42111, .T. ) ;
#67567 = CARTESIAN_POINT ( 'NONE',  ( -20.48789480994130230, 5.740754632170482097, -1.500000000000002220 ) ) ;
#67568 = ADVANCED_FACE ( 'NONE', ( #69533 ), #24352, .F. ) ;
#67569 = ORIENTED_EDGE ( 'NONE', *, *, #12545, .T. ) ;
#67570 = DIRECTION ( 'NONE',  ( -1.000000000000000000, -0.000000000000000000, -0.000000000000000000 ) ) ;
#67571 = CARTESIAN_POINT ( 'NONE',  ( -18.19455084753484542, -10.52586660885228298, 11.49999999999998934 ) ) ;
#67572 = PLANE ( 'NONE',  #48143 ) ;
#67573 = CARTESIAN_POINT ( 'NONE',  ( 22.61316900856233403, 2.020702135111208442, -1.500000000000002220 ) ) ;
#67574 = CARTESIAN_POINT ( 'NONE',  ( 14.61581677259038692, -3.466180823938291855, -27.35847992067005308 ) ) ;
#67575 = CARTESIAN_POINT ( 'NONE',  ( -29.52287095715006160, -23.38909342368989641, 11.44779306042727285 ) ) ;
#67576 = CARTESIAN_POINT ( 'NONE',  ( 21.48171311866277122, -4.276277801222842179, -1.500000000000002220 ) ) ;
#67577 = CARTESIAN_POINT ( 'NONE',  ( -87.54532251907512830, -24.51314013834317507, 0.6176544820404262781 ) ) ;
#67578 = ORIENTED_EDGE ( 'NONE', *, *, #59922, .F. ) ;
#67579 = CARTESIAN_POINT ( 'NONE',  ( -122.6234929911659606, -24.66019654487200086, 8.947790411086113949 ) ) ;
#67580 = EDGE_CURVE ( 'NONE', #3446, #1307, #59712, .T. ) ;
#67581 = AXIS2_PLACEMENT_3D ( 'NONE', #35489, #89769, #29740 ) ;
#67582 = ADVANCED_FACE ( 'NONE', ( #62937 ), #80605, .T. ) ;
#67583 = EDGE_LOOP ( 'NONE', ( #28058, #98139, #54520, #51989 ) ) ;
#67584 = CARTESIAN_POINT ( 'NONE',  ( -84.55846707206313795, -23.73791477778912551, 11.05961554403170766 ) ) ;
#67585 = CARTESIAN_POINT ( 'NONE',  ( -29.49875734969026198, 0.3587747205144265483, 2.362022800118626531 ) ) ;
#67586 = CIRCLE ( 'NONE', #62742, 0.1000000000000000472 ) ;
#67587 = CARTESIAN_POINT ( 'NONE',  ( -30.60199688435473320, -24.75181118439798311, 1.363349870542264863 ) ) ;
#67588 = CARTESIAN_POINT ( 'NONE',  ( 9.380127297304197143, -19.07726845333505494, -1.500000000000002220 ) ) ;
#67589 = CARTESIAN_POINT ( 'NONE',  ( -112.5870109292292511, -24.65952944569305316, 1.056160979905707897 ) ) ;
#67590 = CARTESIAN_POINT ( 'NONE',  ( -26.80230302508262241, -24.97064477538173222, 2.622372507731231650 ) ) ;
#67591 = CARTESIAN_POINT ( 'NONE',  ( -85.63197954799407796, -24.52300882791530157, 0.6510814631126254914 ) ) ;
#67592 = CARTESIAN_POINT ( 'NONE',  ( -29.55620429048340725, -23.40356933438083331, -1.443836155048349834 ) ) ;
#67593 = B_SPLINE_SURFACE_WITH_KNOTS ( 'NONE', 3, 3, ( 
 ( #63795, #17085, #94711, #34322 ),
 ( #40437, #25194, #79489, #64801 ),
 ( #26205, #56171, #49556, #9976 ),
 ( #2376, #57178, #80485, #33307 ),
 ( #10981, #64295, #72889, #41946 ),
 ( #95218, #65299, #96224, #57666 ),
 ( #88609, #78474, #8974, #67785 ) ),
 .UNSPECIFIED., .F., .F., .F.,
 ( 4, 3, 4 ),
 ( 4, 4 ),
 ( 0.7945040050992246972, 0.8970133687736505657, 0.9995227324480764342 ),
 ( 0.4796158742846823864, 0.4808500213541327395 ),
 .UNSPECIFIED. ) ;
#67594 = LINE ( 'NONE', #97525, #18295 ) ;
#67595 = ORIENTED_EDGE ( 'NONE', *, *, #42113, .F. ) ;
#67596 = CARTESIAN_POINT ( 'NONE',  ( -99.96028742912865539, -25.05658428359392076, 7.499825484813623433 ) ) ;
#67597 = CARTESIAN_POINT ( 'NONE',  ( 19.42422255247381457, -2.945173967302487039, 11.49999999999999645 ) ) ;
#67598 = PLANE ( 'NONE',  #73033 ) ;
#67599 = DIRECTION ( 'NONE',  ( -1.000000000000000000, 0.000000000000000000, -0.000000000000000000 ) ) ;
#67600 = VERTEX_POINT ( 'NONE', #17743 ) ;
#67601 = CARTESIAN_POINT ( 'NONE',  ( -69.10880722458374237, -25.29515380318773765, 5.511221748791859554 ) ) ;
#67602 = CARTESIAN_POINT ( 'NONE',  ( -99.60228783053516111, -25.31549506111867487, 4.950078004910987595 ) ) ;
#67603 = VECTOR ( 'NONE', #21631, 1000.000000000000114 ) ;
#67604 = CARTESIAN_POINT ( 'NONE',  ( -25.57898076830435485, -24.90004706754400488, 5.867565877950162267 ) ) ;
#67605 = FACE_OUTER_BOUND ( 'NONE', #1918, .T. ) ;
#67606 = ADVANCED_FACE ( 'NONE', ( #86749 ), #72540, .F. ) ;
#67607 = CARTESIAN_POINT ( 'NONE',  ( 10.64064036176630879, -16.58286410872727146, 11.49999999999998934 ) ) ;
#67608 = ORIENTED_EDGE ( 'NONE', *, *, #17923, .F. ) ;
#67609 = CARTESIAN_POINT ( 'NONE',  ( 33.61456970919605425, -3.316774720514426900, -11.35828564741663449 ) ) ;
#67610 = CARTESIAN_POINT ( 'NONE',  ( -70.62287095715009855, -24.63287334234179937, 0.9662140553045409641 ) ) ;
#67611 = EDGE_CURVE ( 'NONE', #87143, #94978, #25852, .T. ) ;
#67612 = DATE_AND_TIME ( #19424, #47303 ) ;
#67613 = ORIENTED_EDGE ( 'NONE', *, *, #84721, .F. ) ;
#67614 = CARTESIAN_POINT ( 'NONE',  ( 8.071512145086501278, -1.000000000000000000, 3.746884140868835367 ) ) ;
#67615 = CARTESIAN_POINT ( 'NONE',  ( -103.6228709571500559, -24.51387760970723662, 9.387446482453412955 ) ) ;
#67616 = CARTESIAN_POINT ( 'NONE',  ( -55.55112771745390177, -24.15503026093912808, -0.2815557561904589168 ) ) ;
#67617 = DIRECTION ( 'NONE',  ( -0.9980236263794188822, 0.000000000000000000, 0.06283980576413539243 ) ) ;
#67618 = LINE ( 'NONE', #89942, #67783 ) ;
#67619 = AXIS2_PLACEMENT_3D ( 'NONE', #19751, #58349, #21250 ) ;
#67620 = PLANE ( 'NONE',  #34397 ) ;
#67621 = CARTESIAN_POINT ( 'NONE',  ( -107.5572310108091187, -23.73766607897672642, -1.055555164236427590 ) ) ;
#67622 = CARTESIAN_POINT ( 'NONE',  ( -4.560224734120114753, 19.45435480350565882, -1.500000000000002220 ) ) ;
#67623 = DIRECTION ( 'NONE',  ( -3.773278334453079618E-23, 0.9999999999976377785, 2.173523156925979975E-06 ) ) ;
#67624 = CARTESIAN_POINT ( 'NONE',  ( -0.01293961071214225038, -22.88248657085181748, 2.995806029868834486 ) ) ;
#67625 = VERTEX_POINT ( 'NONE', #40590 ) ;
#67626 = CARTESIAN_POINT ( 'NONE',  ( -20.27875734969026311, 3.456774720514426136, 22.85402280011862430 ) ) ;
#67627 = DIRECTION ( 'NONE',  ( 2.615445361545220718E-15, -6.974520964120588319E-15, 1.000000000000000000 ) ) ;
#67628 = CARTESIAN_POINT ( 'NONE',  ( -119.5902202967278072, -24.15543982623907837, -0.2315651400026546569 ) ) ;
#67629 = LINE ( 'NONE', #12816, #70233 ) ;
#67630 = DIRECTION ( 'NONE',  ( -3.773278334444166432E-23, 1.000000000000000000, 0.000000000000000000 ) ) ;
#67631 = CARTESIAN_POINT ( 'NONE',  ( -39.51316539375884673, -23.73766607897669800, -1.055555164236461341 ) ) ;
#67632 = CARTESIAN_POINT ( 'NONE',  ( -119.6228709571501128, -24.50216790748207529, 0.6166512839542543922 ) ) ;
#67633 = CARTESIAN_POINT ( 'NONE',  ( -1.456683411003494966, -5.876774720514415407, 19.95737465391042775 ) ) ;
#67634 = B_SPLINE_CURVE_WITH_KNOTS ( 'NONE', 3,
 ( #97356, #80631, #81634, #4518 ),
 .UNSPECIFIED., .F., .F.,
 ( 4, 4 ),
 ( 0.000000000000000000, 9.999999999999592548E-05 ),
 .UNSPECIFIED. ) ;
#67636 = EDGE_CURVE ( 'NONE', #55933, #12105, #98095, .T. ) ;
#67635 = ORIENTED_EDGE ( 'NONE', *, *, #65957, .F. ) ;
#67637 = CARTESIAN_POINT ( 'NONE',  ( -5.366453405989236813, 0.000000000000000000, 18.50000000000000000 ) ) ;
#67638 = CARTESIAN_POINT ( 'NONE',  ( -100.6228709571500559, -29.50249982740957577, 7.747779886224967605 ) ) ;
#67639 = ORIENTED_EDGE ( 'NONE', *, *, #47363, .F. ) ;
#67640 = CARTESIAN_POINT ( 'NONE',  ( -11.05657426389776354, 17.00066307926000420, -1.500000000000002220 ) ) ;
#67641 = CARTESIAN_POINT ( 'NONE',  ( -122.6263427379263220, -23.73766607897671221, -1.055555164236450461 ) ) ;
#67642 = CARTESIAN_POINT ( 'NONE',  ( 9.478389368232452483, 2.682774720514426559, -23.17485683983816003 ) ) ;
#67643 = ADVANCED_FACE ( 'NONE', ( #25351 ), #75811, .T. ) ;
#67644 = VECTOR ( 'NONE', #87781, 1000.000000000000000 ) ;
#67645 = ADVANCED_FACE ( 'NONE', ( #33968 ), #94860, .F. ) ;
#67646 = DIRECTION ( 'NONE',  ( -1.000000000000000000, -0.000000000000000000, -0.000000000000000000 ) ) ;
#67647 = EDGE_CURVE ( 'NONE', #5613, #26949, #54850, .T. ) ;
#67648 = ORIENTED_EDGE ( 'NONE', *, *, #9904, .F. ) ;
#67649 = PLANE ( 'NONE',  #72879 ) ;
#67650 = CARTESIAN_POINT ( 'NONE',  ( -46.52287095715004028, -23.95044443724990657, 10.65354141964648882 ) ) ;
#67651 = CARTESIAN_POINT ( 'NONE',  ( 19.36564117097816862, 5.170944958934900804, -1.500000000000002220 ) ) ;
#67652 = CARTESIAN_POINT ( 'NONE',  ( 14.88031740681034698, -14.96734982212533183, 11.49999999999999645 ) ) ;
#67653 = ADVANCED_FACE ( 'NONE', ( #28932 ), #80343, .F. ) ;
#67654 = VECTOR ( 'NONE', #57869, 1000.000000000000000 ) ;
#67655 = CARTESIAN_POINT ( 'NONE',  ( 30.55456828421202076, 1.252966014080275192, 24.28055799599968623 ) ) ;
#67656 = CARTESIAN_POINT ( 'NONE',  ( -70.49055710964816512, -24.83644354573578283, 8.397322867130098345 ) ) ;
#67657 = CARTESIAN_POINT ( 'NONE',  ( -12.21066354923914865, 18.40238043084326591, -1.500000000000002220 ) ) ;
#67658 = CARTESIAN_POINT ( 'NONE',  ( -18.81443736134900035, 8.205417114561466718, 11.49999999999998934 ) ) ;
#67659 = CARTESIAN_POINT ( 'NONE',  ( -93.55620429048339304, -23.47596703998600631, 11.44779298504227683 ) ) ;
#67660 = DIRECTION ( 'NONE',  ( 0.000000000000000000, 0.000000000000000000, 1.000000000000000000 ) ) ;
#67661 = DIRECTION ( 'NONE',  ( 0.000000000000000000, -1.000000000000000000, 0.000000000000000000 ) ) ;
#67662 = ORIENTED_EDGE ( 'NONE', *, *, #37901, .F. ) ;
#67663 = CARTESIAN_POINT ( 'NONE',  ( 25.61870917940689196, -0.3587747205144265483, 29.49402280011862487 ) ) ;
#67664 = FACE_OUTER_BOUND ( 'NONE', #80480, .T. ) ;
#67665 = ORIENTED_EDGE ( 'NONE', *, *, #62029, .T. ) ;
#67666 = ORIENTED_EDGE ( 'NONE', *, *, #20775, .F. ) ;
#67667 = FACE_OUTER_BOUND ( 'NONE', #41172, .T. ) ;
#67668 = CARTESIAN_POINT ( 'NONE',  ( -61.47555956910319708, -25.05987955553484525, 7.435194464380680657 ) ) ;
#67669 = CARTESIAN_POINT ( 'NONE',  ( -76.62668118872166190, -24.51314013834316441, 0.6176544820404190617 ) ) ;
#67670 = CARTESIAN_POINT ( 'NONE',  ( -9.016818060619870678, -18.48156098877705844, -1.500000000000002220 ) ) ;
#67671 = EDGE_CURVE ( 'NONE', #54031, #75907, #10839, .T. ) ;
#67672 = EDGE_CURVE ( 'NONE', #36632, #21243, #39791, .T. ) ;
#67673 = CARTESIAN_POINT ( 'NONE',  ( 21.29926025483437257, -3.289820829717503337, 11.49999999999999645 ) ) ;
#67674 = ORIENTED_EDGE ( 'NONE', *, *, #87711, .T. ) ;
#67675 = CARTESIAN_POINT ( 'NONE',  ( -99.30689605304669954, -25.29963387158551669, 4.613820302888914426 ) ) ;
#67676 = CARTESIAN_POINT ( 'NONE',  ( -129.6228709571500133, -24.34917612406838572, 0.1852690917426697004 ) ) ;
#67677 = CARTESIAN_POINT ( 'NONE',  ( -10.28394192611005842, 19.82837715243953625, 11.49999999999998934 ) ) ;
#67678 = AXIS2_PLACEMENT_3D ( 'NONE', #50490, #37626, #68583 ) ;
#67679 = DIRECTION ( 'NONE',  ( 0.000000000000000000, 0.000000000000000000, 1.000000000000000000 ) ) ;
#67680 = CARTESIAN_POINT ( 'NONE',  ( -84.64453684150217327, -23.48783264082476308, -1.443836473390094799 ) ) ;
#67681 = EDGE_CURVE ( 'NONE', #35091, #85611, #77813, .T. ) ;
#67682 = VERTEX_POINT ( 'NONE', #37045 ) ;
#67683 = CARTESIAN_POINT ( 'NONE',  ( -43.62287095715004881, -23.47593901973091235, -1.443836447539011525 ) ) ;
#67684 = CARTESIAN_POINT ( 'NONE',  ( -35.51857469582687088, -25.00182538069146077, 7.747789668545035369 ) ) ;
#67685 = CARTESIAN_POINT ( 'NONE',  ( 20.66465755290784401, -3.126920214821775623, -1.500000000000002220 ) ) ;
#67686 = ORIENTED_EDGE ( 'NONE', *, *, #34311, .F. ) ;
#67689 = ORIENTED_EDGE ( 'NONE', *, *, #19991, .F. ) ;
#67688 = EDGE_CURVE ( 'NONE', #97596, #3302, #52277, .T. ) ;
#67687 = CARTESIAN_POINT ( 'NONE',  ( -86.63552353197610501, -23.96119346886881019, -0.6495511937831902616 ) ) ;
#67690 = AXIS2_PLACEMENT_3D ( 'NONE', #51923, #91459, #99067 ) ;
#67691 = VERTEX_POINT ( 'NONE', #58027 ) ;
#67692 = CARTESIAN_POINT ( 'NONE',  ( -50.90512332773992199, -25.29912375439049654, 4.600680353948681578 ) ) ;
#67693 = CARTESIAN_POINT ( 'NONE',  ( -2.902382693073098707, -20.91247731031871382, -1.500000000000002220 ) ) ;
#67694 = ORIENTED_EDGE ( 'NONE', *, *, #93664, .T. ) ;
#67695 = LINE ( 'NONE', #21479, #39725 ) ;
#67696 = CARTESIAN_POINT ( 'NONE',  ( 31.88667425545053291, -2.682774720514426559, -9.651215965565024035 ) ) ;
#67697 = CARTESIAN_POINT ( 'NONE',  ( -100.6228709571500559, -29.50247984919015209, -1.443849546365050029 ) ) ;
#67698 = AXIS2_PLACEMENT_3D ( 'NONE', #57488, #42273, #88424 ) ;
#67699 = CARTESIAN_POINT ( 'NONE',  ( -76.62361889982840069, -24.66019654487199375, 8.947790411086119278 ) ) ;
#67700 = B_SPLINE_CURVE_WITH_KNOTS ( 'NONE', 3,
 ( #78753, #63067, #70665, #40216 ),
 .UNSPECIFIED., .F., .F.,
 ( 4, 4 ),
 ( 0.000000000000000000, 9.999999999999592548E-05 ),
 .UNSPECIFIED. ) ;
#67701 = CARTESIAN_POINT ( 'NONE',  ( -80.48900664166535535, -25.13313949306887807, 7.101635536975466678 ) ) ;
#67702 = CARTESIAN_POINT ( 'NONE',  ( -14.02725853290852243, 16.66567569088042688, -1.500000000000002220 ) ) ;
#67703 = CARTESIAN_POINT ( 'NONE',  ( -71.22803624472236095, -25.24674067209845418, 4.920688748475479102 ) ) ;
#67705 = VERTEX_POINT ( 'NONE', #64655 ) ;
#67704 = CARTESIAN_POINT ( 'NONE',  ( -6.278373996654322831, -21.41630973362384083, 11.49999999999999645 ) ) ;
#67706 = CARTESIAN_POINT ( 'NONE',  ( -60.62287095715004881, -25.00182538069145011, 7.747789668545098429 ) ) ;
#67707 = CARTESIAN_POINT ( 'NONE',  ( 14.64534568429317218, 3.754078354150065522, -27.31564152833324499 ) ) ;
#67708 = CARTESIAN_POINT ( 'NONE',  ( 1.305682803664691249, -5.965225279485572685, 29.57950906855421991 ) ) ;
#67710 = ORIENTED_EDGE ( 'NONE', *, *, #8433, .T. ) ;
#67709 = EDGE_CURVE ( 'NONE', #78496, #54952, #18445, .T. ) ;
#67711 = EDGE_CURVE ( 'NONE', #74791, #27009, #48923, .T. ) ;
#67712 = ORIENTED_EDGE ( 'NONE', *, *, #3051, .T. ) ;
#67713 = ADVANCED_FACE ( 'NONE', ( #96074 ), #42801, .T. ) ;
#67714 = VERTEX_POINT ( 'NONE', #33676 ) ;
#67715 = CARTESIAN_POINT ( 'NONE',  ( -101.0859251941938055, -25.16066481202448557, 6.938184544222248284 ) ) ;
#67716 = CARTESIAN_POINT ( 'NONE',  ( -78.62287095715005592, -29.50248528299804818, 1.056150453629038477 ) ) ;
#67717 = CARTESIAN_POINT ( 'NONE',  ( 30.59918777245023236, -5.333550415411136392, 26.68477081578061316 ) ) ;
#67718 = CARTESIAN_POINT ( 'NONE',  ( 29.64064043116815128, 6.475225279485573360, 28.71191112024341408 ) ) ;
#67719 = CARTESIAN_POINT ( 'NONE',  ( -8.550378450311910683, 17.38971893761031851, -1.500000000000002220 ) ) ;
#67720 = DIRECTION ( 'NONE',  ( -1.000000000000000000, 0.000000000000000000, -0.000000000000000000 ) ) ;
#67721 = ORIENTED_EDGE ( 'NONE', *, *, #16659, .F. ) ;
#67722 = CARTESIAN_POINT ( 'NONE',  ( 2.844571010020486845, -19.19604305453586690, 11.49999999999999645 ) ) ;
#67723 = LINE ( 'NONE', #35269, #92486 ) ;
#67724 = B_SPLINE_CURVE_WITH_KNOTS ( 'NONE', 3,
 ( #22308, #97934, #53286, #29429 ),
 .UNSPECIFIED., .F., .F.,
 ( 4, 4 ),
 ( 0.000000000000000000, 1.000000000000000000 ),
 .UNSPECIFIED. ) ;
#67725 = EDGE_LOOP ( 'NONE', ( #69813, #89370, #88356, #77989 ) ) ;
#67726 = CARTESIAN_POINT ( 'NONE',  ( 3.787259615384621636, -6.376774720514404748, 18.51923076923076650 ) ) ;
#67727 = FACE_OUTER_BOUND ( 'NONE', #25804, .T. ) ;
#67728 = AXIS2_PLACEMENT_3D ( 'NONE', #33365, #25760, #42005 ) ;
#67729 = CARTESIAN_POINT ( 'NONE',  ( -102.6228709571500275, -23.48783264082478794, -1.443836473390062158 ) ) ;
#67730 = DIRECTION ( 'NONE',  ( -3.773278334453079618E-23, 0.9999999999976377785, 2.173523156925979975E-06 ) ) ;
#67731 = CARTESIAN_POINT ( 'NONE',  ( 16.02095076306289201, 11.36058263404076030, -1.500000000000002220 ) ) ;
#67732 = B_SPLINE_SURFACE_WITH_KNOTS ( 'NONE', 3, 1, ( 
 ( #48922, #87471 ),
 ( #2748, #11838 ),
 ( #3749, #95084 ),
 ( #25569, #72762 ),
 ( #95581, #56540 ),
 ( #10346, #72259 ),
 ( #80357, #49933 ),
 ( #73742, #26070 ),
 ( #11349, #42323 ),
 ( #17961, #57542 ),
 ( #18953, #34690 ),
 ( #58041, #50416 ),
 ( #32679, #94580 ),
 ( #25061, #59526 ),
 ( #66163, #60032 ) ),
 .UNSPECIFIED., .F., .F., .F.,
 ( 4, 1, 1, 1, 1, 1, 1, 1, 1, 1, 1, 1, 4 ),
 ( 2, 2 ),
 ( 0.000000000000000000, 0.08436071833182734458, 0.1674897660598589910, 0.2505333068873835112, 0.3353998789434969874, 0.4196274113919481463, 0.5021719904600034923, 0.5840851136372724461, 0.6672595181981534340, 0.7504339227590341999, 0.8329476815839259585, 0.9156652780073727405, 1.000000000000000000 ),
 ( 0.000000000000000000, 1.000000000000000000 ),
 .UNSPECIFIED. ) ;
#67733 = CARTESIAN_POINT ( 'NONE',  ( -46.49383670590691509, -24.34968618360933235, 0.1864209137778778391 ) ) ;
#67734 = VERTEX_POINT ( 'NONE', #81348 ) ;
#67735 = CARTESIAN_POINT ( 'NONE',  ( 20.98369277809155165, -4.918611649023987731, 11.49999999999998934 ) ) ;
#67736 = DIRECTION ( 'NONE',  ( 1.000000000000000000, 0.000000000000000000, 0.000000000000000000 ) ) ;
#67737 = CARTESIAN_POINT ( 'NONE',  ( -70.32380231474228083, -25.25639601488366637, 7.101635269074562551 ) ) ;
#67738 = FACE_OUTER_BOUND ( 'NONE', #85751, .T. ) ;
#67739 = CARTESIAN_POINT ( 'NONE',  ( -32.30247028140506416, 5.965225279485572685, 27.60502002861223048 ) ) ;
#67740 = CARTESIAN_POINT ( 'NONE',  ( 20.35648204094723468, -10.72454223111430593, -1.500000000000002220 ) ) ;
#67741 = COORDINATED_UNIVERSAL_TIME_OFFSET ( 0, 0, .AHEAD. ) ;
#67742 = CARTESIAN_POINT ( 'NONE',  ( -101.5084176993576648, -25.27307239909413639, 3.986250617436080113 ) ) ;
#67743 = CARTESIAN_POINT ( 'NONE',  ( -83.62287095715005592, -29.50248528299804818, 1.056150453629038477 ) ) ;
#67744 = CARTESIAN_POINT ( 'NONE',  ( 4.949566031639514918, 19.51814346981619863, 11.49999999999999645 ) ) ;
#67745 = CARTESIAN_POINT ( 'NONE',  ( -109.2412217894342916, -25.28814177081538972, 3.330160904322529536 ) ) ;
#67746 = FACE_OUTER_BOUND ( 'NONE', #57939, .T. ) ;
#67747 = CARTESIAN_POINT ( 'NONE',  ( -4.165021623707020559, -5.876774720514418071, 20.26087634804756377 ) ) ;
#67748 = FACE_OUTER_BOUND ( 'NONE', #44193, .T. ) ;
#67749 = CARTESIAN_POINT ( 'NONE',  ( -122.5228709571500616, -24.66019654487200441, 8.947790411086112172 ) ) ;
#67750 = CARTESIAN_POINT ( 'NONE',  ( -6.239078800006583769, 18.87631364486404806, 11.49999999999998934 ) ) ;
#67751 = DIRECTION ( 'NONE',  ( -3.773278334453079618E-23, 0.9999999999976377785, 2.173523156925979975E-06 ) ) ;
#67752 = CARTESIAN_POINT ( 'NONE',  ( -6.431973572030615038, 18.70533856667250916, -1.500000000000002220 ) ) ;
#67753 = VECTOR ( 'NONE', #34784, 1000.000000000000000 ) ;
#67754 = DIRECTION ( 'NONE',  ( -0.000000000000000000, -1.000000000000000000, -0.000000000000000000 ) ) ;
#67755 = CARTESIAN_POINT ( 'NONE',  ( -73.22287095715006444, -23.47596703998600631, 11.44779298504227860 ) ) ;
#67756 = CARTESIAN_POINT ( 'NONE',  ( -37.52287095715008292, -24.51283580621450398, 0.6167428607045408739 ) ) ;
#67757 = CARTESIAN_POINT ( 'NONE',  ( 15.34805171112899203, -13.82090413600154299, 11.49999999999999645 ) ) ;
#67758 = CARTESIAN_POINT ( 'NONE',  ( -56.55620429048339304, -23.47593901973091235, -1.443836447539007972 ) ) ;
#67759 = CIRCLE ( 'NONE', #82300, 2.500000000000465405 ) ;
#67760 = PLANE ( 'NONE',  #61026 ) ;
#67761 = CARTESIAN_POINT ( 'NONE',  ( -50.05581273115511465, -25.25138681102044913, 5.236521854102218043 ) ) ;
#67762 = CARTESIAN_POINT ( 'NONE',  ( -20.99730734726578874, -8.693733401623333634, 11.49999999999999645 ) ) ;
#67763 = ORIENTED_EDGE ( 'NONE', *, *, #51407, .F. ) ;
#67764 = CARTESIAN_POINT ( 'NONE',  ( -46.62287095715006302, -24.51387760970722240, 9.387446482453421837 ) ) ;
#67766 = EDGE_CURVE ( 'NONE', #23547, #54552, #49919, .T. ) ;
#67765 = CARTESIAN_POINT ( 'NONE',  ( 30.61317826727886526, 3.861502214243257125, 27.24847364799711613 ) ) ;
#67767 = AXIS2_PLACEMENT_3D ( 'NONE', #23406, #53393, #76695 ) ;
#67768 = EDGE_CURVE ( 'NONE', #81257, #50685, #24632, .T. ) ;
#67769 = CARTESIAN_POINT ( 'NONE',  ( -9.895454706725905325, 17.58729670687104729, -1.500000000000002220 ) ) ;
#67770 = B_SPLINE_CURVE_WITH_KNOTS ( 'NONE', 3,
 ( #22879, #44754, #6676, #75678, #45253, #38122 ),
 .UNSPECIFIED., .F., .F.,
 ( 4, 2, 4 ),
 ( 6.384118695308377748E-06, 0.001386860460836723775, 0.002767336802978138856 ),
 .UNSPECIFIED. ) ;
#67771 = CARTESIAN_POINT ( 'NONE',  ( -63.65416434033561899, -23.48783264082475952, -1.443836473390093245 ) ) ;
#67772 = EDGE_CURVE ( 'NONE', #56501, #55445, #3736, .T. ) ;
#67773 = DIRECTION ( 'NONE',  ( 1.000000000000000000, 3.773278334444167608E-23, 8.201307833595939069E-29 ) ) ;
#67774 = B_SPLINE_CURVE_WITH_KNOTS ( 'NONE', 3,
 ( #15713, #76103, #22808, #30939 ),
 .UNSPECIFIED., .F., .F.,
 ( 4, 4 ),
 ( 0.8093576887341661363, 0.8103584357749318290 ),
 .UNSPECIFIED. ) ;
#67775 = EDGE_CURVE ( 'NONE', #37481, #69074, #4226, .T. ) ;
#67776 = VERTEX_POINT ( 'NONE', #21306 ) ;
#67777 = EDGE_CURVE ( 'NONE', #65243, #55675, #6500, .T. ) ;
#67778 = ORIENTED_EDGE ( 'NONE', *, *, #26779, .T. ) ;
#67779 = CARTESIAN_POINT ( 'NONE',  ( -0.4362980769230789257, -5.876774720514411854, 19.46153846153846345 ) ) ;
#67780 = CARTESIAN_POINT ( 'NONE',  ( 9.198035947750891950, -20.93187084735588144, 11.49999999999998934 ) ) ;
#67781 = CARTESIAN_POINT ( 'NONE',  ( -29.67002368223832676, -23.41236132725490293, -1.443836171194816886 ) ) ;
#67782 = CARTESIAN_POINT ( 'NONE',  ( 17.73057777116804701, 12.32922261165129285, -1.500000000000002220 ) ) ;
#67783 = VECTOR ( 'NONE', #68113, 1000.000000000000000 ) ;
#67784 = PLANE ( 'NONE',  #56106 ) ;
#67785 = CARTESIAN_POINT ( 'NONE',  ( -82.52213977090120522, -23.48786465467241413, 11.44779295918254824 ) ) ;
#67786 = CARTESIAN_POINT ( 'NONE',  ( -16.74547196562220464, 15.07928529822544661, 11.49999999999999645 ) ) ;
#67787 = ORIENTED_EDGE ( 'NONE', *, *, #72263, .T. ) ;
#67788 = DIRECTION ( 'NONE',  ( 0.9685340172660600322, 0.000000000000000000, -0.2488812114211667315 ) ) ;
#67789 = CARTESIAN_POINT ( 'NONE',  ( -1.351711525931510449, 21.94731587555429186, -1.500000000000002220 ) ) ;
#67790 = DIRECTION ( 'NONE',  ( -3.773278334453079030E-23, 0.9999999999976377785, 2.173523156925979128E-06 ) ) ;
#67791 = FACE_OUTER_BOUND ( 'NONE', #6858, .T. ) ;
#67792 = ORIENTED_EDGE ( 'NONE', *, *, #70192, .T. ) ;
#67793 = CARTESIAN_POINT ( 'NONE',  ( 4.642799911345256270, -6.376774720514408301, 18.59646607068888713 ) ) ;
#67794 = CARTESIAN_POINT ( 'NONE',  ( -90.63673542715442011, -24.15602025860896873, 10.28564288303535434 ) ) ;
#67795 = ORIENTED_EDGE ( 'NONE', *, *, #11867, .F. ) ;
#67796 = CARTESIAN_POINT ( 'NONE',  ( -29.52287095715007581, -24.57618165405973087, 1.056161296257514870 ) ) ;
#67797 = ORIENTED_EDGE ( 'NONE', *, *, #21671, .F. ) ;
#67798 = VERTEX_POINT ( 'NONE', #68006 ) ;
#67799 = FACE_OUTER_BOUND ( 'NONE', #20077, .T. ) ;
#67800 = DIRECTION ( 'NONE',  ( -3.773278334444166432E-23, 1.000000000000000000, 0.000000000000000000 ) ) ;
#67801 = CARTESIAN_POINT ( 'NONE',  ( -57.52207148937385739, -23.48783264082477018, -1.443836473390095243 ) ) ;
#67802 = CARTESIAN_POINT ( 'NONE',  ( -10.01004151551622456, -17.79114453763541093, -1.500000000000002220 ) ) ;
#67803 = EDGE_CURVE ( 'NONE', #21715, #46174, #29424, .T. ) ;
#67804 = VERTEX_POINT ( 'NONE', #10334 ) ;
#67805 = CARTESIAN_POINT ( 'NONE',  ( -0.4686347352592966087, -5.876774720514411854, 19.46274624311237034 ) ) ;
#67806 = CARTESIAN_POINT ( 'NONE',  ( -99.52287095715001897, -24.35013146730204525, 9.818937971375097717 ) ) ;
#67807 = DIRECTION ( 'NONE',  ( 0.1875268396392986980, 0.000000000000000000, 0.9822594791677485837 ) ) ;
#67808 = CARTESIAN_POINT ( 'NONE',  ( 29.77147767949874790, 5.356774720514425603, 26.15915692125051706 ) ) ;
#67809 = EDGE_CURVE ( 'NONE', #37373, #70639, #56114, .T. ) ;
#67810 = EDGE_LOOP ( 'NONE', ( #5997, #76029, #50987, #46411 ) ) ;
#67811 = CARTESIAN_POINT ( 'NONE',  ( -51.52287095715006870, -29.50250243563736774, 8.947779886222146928 ) ) ;
#67812 = CARTESIAN_POINT ( 'NONE',  ( -27.75512851621423138, -25.26248076641628515, 8.250985936982687008 ) ) ;
#67813 = CARTESIAN_POINT ( 'NONE',  ( 18.03836333725549324, -10.36167025447706713, 11.49999999999998934 ) ) ;
#67814 = ORIENTED_EDGE ( 'NONE', *, *, #31333, .F. ) ;
#67816 = EDGE_LOOP ( 'NONE', ( #65468, #77351, #39223 ) ) ;
#67815 = CARTESIAN_POINT ( 'NONE',  ( 4.451706829556401956, -6.376774720514406525, 18.91922570401084513 ) ) ;
#67817 = B_SPLINE_SURFACE_WITH_KNOTS ( 'NONE', 3, 1, ( 
 ( #4056, #10164 ),
 ( #12148, #48744 ),
 ( #2067, #18276 ),
 ( #33006, #34505 ),
 ( #63981, #35000 ),
 ( #49746, #41124 ),
 ( #42135, #27392 ) ),
 .UNSPECIFIED., .F., .F., .F.,
 ( 4, 1, 1, 1, 4 ),
 ( 2, 2 ),
 ( 0.000000000000000000, 0.2750683690187516461, 0.5329014600899387721, 0.7739734595924534499, 1.000000000000000000 ),
 ( 0.000000000000000000, 1.000000000000000000 ),
 .UNSPECIFIED. ) ;
#67818 = CARTESIAN_POINT ( 'NONE',  ( 30.52397162719526946, -4.695236745772901621, 19.84760796525321425 ) ) ;
#67819 = ORIENTED_EDGE ( 'NONE', *, *, #8293, .T. ) ;
#67820 = EDGE_LOOP ( 'NONE', ( #56005, #58152, #28809, #67440 ) ) ;
#67821 = CARTESIAN_POINT ( 'NONE',  ( -29.49875734969026198, -5.965225279485572685, 2.362022800118626531 ) ) ;
#67822 = CARTESIAN_POINT ( 'NONE',  ( -116.7735416517568297, -25.27125674707836822, 4.078964885054422673 ) ) ;
#67823 = CARTESIAN_POINT ( 'NONE',  ( -86.52287095715007581, -23.94994826722565406, -0.6494450866342726947 ) ) ;
#67824 = CARTESIAN_POINT ( 'NONE',  ( -100.5895376238167245, -25.00182538069145721, 7.747789668545099317 ) ) ;
#67826 = ORIENTED_EDGE ( 'NONE', *, *, #78882, .T. ) ;
#67825 = CARTESIAN_POINT ( 'NONE',  ( -8.904070064990065703, -20.24664451029508783, 11.49999999999999645 ) ) ;
#67827 = CARTESIAN_POINT ( 'NONE',  ( -108.5552614013656978, -23.96119346886881729, -0.6495511937831862648 ) ) ;
#67828 = CARTESIAN_POINT ( 'NONE',  ( -22.13905560727926414, 4.690293145198261904, -1.500000000000002220 ) ) ;
#67829 = VECTOR ( 'NONE', #74839, 1000.000000000000114 ) ;
#67830 = ADVANCED_FACE ( 'NONE', ( #70499 ), #38042, .T. ) ;
#67832 = ORIENTED_EDGE ( 'NONE', *, *, #55526, .F. ) ;
#67831 = CYLINDRICAL_SURFACE ( 'NONE', #16593, 20.00000000000000000 ) ;
#67833 = EDGE_LOOP ( 'NONE', ( #68296, #11489, #51214, #59078 ) ) ;
#67834 = PLANE ( 'NONE',  #93629 ) ;
#67835 = EDGE_CURVE ( 'NONE', #48827, #40589, #65840, .T. ) ;
#67836 = CARTESIAN_POINT ( 'NONE',  ( -18.49208213979201076, -7.923680710433813168, 11.49999999999998934 ) ) ;
#67837 = CARTESIAN_POINT ( 'NONE',  ( -57.61198011476029279, -23.48786465467241058, 11.44779295918254647 ) ) ;
#67838 = ORIENTED_EDGE ( 'NONE', *, *, #71358, .F. ) ;
#67839 = AXIS2_PLACEMENT_3D ( 'NONE', #23679, #55163, #17077 ) ;
#67840 = CARTESIAN_POINT ( 'NONE',  ( -5.366453405989236813, 0.000000000000000000, 0.000000000000000000 ) ) ;
#67841 = CARTESIAN_POINT ( 'NONE',  ( 20.56042274393015035, -8.519965759701490171, -1.500000000000002220 ) ) ;
#67842 = ORIENTED_EDGE ( 'NONE', *, *, #97339, .T. ) ;
#67843 = EDGE_LOOP ( 'NONE', ( #84770, #53205, #25737 ) ) ;
#67844 = CARTESIAN_POINT ( 'NONE',  ( -5.154768636056045850, -6.376774720514413630, 19.48351902941045921 ) ) ;
#67845 = DIRECTION ( 'NONE',  ( -0.000000000000000000, 2.173523156925979552E-06, -0.9999999999976378895 ) ) ;
#67846 = LINE ( 'NONE', #18773, #18190 ) ;
#67847 = CYLINDRICAL_SURFACE ( 'NONE', #42315, 2.040000000000000036 ) ;
#67849 = VECTOR ( 'NONE', #24552, 1000.000000000000114 ) ;
#67848 = CARTESIAN_POINT ( 'NONE',  ( -9.627943313441900131, 16.98966435471970726, -1.500000000000002220 ) ) ;
#67850 = CARTESIAN_POINT ( 'NONE',  ( 1.049947104896167049, -21.43676768134831434, 11.49999999999998934 ) ) ;
#67851 = CARTESIAN_POINT ( 'NONE',  ( -2.794644232660540961, -6.376774720514415407, 20.26757654895259009 ) ) ;
#67852 = FACE_OUTER_BOUND ( 'NONE', #43751, .T. ) ;
#67853 = DIRECTION ( 'NONE',  ( -0.000000000000000000, -0.000000000000000000, 1.000000000000000000 ) ) ;
#67854 = CARTESIAN_POINT ( 'NONE',  ( 19.59772090806136902, -11.66877021596143926, -1.500000000000002220 ) ) ;
#67855 = COORDINATED_UNIVERSAL_TIME_OFFSET ( 0, 0, .AHEAD. ) ;
#67856 = CARTESIAN_POINT ( 'NONE',  ( -96.50857322515494729, -24.51419770103159834, 9.386484678747169852 ) ) ;
#67857 = CYLINDRICAL_SURFACE ( 'NONE', #5339, 0.8160000000000007248 ) ;
#67858 = CARTESIAN_POINT ( 'NONE',  ( -15.89961544564849305, 12.09337254111102844, 11.49999999999999645 ) ) ;
#67859 = CARTESIAN_POINT ( 'NONE',  ( 5.271800844963591359, 0.3587747205143965168, -28.56638892015329745 ) ) ;
#67860 = CARTESIAN_POINT ( 'NONE',  ( -74.49972297989059200, -24.51419770103157703, 9.386484678747164523 ) ) ;
#67861 = DIRECTION ( 'NONE',  ( 0.000000000000000000, 1.000000000000000000, 0.000000000000000000 ) ) ;
#67862 = ORIENTED_EDGE ( 'NONE', *, *, #27316, .F. ) ;
#67863 = CARTESIAN_POINT ( 'NONE',  ( -110.6228709571500559, -29.50248528299804818, 1.056150453629043584 ) ) ;
#67864 = LINE ( 'NONE', #6452, #50712 ) ;
#67865 = CARTESIAN_POINT ( 'NONE',  ( 21.72137571921558319, 1.130696696492564213, -1.500000000000002220 ) ) ;
#67866 = CARTESIAN_POINT ( 'NONE',  ( -4.495793269230770939, -6.376774720514410077, 19.27714342948718595 ) ) ;
#67867 = CARTESIAN_POINT ( 'NONE',  ( 3.881049643139886207, -19.21785841795820104, -1.500000000000002220 ) ) ;
#67868 = CARTESIAN_POINT ( 'NONE',  ( -99.46032996850638597, -25.20155714560419469, 6.668840158564011134 ) ) ;
#67869 = VERTEX_POINT ( 'NONE', #8095 ) ;
#67870 = COORDINATED_UNIVERSAL_TIME_OFFSET ( 0, 0, .AHEAD. ) ;
#67871 = CARTESIAN_POINT ( 'NONE',  ( 14.61581670307174008, -6.376774720514426953, -27.35847990810646024 ) ) ;
#67872 = CARTESIAN_POINT ( 'NONE',  ( 3.632573734185411851, -6.376774720514429617, 21.82795992345630509 ) ) ;
#67873 = CARTESIAN_POINT ( 'NONE',  ( -6.383830130275963910, 19.51498944528526991, 11.49999999999999645 ) ) ;
#67874 = LINE ( 'NONE', #83576, #57107 ) ;
#67875 = CARTESIAN_POINT ( 'NONE',  ( -61.24303164512834030, -25.04307381209219230, 7.563174986197129357 ) ) ;
#67876 = ORIENTED_EDGE ( 'NONE', *, *, #53001, .F. ) ;
#67877 = DIRECTION ( 'NONE',  ( -0.000000000000000000, -0.000000000000000000, 1.000000000000000000 ) ) ;
#67878 = CARTESIAN_POINT ( 'NONE',  ( -40.25588136632453740, -25.18430874478563197, 3.308432125291594250 ) ) ;
#67879 = VECTOR ( 'NONE', #28429, 1000.000000000000000 ) ;
#67881 = EDGE_CURVE ( 'NONE', #98594, #99101, #51250, .T. ) ;
#67880 = CARTESIAN_POINT ( 'NONE',  ( -42.62287095715004881, -29.50250243563736774, 8.947779886222148704 ) ) ;
#67882 = AXIS2_PLACEMENT_3D ( 'NONE', #70561, #47, #38609 ) ;
#67883 = B_SPLINE_CURVE_WITH_KNOTS ( 'NONE', 3,
 ( #21618, #15013, #30237, #68813 ),
 .UNSPECIFIED., .F., .F.,
 ( 4, 4 ),
 ( 0.000000000000000000, 1.000000000000000000 ),
 .UNSPECIFIED. ) ;
#67884 = B_SPLINE_CURVE_WITH_KNOTS ( 'NONE', 3,
 ( #58685, #4899, #11503, #42482 ),
 .UNSPECIFIED., .F., .F.,
 ( 4, 4 ),
 ( 0.000000000000000000, 0.0001000000000000028644 ),
 .UNSPECIFIED. ) ;
#67885 = DIRECTION ( 'NONE',  ( 1.000000000000000000, -0.000000000000000000, -0.000000000000000000 ) ) ;
#67887 = ORIENTED_EDGE ( 'NONE', *, *, #15400, .F. ) ;
#67886 = EDGE_CURVE ( 'NONE', #6280, #27797, #99751, .T. ) ;
#67888 = CARTESIAN_POINT ( 'NONE',  ( -119.6228709571500559, -23.48783264082479150, -1.443836473390058384 ) ) ;
#67889 = CIRCLE ( 'NONE', #75968, 1.325999999999990298 ) ;
#67890 = EDGE_CURVE ( 'NONE', #72942, #7077, #67089, .T. ) ;
#67891 = CARTESIAN_POINT ( 'NONE',  ( 18.09022303007301247, 14.20294132079179938, 11.49999999999999645 ) ) ;
#67892 = CARTESIAN_POINT ( 'NONE',  ( -20.44213351528904354, 10.05872170072450977, -1.500000000000002220 ) ) ;
#67893 = CARTESIAN_POINT ( 'NONE',  ( -70.66110687620329145, -25.31517380081856672, 4.882286551243335992 ) ) ;
#67894 = ADVANCED_FACE ( 'NONE', ( #985 ), #14193, .T. ) ;
#67895 = CARTESIAN_POINT ( 'NONE',  ( -5.457842845122470976, -6.376774720514410077, 19.25892998154168367 ) ) ;
#67896 = DIRECTION ( 'NONE',  ( 0.000000000000000000, -0.8183310589170136318, 0.5747471426738539613 ) ) ;
#67897 = AXIS2_PLACEMENT_3D ( 'NONE', #41812, #49426, #25566 ) ;
#67898 = CARTESIAN_POINT ( 'NONE',  ( -45.62287095715004881, -29.50249982740957577, 7.747779886224967605 ) ) ;
#67899 = ADVANCED_FACE ( 'NONE', ( #100416 ), #62905, .F. ) ;
#67900 = CARTESIAN_POINT ( 'NONE',  ( -69.55620429048337883, -24.64898659630528854, 1.056161002820824368 ) ) ;
#67901 = CARTESIAN_POINT ( 'NONE',  ( 21.88901064076550185, 0.7357440816682787599, -1.500000000000002220 ) ) ;
#67902 = FACE_OUTER_BOUND ( 'NONE', #38682, .T. ) ;
#67903 = LINE ( 'NONE', #61788, #49520 ) ;
#67904 = CARTESIAN_POINT ( 'NONE',  ( -33.52287095715004739, -23.96177878511307924, 10.65340807706330750 ) ) ;
#67905 = CARTESIAN_POINT ( 'NONE',  ( -78.59599014444141574, -23.96119346886880308, -0.6495511937832113558 ) ) ;
#67906 = DIRECTION ( 'NONE',  ( -3.773278334444166432E-23, 1.000000000000000000, 0.000000000000000000 ) ) ;
#67907 = PLANE ( 'NONE',  #95550 ) ;
#67908 = VERTEX_POINT ( 'NONE', #45171 ) ;
#67909 = AXIS2_PLACEMENT_3D ( 'NONE', #87226, #17723, #48691 ) ;
#67910 = CARTESIAN_POINT ( 'NONE',  ( -2.750569593922542300, -20.27526743851804625, 11.49999999999998934 ) ) ;
#67911 = ORIENTED_EDGE ( 'NONE', *, *, #75212, .F. ) ;
#67912 = EDGE_LOOP ( 'NONE', ( #22328, #23596, #28721, #53540 ) ) ;
#67913 = EDGE_LOOP ( 'NONE', ( #48463, #11558, #14258, #74669 ) ) ;
#67914 = ORIENTED_EDGE ( 'NONE', *, *, #44290, .F. ) ;
#67915 = CARTESIAN_POINT ( 'NONE',  ( -20.34888222059871410, 10.79260868881566715, 11.49999999999998934 ) ) ;
#67916 = DIRECTION ( 'NONE',  ( 0.000000000000000000, -0.9999999999976377785, -2.173523156925979975E-06 ) ) ;
#67917 = CARTESIAN_POINT ( 'NONE',  ( -14.69473627950705108, 13.90061564059656440, -1.500000000000002220 ) ) ;
#67918 = ORIENTED_EDGE ( 'NONE', *, *, #77743, .F. ) ;
#67919 = CARTESIAN_POINT ( 'NONE',  ( -27.15236911514251972, -24.75132242458699849, 7.636915180611342002 ) ) ;
#67920 = CARTESIAN_POINT ( 'NONE',  ( -40.58132354090890459, -25.30363535146268816, 5.541646066808135096 ) ) ;
#67921 = CARTESIAN_POINT ( 'NONE',  ( -47.52287095715006160, -23.48783264083458988, -1.443836473374825236 ) ) ;
#67922 = CARTESIAN_POINT ( 'NONE',  ( -70.54351358342104561, -24.52300882791528380, 0.6510814631126248253 ) ) ;
#67924 = ORIENTED_EDGE ( 'NONE', *, *, #53445, .F. ) ;
#67923 = CARTESIAN_POINT ( 'NONE',  ( -11.90495014755217618, 17.82271480561356469, 11.49999999999999645 ) ) ;
#67925 = B_SPLINE_CURVE_WITH_KNOTS ( 'NONE', 3,
 ( #85288, #95412, #96412, #95910, #56871, #33018 ),
 .UNSPECIFIED., .F., .F.,
 ( 4, 2, 4 ),
 ( 6.391158118969315506E-06, 0.001387004593080790266, 0.002767618028042611537 ),
 .UNSPECIFIED. ) ;
#67926 = DIRECTION ( 'NONE',  ( 0.000000000000000000, -1.000000000000000000, 0.000000000000000000 ) ) ;
#67927 = CARTESIAN_POINT ( 'NONE',  ( -41.59371986446371494, -24.15543982623907127, -0.2315651400026566831 ) ) ;
#67928 = ORIENTED_EDGE ( 'NONE', *, *, #25599, .T. ) ;
#67929 = B_SPLINE_CURVE_WITH_KNOTS ( 'NONE', 3,
 ( #95121, #56579, #34231, #79887, #34723, #65204 ),
 .UNSPECIFIED., .F., .F.,
 ( 4, 2, 4 ),
 ( 0.000000000000000000, 0.001380764517853247733, 0.002761529035706495466 ),
 .UNSPECIFIED. ) ;
#67930 = CARTESIAN_POINT ( 'NONE',  ( -19.01758589260300525, -8.224767016273846210, -1.500000000000002220 ) ) ;
#67931 = VERTEX_POINT ( 'NONE', #22299 ) ;
#67932 = CARTESIAN_POINT ( 'NONE',  ( -91.52287095715011844, -24.51387760970726504, 9.387446482453416507 ) ) ;
#67933 = ORIENTED_EDGE ( 'NONE', *, *, #36971, .F. ) ;
#67934 = CARTESIAN_POINT ( 'NONE',  ( 4.190829928318763109, -5.876774720514399419, 18.23548058298382557 ) ) ;
#67935 = VERTEX_POINT ( 'NONE', #8599 ) ;
#67936 = CARTESIAN_POINT ( 'NONE',  ( 19.54352652498339182, 7.673529024697476331, -1.500000000000002220 ) ) ;
#67937 = CARTESIAN_POINT ( 'NONE',  ( -19.92591009635028243, 9.278653061003369729, 11.49999999999999645 ) ) ;
#67938 = CARTESIAN_POINT ( 'NONE',  ( 8.160000000000000142, -9.728493947732140157, 1.239948043688426926 ) ) ;
#67939 = CARTESIAN_POINT ( 'NONE',  ( 15.74396088501716839, 16.14010210793005839, 11.49999999999998934 ) ) ;
#67940 = CARTESIAN_POINT ( 'NONE',  ( -20.92093621315066443, -1.481899440790641842, -1.500000000000002220 ) ) ;
#67941 = CARTESIAN_POINT ( 'NONE',  ( -48.62287095715004881, -23.48783264082478439, -1.443836473390070596 ) ) ;
#67942 = CARTESIAN_POINT ( 'NONE',  ( -6.499999999999992895, 0.9999999999999993339, 3.499999999999998668 ) ) ;
#67943 = CARTESIAN_POINT ( 'NONE',  ( 8.197725756732245017, -0.4963810196290975307, -3.727086380289611256 ) ) ;
#67944 = EDGE_LOOP ( 'NONE', ( #4798, #12496, #69910, #39502 ) ) ;
#67945 = ORIENTED_EDGE ( 'NONE', *, *, #17601, .F. ) ;
#67946 = ORIENTED_EDGE ( 'NONE', *, *, #69992, .F. ) ;
#67947 = CARTESIAN_POINT ( 'NONE',  ( -66.54902258912107982, -24.15543982623906771, -0.2315651400026687845 ) ) ;
#67948 = EDGE_CURVE ( 'NONE', #48682, #68549, #68995, .T. ) ;
#67949 = CARTESIAN_POINT ( 'NONE',  ( 8.900169022907615357, -19.58186849131130813, -1.500000000000002220 ) ) ;
#67950 = EDGE_CURVE ( 'NONE', #58159, #80349, #54374, .T. ) ;
#67951 = CARTESIAN_POINT ( 'NONE',  ( -121.5895376238167103, -24.66019654487200086, 8.947790411086115725 ) ) ;
#67952 = ORIENTED_EDGE ( 'NONE', *, *, #7411, .F. ) ;
#67953 = CARTESIAN_POINT ( 'NONE',  ( 14.88031740681034698, -14.96734982212533183, -1.500000000000002220 ) ) ;
#67954 = FACE_OUTER_BOUND ( 'NONE', #2743, .T. ) ;
#67955 = DIRECTION ( 'NONE',  ( -0.8244855201331809935, 1.229959914849042681E-06, -0.5658830507173768787 ) ) ;
#67956 = CARTESIAN_POINT ( 'NONE',  ( 3.750000000000001332, 25.69999999999999574, 0.000000000000000000 ) ) ;
#67957 = LINE ( 'NONE', #66484, #41028 ) ;
#67958 = CARTESIAN_POINT ( 'NONE',  ( -100.1148124853301340, -25.11623808430151072, 2.865158905384864951 ) ) ;
#67959 = CARTESIAN_POINT ( 'NONE',  ( 12.17348956504948987, -18.45705692928949659, -1.500000000000002220 ) ) ;
#67960 = CARTESIAN_POINT ( 'NONE',  ( 10.46399479596396453, -2.682774720514426559, -27.03001098546561920 ) ) ;
#67961 = ORIENTED_EDGE ( 'NONE', *, *, #80360, .F. ) ;
#67962 = CARTESIAN_POINT ( 'NONE',  ( -56.52287095715008292, -24.50321055353803956, 9.387540953477522265 ) ) ;
#67963 = CARTESIAN_POINT ( 'NONE',  ( -79.62287095715005592, -24.33832256527048798, 0.1851278514138599840 ) ) ;
#67964 = CARTESIAN_POINT ( 'NONE',  ( -99.52287095715006160, -23.47596703998600631, 11.44779298504228215 ) ) ;
#67966 = VECTOR ( 'NONE', #87890, 1000.000000000000114 ) ;
#67965 = B_SPLINE_CURVE_WITH_KNOTS ( 'NONE', 3,
 ( #93678, #16051, #6949, #62251, #37903, #15554 ),
 .UNSPECIFIED., .F., .F.,
 ( 4, 2, 4 ),
 ( 1.570887131794176733E-05, 0.001396322306279756519, 0.002776935741241571502 ),
 .UNSPECIFIED. ) ;
#67967 = CARTESIAN_POINT ( 'NONE',  ( -97.52287095715004739, -24.50321055353804667, 9.387540953477522265 ) ) ;
#67968 = AXIS2_PLACEMENT_3D ( 'NONE', #79733, #63536, #16331 ) ;
#67969 = CARTESIAN_POINT ( 'NONE',  ( -9.780116039169133302, 16.78644576961053048, 11.49999999999998934 ) ) ;
#67970 = AXIS2_PLACEMENT_3D ( 'NONE', #65921, #51675, #67402 ) ;
#67971 = CARTESIAN_POINT ( 'NONE',  ( 11.27511198983438412, 18.17944245918264912, -1.500000000000002220 ) ) ;
#67972 = CARTESIAN_POINT ( 'NONE',  ( 16.36243866176394945, 0.000000000000000000, 0.000000000000000000 ) ) ;
#67973 = CARTESIAN_POINT ( 'NONE',  ( -91.16165857266686601, -25.26877915520014639, 5.947789088310639904 ) ) ;
#67974 = CARTESIAN_POINT ( 'NONE',  ( -40.52287095715005449, -25.00158670708908915, 2.256160236439166411 ) ) ;
#67975 = CYLINDRICAL_SURFACE ( 'NONE', #81651, 27.94799999999999685 ) ;
#67976 = CARTESIAN_POINT ( 'NONE',  ( 22.15051849217804403, -4.756829024181505439, -1.500000000000002220 ) ) ;
#67977 = VECTOR ( 'NONE', #60467, 1000.000000000000000 ) ;
#67978 = ORIENTED_EDGE ( 'NONE', *, *, #87470, .T. ) ;
#67979 = CARTESIAN_POINT ( 'NONE',  ( -119.5228709571500474, -23.47593901973090524, -1.443836447538996204 ) ) ;
#67980 = DIRECTION ( 'NONE',  ( -1.000000000000000000, -3.773278334444166432E-23, -8.201307841325785021E-29 ) ) ;
#67981 = CARTESIAN_POINT ( 'NONE',  ( -1.996473883165060581, 19.68112600131995293, 11.49999999999999645 ) ) ;
#67982 = CARTESIAN_POINT ( 'NONE',  ( -67.52287095715009002, -23.48783264082477018, -1.443836473390090802 ) ) ;
#67983 = ORIENTED_EDGE ( 'NONE', *, *, #17885, .T. ) ;
#67984 = CARTESIAN_POINT ( 'NONE',  ( -59.52287095715008292, -23.72747288104470798, -1.053458166803227014 ) ) ;
#67985 = DIRECTION ( 'NONE',  ( 0.000000000000000000, -2.173523156925979552E-06, 0.9999999999976378895 ) ) ;
#67986 = CARTESIAN_POINT ( 'NONE',  ( -5.517532219241116032, 20.92096086382833064, 11.49999999999998934 ) ) ;
#67987 = CARTESIAN_POINT ( 'NONE',  ( -99.62287095715007013, -24.34917612406838217, 0.1852690917426680350 ) ) ;
#67988 = CARTESIAN_POINT ( 'NONE',  ( 18.67713048845720181, -5.233370074711279685, -1.500000000000002220 ) ) ;
#67989 = CARTESIAN_POINT ( 'NONE',  ( -61.62287095715007723, -24.34917612406837506, 0.1852690917426614847 ) ) ;
#67990 = LINE ( 'NONE', #6073, #79818 ) ;
#67991 = CARTESIAN_POINT ( 'NONE',  ( -4.105667982141768313, -19.37954422259287668, 11.49999999999998934 ) ) ;
#67992 = ORIENTED_EDGE ( 'NONE', *, *, #50823, .F. ) ;
#67993 = CARTESIAN_POINT ( 'NONE',  ( 18.91379238805564356, 7.493326543281090935, 11.49999999999999645 ) ) ;
#67994 = CARTESIAN_POINT ( 'NONE',  ( -111.5228709571500758, -24.66019654487200441, 8.947790411086108620 ) ) ;
#67995 = CARTESIAN_POINT ( 'NONE',  ( 32.98371819488264833, -4.742969794006914874, -11.67826368001470172 ) ) ;
#67996 = ORIENTED_EDGE ( 'NONE', *, *, #7994, .T. ) ;
#67997 = B_SPLINE_SURFACE_WITH_KNOTS ( 'NONE', 3, 1, ( 
 ( #11971, #66786 ),
 ( #3879, #97703 ),
 ( #28198, #12956 ),
 ( #43925, #50050 ),
 ( #34817, #84473 ),
 ( #60660, #61162 ),
 ( #84967, #83470 ),
 ( #6358, #6849 ),
 ( #29690, #52534 ),
 ( #53542, #14953 ),
 ( #37804, #69754 ),
 ( #45432, #15453 ),
 ( #92574, #30684 ),
 ( #75854, #92081 ),
 ( #54529, #61655 ),
 ( #53043, #83973 ),
 ( #23052, #22551 ),
 ( #13957, #5855 ),
 ( #75355, #67779 ) ),
 .UNSPECIFIED., .F., .F., .F.,
 ( 4, 1, 1, 1, 1, 1, 1, 1, 1, 1, 1, 1, 1, 1, 1, 1, 4 ),
 ( 2, 2 ),
 ( 0.000000000000000000, 0.06976287284686377710, 0.1345149942976648916, 0.1951193525406907936, 0.2509143402908634579, 0.3026968495153156136, 0.3502960464810115360, 0.3933858467586648366, 0.4329734110072616105, 0.5070892430766307246, 0.5787491638444315356, 0.6502280224451015833, 0.7224618180302719850, 0.7938856428547010902, 0.8631290414909040809, 0.9313229315869651082, 1.000000000000000000 ),
 ( 0.000000000000000000, 1.000000000000000000 ),
 .UNSPECIFIED. ) ;
#67998 = CARTESIAN_POINT ( 'NONE',  ( -102.6311381732150494, -23.96169478059713498, 10.65365249895717881 ) ) ;
#67999 = CARTESIAN_POINT ( 'NONE',  ( -29.49875734969026198, 5.965225279485572685, 2.362022800118626531 ) ) ;
#68000 = DIRECTION ( 'NONE',  ( -3.773278334453080206E-23, 0.9999999999976377785, 2.173523156925979975E-06 ) ) ;
#68001 = CARTESIAN_POINT ( 'NONE',  ( -47.58953762381673158, -23.47593901973091235, -1.443836447539009749 ) ) ;
#68002 = CARTESIAN_POINT ( 'NONE',  ( -51.52764846858840997, -25.24768739062223943, 6.187572788000800017 ) ) ;
#68003 = CARTESIAN_POINT ( 'NONE',  ( -18.81522532469529452, 6.996975221643539911, -1.500000000000002220 ) ) ;
#68004 = CARTESIAN_POINT ( 'NONE',  ( -120.6228709571500559, -25.00182538069145721, 7.747789668545100206 ) ) ;
#68005 = ORIENTED_EDGE ( 'NONE', *, *, #35685, .T. ) ;
#68006 = CARTESIAN_POINT ( 'NONE',  ( -4.141025641025642301, -5.876774720514412742, 19.63681891025641235 ) ) ;
#68007 = CARTESIAN_POINT ( 'NONE',  ( -10.93939140624874007, -20.02795264745160608, 11.49999999999999645 ) ) ;
#68008 = CARTESIAN_POINT ( 'NONE',  ( -49.57368764975930731, -25.26258781768282446, 4.259412078242385213 ) ) ;
#68009 = EDGE_CURVE ( 'NONE', #56523, #47938, #52779, .T. ) ;
#68010 = DIRECTION ( 'NONE',  ( -0.7071067811865452413, 0.000000000000000000, 0.7071067811865497932 ) ) ;
#68011 = DIRECTION ( 'NONE',  ( -3.773278334453079618E-23, 0.9999999999976377785, 2.173523156925979975E-06 ) ) ;
#68012 = EDGE_CURVE ( 'NONE', #91984, #67600, #85215, .T. ) ;
#68013 = CARTESIAN_POINT ( 'NONE',  ( 6.251785340501501587, -5.876774720514423400, 21.46941214867599612 ) ) ;
#68014 = B_SPLINE_CURVE_WITH_KNOTS ( 'NONE', 3,
 ( #80537, #72440, #71436, #11031 ),
 .UNSPECIFIED., .F., .F.,
 ( 4, 4 ),
 ( 0.7092829846576129693, 0.7102837316983785509 ),
 .UNSPECIFIED. ) ;
#68015 = VECTOR ( 'NONE', #95292, 1000.000000000000000 ) ;
#68016 = CARTESIAN_POINT ( 'NONE',  ( -80.62287095715005592, -29.50249982740957577, 7.747779886224967605 ) ) ;
#68017 = LINE ( 'NONE', #29435, #22588 ) ;
#68018 = ORIENTED_EDGE ( 'NONE', *, *, #39669, .F. ) ;
#68019 = VECTOR ( 'NONE', #3406, 1000.000000000000114 ) ;
#68020 = CARTESIAN_POINT ( 'NONE',  ( 15.61528876134825161, -13.05345633644532732, 11.49999999999998934 ) ) ;
#68021 = VERTEX_POINT ( 'NONE', #85214 ) ;
#68022 = EDGE_CURVE ( 'NONE', #55708, #47794, #64571, .T. ) ;
#68023 = CARTESIAN_POINT ( 'NONE',  ( 1.269710630819723463, 22.90746787927615102, 11.49999999999998934 ) ) ;
#68024 = CARTESIAN_POINT ( 'NONE',  ( 13.91401389203221406, 5.965225279485572685, 158.0376437107427137 ) ) ;
#68025 = VERTEX_POINT ( 'NONE', #478 ) ;
#68026 = VECTOR ( 'NONE', #82153, 1000.000000000000000 ) ;
#68027 = CARTESIAN_POINT ( 'NONE',  ( -101.4435148696508406, -25.21059354442303047, 6.520239176572899531 ) ) ;
#68028 = CARTESIAN_POINT ( 'NONE',  ( -67.52287095715007581, -23.72773821059536559, 11.05748984161097326 ) ) ;
#68029 = VECTOR ( 'NONE', #127, 1000.000000000000114 ) ;
#68030 = CARTESIAN_POINT ( 'NONE',  ( -51.58226167061351219, -24.51419770103156637, 9.386484678747176957 ) ) ;
#68032 = ORIENTED_EDGE ( 'NONE', *, *, #1858, .T. ) ;
#68031 = CARTESIAN_POINT ( 'NONE',  ( 4.782327729912362990, -20.71560727227588927, 11.49999999999999645 ) ) ;
#68033 = AXIS2_PLACEMENT_3D ( 'NONE', #34538, #73597, #64516 ) ;
#68034 = ORIENTED_EDGE ( 'NONE', *, *, #11150, .T. ) ;
#68035 = CARTESIAN_POINT ( 'NONE',  ( 17.07819277939130842, -14.19623557145530057, -1.500000000000002220 ) ) ;
#68036 = CARTESIAN_POINT ( 'NONE',  ( -9.157874670058189892, -18.46812626297970539, -1.500000000000002220 ) ) ;
#68038 = ORIENTED_EDGE ( 'NONE', *, *, #27799, .T. ) ;
#68037 = AXIS2_PLACEMENT_3D ( 'NONE', #65111, #40745, #88426 ) ;
#68039 = ORIENTED_EDGE ( 'NONE', *, *, #74397, .T. ) ;
#68040 = PLANE ( 'NONE',  #72262 ) ;
#68041 = CARTESIAN_POINT ( 'NONE',  ( -56.62287095715006302, -23.73907113216990794, -1.053371485793233031 ) ) ;
#68042 = ORIENTED_EDGE ( 'NONE', *, *, #27693, .F. ) ;
#68043 = ORIENTED_EDGE ( 'NONE', *, *, #81458, .T. ) ;
#68044 = CARTESIAN_POINT ( 'NONE',  ( 30.57061049414810228, 4.696956328126698388, 25.28683757526521703 ) ) ;
#68045 = CARTESIAN_POINT ( 'NONE',  ( -75.62287095715005592, -23.47596703998600631, 11.44779298504227860 ) ) ;
#68046 = FACE_OUTER_BOUND ( 'NONE', #41965, .T. ) ;
#68047 = CARTESIAN_POINT ( 'NONE',  ( 19.40640353424967302, -7.489167304209242815, -1.500000000000002220 ) ) ;
#68048 = CARTESIAN_POINT ( 'NONE',  ( 15.22768361601695020, -15.61070304372801587, 11.49999999999999645 ) ) ;
#68049 = CARTESIAN_POINT ( 'NONE',  ( -51.91081924717653351, -25.22346074172688901, 6.413989918693766334 ) ) ;
#68050 = LINE ( 'NONE', #52819, #43424 ) ;
#68051 = CARTESIAN_POINT ( 'NONE',  ( -17.93832129671990572, 13.47109510200611560, -1.500000000000002220 ) ) ;
#68052 = CARTESIAN_POINT ( 'NONE',  ( -49.10457154551148307, -29.50249168100820896, 3.999763059310747160 ) ) ;
#68054 = EDGE_CURVE ( 'NONE', #96886, #30238, #42813, .T. ) ;
#68053 = ORIENTED_EDGE ( 'NONE', *, *, #45998, .T. ) ;
#68055 = B_SPLINE_CURVE_WITH_KNOTS ( 'NONE', 3,
 ( #59216, #27762, #66349, #4437, #99257, #74916 ),
 .UNSPECIFIED., .F., .F.,
 ( 4, 2, 4 ),
 ( 0.000000000000000000, 0.001380901958385387894, 0.002761803916770775788 ),
 .UNSPECIFIED. ) ;
#68056 = CARTESIAN_POINT ( 'NONE',  ( -71.69006450592775082, -25.27819024002308268, 5.957498326979273173 ) ) ;
#68057 = CARTESIAN_POINT ( 'NONE',  ( 32.48725517365867432, 4.170878844625590887, -0.8993273505261454304 ) ) ;
#68058 = EDGE_LOOP ( 'NONE', ( #92615, #29792, #83198, #67559 ) ) ;
#68059 = EDGE_LOOP ( 'NONE', ( #76835, #39595, #62922, #92594, #19720, #4100 ) ) ;
#68060 = FACE_OUTER_BOUND ( 'NONE', #82095, .T. ) ;
#68061 = EDGE_CURVE ( 'NONE', #65082, #95862, #31432, .T. ) ;
#68062 = EDGE_LOOP ( 'NONE', ( #12236, #65505, #65209, #33621 ) ) ;
#68063 = CARTESIAN_POINT ( 'NONE',  ( 20.93798385506118365, 3.901641247904229282, -1.500000000000002220 ) ) ;
#68064 = VERTEX_POINT ( 'NONE', #86219 ) ;
#68065 = DIRECTION ( 'NONE',  ( 0.000000000000000000, 0.000000000000000000, -1.000000000000000000 ) ) ;
#68066 = CARTESIAN_POINT ( 'NONE',  ( -20.81348254183067681, -2.960215062046979373, 11.49999999999998934 ) ) ;
#68067 = CARTESIAN_POINT ( 'NONE',  ( -38.52287095715006870, -23.47596703998600631, 11.44779298504229281 ) ) ;
#68068 = CARTESIAN_POINT ( 'NONE',  ( -41.44993916608342488, -25.18431026911753889, 4.009750576414989887 ) ) ;
#68069 = CARTESIAN_POINT ( 'NONE',  ( -32.07722060962682775, -29.50248914092071928, 2.831113219569932227 ) ) ;
#68070 = CARTESIAN_POINT ( 'NONE',  ( -12.72821696145241255, -17.84489267850806726, -1.500000000000002220 ) ) ;
#68071 = CARTESIAN_POINT ( 'NONE',  ( -87.50497043089684723, -24.51314013834317507, 0.6176544820404262781 ) ) ;
#68072 = ORIENTED_EDGE ( 'NONE', *, *, #59545, .F. ) ;
#68073 = CARTESIAN_POINT ( 'NONE',  ( -122.6271177707151878, -23.48786465467241769, 11.44779295918253581 ) ) ;
#68074 = CARTESIAN_POINT ( 'NONE',  ( -120.5228709571500190, -24.91544648472626378, 1.928969306349433976 ) ) ;
#68075 = CARTESIAN_POINT ( 'NONE',  ( -41.62287095715006302, -24.65952944569303895, 1.056160979905692576 ) ) ;
#68076 = CARTESIAN_POINT ( 'NONE',  ( -30.63910746512184247, -23.78113234500525408, 10.97511746239722186 ) ) ;
#68077 = CARTESIAN_POINT ( 'NONE',  ( 19.98943718749924159, -7.363913660680385220, 11.49999999999998934 ) ) ;
#68078 = FACE_OUTER_BOUND ( 'NONE', #12903, .T. ) ;
#68079 = DIRECTION ( 'NONE',  ( -1.000000000000000000, 0.000000000000000000, 0.000000000000000000 ) ) ;
#68080 = VECTOR ( 'NONE', #24086, 1000.000000000000000 ) ;
#68081 = FACE_OUTER_BOUND ( 'NONE', #27039, .T. ) ;
#68082 = CARTESIAN_POINT ( 'NONE',  ( -70.52287095715009002, -23.84047902841604838, -0.8780736468305397890 ) ) ;
#68083 = CC_DESIGN_PERSON_AND_ORGANIZATION_ASSIGNMENT ( #14037, #84058, ( #40782 ) ) ;
#68084 = CARTESIAN_POINT ( 'NONE',  ( -6.794891441663577503, 21.43730618243864683, -1.500000000000002220 ) ) ;
#68085 = CARTESIAN_POINT ( 'NONE',  ( -108.8781268588537046, -25.11552134530501590, 2.805129186380272088 ) ) ;
#68086 = ORIENTED_EDGE ( 'NONE', *, *, #51502, .F. ) ;
#68087 = CARTESIAN_POINT ( 'NONE',  ( -30.47287095715008576, -23.47593902499770380, -1.441415665115638456 ) ) ;
#68088 = CARTESIAN_POINT ( 'NONE',  ( 10.71975780190685690, -16.47196428025586812, 11.49999999999999645 ) ) ;
#68089 = DIRECTION ( 'NONE',  ( -2.417950247244706201E-16, 0.000000000000000000, 1.000000000000000000 ) ) ;
#68090 = VECTOR ( 'NONE', #65189, 1000.000000000000227 ) ;
#68091 = B_SPLINE_CURVE_WITH_KNOTS ( 'NONE', 3,
 ( #596, #46780, #38657, #84831, #16322, #14810, #100034, #31547 ),
 .UNSPECIFIED., .F., .F.,
 ( 4, 2, 2, 4 ),
 ( -0.001224873891641421308, -0.0002244903592271061104, 0.0007758931731872090870, 0.002776660238015835145 ),
 .UNSPECIFIED. ) ;
#68092 = CARTESIAN_POINT ( 'NONE',  ( -89.81226385320381667, -25.26877915520014994, 5.947789088310639904 ) ) ;
#68093 = ORIENTED_EDGE ( 'NONE', *, *, #88499, .T. ) ;
#68094 = CARTESIAN_POINT ( 'NONE',  ( -69.26415293485048608, -25.30211383818459581, 5.299568534518257046 ) ) ;
#68095 = CARTESIAN_POINT ( 'NONE',  ( -36.52287095715009002, -24.33927499327854349, 9.819080762295813614 ) ) ;
#68096 = ADVANCED_FACE ( 'NONE', ( #17708 ), #79095, .T. ) ;
#68097 = CARTESIAN_POINT ( 'NONE',  ( -100.0218067620262303, -25.25095795709099278, 5.284572167519165475 ) ) ;
#68098 = CARTESIAN_POINT ( 'NONE',  ( 29.57907552799942508, -3.316774720514426456, 29.21818156447043791 ) ) ;
#68099 = CARTESIAN_POINT ( 'NONE',  ( -10.80270875523330965, -16.48872379891551532, 11.49999999999998934 ) ) ;
#68100 = VECTOR ( 'NONE', #75417, 1000.000000000000000 ) ;
#68101 = ORIENTED_EDGE ( 'NONE', *, *, #2132, .T. ) ;
#68102 = VECTOR ( 'NONE', #58162, 1000.000000000000000 ) ;
#68103 = PLANE ( 'NONE',  #14827 ) ;
#68104 = CARTESIAN_POINT ( 'NONE',  ( -28.62287095715004881, -23.31954350884483773, -1.443835782653508426 ) ) ;
#68105 = B_SPLINE_CURVE_WITH_KNOTS ( 'NONE', 3,
 ( #53977, #68697, #30618, #69694 ),
 .UNSPECIFIED., .F., .F.,
 ( 4, 4 ),
 ( 0.04052894072451945079, 0.04953537199663500534 ),
 .UNSPECIFIED. ) ;
#68106 = AXIS2_PLACEMENT_3D ( 'NONE', #10680, #79683, #94908 ) ;
#68107 = APPROVAL_STATUS ( 'not_yet_approved' ) ;
#68108 = EDGE_LOOP ( 'NONE', ( #58471, #9470, #45295, #20936, #47472 ) ) ;
#68109 = DIRECTION ( 'NONE',  ( -0.000000000000000000, 1.000000000000000000, -0.000000000000000000 ) ) ;
#68110 = CARTESIAN_POINT ( 'NONE',  ( -87.55620429048339304, -24.64965694238575011, 8.947790433994194714 ) ) ;
#68111 = CARTESIAN_POINT ( 'NONE',  ( -90.55620429048340725, -23.48786465467241413, 11.44779295918254647 ) ) ;
#68112 = CARTESIAN_POINT ( 'NONE',  ( -118.5911711821453451, -23.96119346886881374, -0.6495511937832023630 ) ) ;
#68113 = DIRECTION ( 'NONE',  ( -0.7689940216596065081, 4.164321980682960499E-15, 0.6392559695863502256 ) ) ;
#68114 = CARTESIAN_POINT ( 'NONE',  ( -69.79628282111092119, -25.24515073828506928, 5.458995855196883795 ) ) ;
#68115 = CARTESIAN_POINT ( 'NONE',  ( -112.5228709571500616, -24.33832256527048798, 0.1851278514138649522 ) ) ;
#68117 = ADVANCED_FACE ( 'NONE', ( #55286 ), #71507, .T. ) ;
#68116 = CARTESIAN_POINT ( 'NONE',  ( -4.560224734120114753, 19.45435480350565882, 11.49999999999998934 ) ) ;
#68118 = CARTESIAN_POINT ( 'NONE',  ( -45.55620429048340014, -23.47593901973091235, -1.443836447539009749 ) ) ;
#68119 = CARTESIAN_POINT ( 'NONE',  ( -45.53131674849007027, -24.73531770709094957, 8.716586749053515604 ) ) ;
#68120 = ORIENTED_EDGE ( 'NONE', *, *, #19012, .F. ) ;
#68121 = FACE_OUTER_BOUND ( 'NONE', #7336, .T. ) ;
#68122 = CARTESIAN_POINT ( 'NONE',  ( -28.98875734969026396, 6.376774720514426953, -0.08597719988137648983 ) ) ;
#68123 = CARTESIAN_POINT ( 'NONE',  ( -80.53951186416253449, -24.83644354573579349, 8.397322867130094792 ) ) ;
#68124 = CARTESIAN_POINT ( 'NONE',  ( -81.62287095715005592, -23.48783264082478794, -1.443836473390065711 ) ) ;
#68125 = CARTESIAN_POINT ( 'NONE',  ( -107.5895376238167245, -24.66019654487199375, 8.947790411086121054 ) ) ;
#68126 = EDGE_CURVE ( 'NONE', #36399, #35863, #9596, .T. ) ;
#68127 = CARTESIAN_POINT ( 'NONE',  ( -97.55620429048339304, -24.65952944569304606, 1.056160979905701236 ) ) ;
#68128 = CARTESIAN_POINT ( 'NONE',  ( -1.428094109758638819, -5.876774720514415407, 20.04104409779160179 ) ) ;
#68129 = CARTESIAN_POINT ( 'NONE',  ( -6.775140224358976226, -6.376774720514408301, 19.14743589743590846 ) ) ;
#68130 = CARTESIAN_POINT ( 'NONE',  ( 0.3627416911114360598, -5.876774720514411854, 19.59793130852656873 ) ) ;
#68131 = ORIENTED_EDGE ( 'NONE', *, *, #60145, .F. ) ;
#68132 = CARTESIAN_POINT ( 'NONE',  ( -19.34540493331696354, 6.066486871809979142, -1.500000000000002220 ) ) ;
#68133 = CARTESIAN_POINT ( 'NONE',  ( 30.43908124610670285, -1.477225279485574028, -13.86910542224428866 ) ) ;
#68134 = EDGE_CURVE ( 'NONE', #84065, #26881, #60964, .T. ) ;
#68135 = DIRECTION ( 'NONE',  ( 1.000000000000000000, -0.000000000000000000, -0.000000000000000000 ) ) ;
#68136 = CARTESIAN_POINT ( 'NONE',  ( -76.62287095715002749, -23.73907113216991860, -1.053371485793229034 ) ) ;
#68137 = ORIENTED_EDGE ( 'NONE', *, *, #55055, .F. ) ;
#68138 = DIRECTION ( 'NONE',  ( -0.9890158633619160478, -0.1478094111296159863, 0.000000000000000000 ) ) ;
#68139 = CARTESIAN_POINT ( 'NONE',  ( -1.390986686320385468, -6.376774720514413630, 19.62288733224860948 ) ) ;
#68140 = CARTESIAN_POINT ( 'NONE',  ( 4.949566031639514918, 19.51814346981619863, -1.500000000000002220 ) ) ;
#68141 = CARTESIAN_POINT ( 'NONE',  ( 1.225302832070333636, 21.05158420706169764, 11.49999999999999645 ) ) ;
#68142 = PLANE ( 'NONE',  #67690 ) ;
#68143 = CARTESIAN_POINT ( 'NONE',  ( 17.94654606563480215, 12.89224558282342947, 11.49999999999998934 ) ) ;
#68144 = VECTOR ( 'NONE', #53586, 1000.000000000000114 ) ;
#68145 = CARTESIAN_POINT ( 'NONE',  ( 19.76637988705548210, 5.604140092158477415, 11.49999999999998934 ) ) ;
#68146 = CARTESIAN_POINT ( 'NONE',  ( -96.52287095715006160, -24.64898659630528499, 1.056161002820829697 ) ) ;
#68147 = PLANE ( 'NONE',  #53316 ) ;
#68148 = EDGE_LOOP ( 'NONE', ( #54905, #68173, #58218, #12787 ) ) ;
#68149 = CARTESIAN_POINT ( 'NONE',  ( 27.53860345374808105, 1.477225279485574028, -1.272392034746785860 ) ) ;
#68150 = ORIENTED_EDGE ( 'NONE', *, *, #19531, .T. ) ;
#68151 = DIRECTION ( 'NONE',  ( -1.000000000000000000, -0.000000000000000000, 0.000000000000000000 ) ) ;
#68152 = CARTESIAN_POINT ( 'NONE',  ( 31.27206728860909024, -4.132774720514318822, -3.930752063305056332 ) ) ;
#68153 = VERTEX_POINT ( 'NONE', #24810 ) ;
#68154 = EDGE_LOOP ( 'NONE', ( #13318, #59441, #35176, #31874 ) ) ;
#68155 = CARTESIAN_POINT ( 'NONE',  ( -118.6228709571500559, -23.47593901973091235, -1.443836447538997536 ) ) ;
#68156 = DIRECTION ( 'NONE',  ( 0.000000000000000000, 0.000000000000000000, -1.000000000000000000 ) ) ;
#68157 = CARTESIAN_POINT ( 'NONE',  ( -76.64295899339111884, -23.73766607897670866, -1.055555164236452681 ) ) ;
#68158 = CARTESIAN_POINT ( 'NONE',  ( -10.41206725544052780, -17.73373708237225799, -1.500000000000002220 ) ) ;
#68159 = CARTESIAN_POINT ( 'NONE',  ( -4.285004571687458963, -21.18589511591401831, 11.49999999999999645 ) ) ;
#68160 = ORIENTED_EDGE ( 'NONE', *, *, #59124, .T. ) ;
#68161 = PLANE ( 'NONE',  #4527 ) ;
#68162 = DIRECTION ( 'NONE',  ( 3.773278334444167608E-23, -1.000000000000000000, 0.000000000000000000 ) ) ;
#68163 = CARTESIAN_POINT ( 'NONE',  ( 22.31825301297700648, 1.237144038376295274, 11.49999999999998934 ) ) ;
#68164 = DIRECTION ( 'NONE',  ( 0.000000000000000000, -1.000000000000000000, 0.000000000000000000 ) ) ;
#68165 = CARTESIAN_POINT ( 'NONE',  ( -17.66201745896767505, -6.376774720514425177, -23.06272557202527906 ) ) ;
#68166 = ORIENTED_EDGE ( 'NONE', *, *, #93050, .F. ) ;
#68167 = CARTESIAN_POINT ( 'NONE',  ( -94.52287095715006160, -23.96127896941631974, -0.6493128931037982499 ) ) ;
#68168 = VECTOR ( 'NONE', #8690, 1000.000000000000000 ) ;
#68169 = CARTESIAN_POINT ( 'NONE',  ( 6.546094359317672584, -6.376774720514411854, 19.73546617144828375 ) ) ;
#68170 = CARTESIAN_POINT ( 'NONE',  ( 6.973883220674568229, 19.69035807221911938, -1.500000000000002220 ) ) ;
#68171 = ORIENTED_EDGE ( 'NONE', *, *, #100279, .F. ) ;
#68173 = ORIENTED_EDGE ( 'NONE', *, *, #11745, .F. ) ;
#68172 = CARTESIAN_POINT ( 'NONE',  ( -28.98875734969026396, 0.3587747205144262708, 0.1180228001186258285 ) ) ;
#68174 = ORIENTED_EDGE ( 'NONE', *, *, #67768, .F. ) ;
#68175 = AXIS2_PLACEMENT_3D ( 'NONE', #60738, #21640, #22142 ) ;
#68176 = ADVANCED_FACE ( 'NONE', ( #94826 ), #3665, .T. ) ;
#68177 = CARTESIAN_POINT ( 'NONE',  ( -51.28881298620314766, -25.27220106976723457, 4.100648920822429488 ) ) ;
#68178 = CARTESIAN_POINT ( 'NONE',  ( 10.59196434753715010, 18.29633683537252509, -1.500000000000002220 ) ) ;
#68179 = ORIENTED_EDGE ( 'NONE', *, *, #42463, .T. ) ;
#68180 = CARTESIAN_POINT ( 'NONE',  ( -117.5170265704868200, -24.51314013834316086, 0.6176544820404215042 ) ) ;
#68181 = CARTESIAN_POINT ( 'NONE',  ( -99.87501341000351829, -25.12215651587715115, 6.992709577391502229 ) ) ;
#68182 = CARTESIAN_POINT ( 'NONE',  ( -5.167225684058948332, 21.16526716281445530, -1.500000000000002220 ) ) ;
#68183 = CARTESIAN_POINT ( 'NONE',  ( -114.5228709571500616, -23.47596703998600631, 11.44779298504228038 ) ) ;
#68184 = CARTESIAN_POINT ( 'NONE',  ( -76.64296881555020491, -23.73791477778911840, 11.05961554403170766 ) ) ;
#68185 = CARTESIAN_POINT ( 'NONE',  ( -79.78390267227787547, -25.17112743842814027, 6.874869416038779768 ) ) ;
#68186 = CARTESIAN_POINT ( 'NONE',  ( -1.994712787082457472, 21.64621699974126656, -1.500000000000002220 ) ) ;
#68187 = CARTESIAN_POINT ( 'NONE',  ( -0.4909855769230799249, -6.376774720514410077, 19.14743589743590491 ) ) ;
#68189 = ORIENTED_EDGE ( 'NONE', *, *, #20181, .T. ) ;
#68188 = CARTESIAN_POINT ( 'NONE',  ( 9.556255610625576935, 20.19728179944524271, 11.49999999999999645 ) ) ;
#68190 = CARTESIAN_POINT ( 'NONE',  ( -116.5895376238167387, -23.47593901973091235, -1.443836447538997536 ) ) ;
#68191 = CARTESIAN_POINT ( 'NONE',  ( -25.92875734969025814, 3.316774720514426456, 0.7300228001186309656 ) ) ;
#68192 = CARTESIAN_POINT ( 'NONE',  ( -31.52287095715006160, -24.64898659630367206, 1.056161002820817485 ) ) ;
#68193 = ORIENTED_EDGE ( 'NONE', *, *, #78882, .F. ) ;
#68194 = ORIENTED_EDGE ( 'NONE', *, *, #48287, .F. ) ;
#68195 = VERTEX_POINT ( 'NONE', #57295 ) ;
#68196 = DIRECTION ( 'NONE',  ( 0.000000000000000000, 0.000000000000000000, -1.000000000000000000 ) ) ;
#68197 = CARTESIAN_POINT ( 'NONE',  ( -9.361133326760958440, -19.03884994183470880, 11.49999999999998934 ) ) ;
#68198 = CARTESIAN_POINT ( 'NONE',  ( 11.05000000000000249, 0.000000000000000000, 0.000000000000000000 ) ) ;
#68199 = CARTESIAN_POINT ( 'NONE',  ( -95.62287095715004170, -23.84081130438200802, 10.88220057463249013 ) ) ;
#68200 = B_SPLINE_CURVE_WITH_KNOTS ( 'NONE', 3,
 ( #35246, #66216, #88531, #57594, #49483, #97136 ),
 .UNSPECIFIED., .F., .F.,
 ( 4, 2, 4 ),
 ( 6.391158118958419274E-06, 0.001387004593080778557, 0.002767618028042598960 ),
 .UNSPECIFIED. ) ;
#68201 = DIRECTION ( 'NONE',  ( -0.9975640502598243087, 0.06975647374412548285, 0.000000000000000000 ) ) ;
#68202 = CARTESIAN_POINT ( 'NONE',  ( 31.84105487026594261, 5.152774720514426754, -11.95870468328485003 ) ) ;
#68203 = EDGE_CURVE ( 'NONE', #31070, #3112, #46319, .T. ) ;
#68204 = CARTESIAN_POINT ( 'NONE',  ( -18.23339674026497903, -6.527145932826366348, 11.49999999999998934 ) ) ;
#68205 = LINE ( 'NONE', #12405, #39207 ) ;
#68206 = ORIENTED_EDGE ( 'NONE', *, *, #7723, .T. ) ;
#68207 = CARTESIAN_POINT ( 'NONE',  ( -19.39930850525863804, 0.8904154686948315689, 11.49999999999999645 ) ) ;
#68208 = CYLINDRICAL_SURFACE ( 'NONE', #61734, 0.8160000000000007248 ) ;
#68209 = EDGE_CURVE ( 'NONE', #77123, #86024, #42061, .T. ) ;
#68210 = ORIENTED_EDGE ( 'NONE', *, *, #72583, .F. ) ;
#68211 = LINE ( 'NONE', #51990, #13472 ) ;
#68212 = CARTESIAN_POINT ( 'NONE',  ( 2.790451961050095520, -6.376774720514408301, 18.85195250256714417 ) ) ;
#68213 = EDGE_CURVE ( 'NONE', #65697, #33349, #34434, .T. ) ;
#68214 = DIRECTION ( 'NONE',  ( 1.000000000000000000, 0.000000000000000000, 0.000000000000000000 ) ) ;
#68215 = ADVANCED_FACE ( 'NONE', ( #86713 ), #48168, .F. ) ;
#68216 = CARTESIAN_POINT ( 'NONE',  ( 8.499999999999989342, 18.74999999999999645, 2.100000000000000089 ) ) ;
#68217 = CARTESIAN_POINT ( 'NONE',  ( 0.6594449095415070294, 19.62168050102039629, 11.49999999999998934 ) ) ;
#68218 = CARTESIAN_POINT ( 'NONE',  ( -33.62287095715005592, -29.50250243563736774, 8.947779886222150481 ) ) ;
#68220 = EDGE_CURVE ( 'NONE', #26340, #95272, #58281, .T. ) ;
#68219 = ORIENTED_EDGE ( 'NONE', *, *, #89960, .T. ) ;
#68221 = CARTESIAN_POINT ( 'NONE',  ( 5.689979955356517571, -20.79666814084963278, 11.49999999999998934 ) ) ;
#68222 = CARTESIAN_POINT ( 'NONE',  ( -33.58672562287462426, -24.35071581493542325, 9.817618358456039473 ) ) ;
#68223 = CARTESIAN_POINT ( 'NONE',  ( -116.5228709571501042, -23.47593901973090524, -1.443836447538996426 ) ) ;
#68224 = CARTESIAN_POINT ( 'NONE',  ( -62.62287095715004881, -24.64965695001468404, 8.947790433994185832 ) ) ;
#68225 = CARTESIAN_POINT ( 'NONE',  ( -99.59031406714542811, -25.27473316629503941, 3.731155320732701952 ) ) ;
#68226 = CARTESIAN_POINT ( 'NONE',  ( -14.58522200957802184, -17.87834940746265389, -1.500000000000002220 ) ) ;
#68227 = APPROVAL_ROLE ( '' ) ;
#68228 = CARTESIAN_POINT ( 'NONE',  ( -93.51534127454544887, -23.96119346886881019, -0.6495511937832080251 ) ) ;
#68229 = CARTESIAN_POINT ( 'NONE',  ( -51.30640140532707960, -25.30285855287542773, 4.744951912546983230 ) ) ;
#68230 = CARTESIAN_POINT ( 'NONE',  ( 14.24339680280927567, 14.23919408161895284, 11.49999999999999645 ) ) ;
#68231 = CARTESIAN_POINT ( 'NONE',  ( -45.62287095715006302, -24.62285846362216191, 9.038163152653527987 ) ) ;
#68232 = DIRECTION ( 'NONE',  ( -0.000000000000000000, 0.000000000000000000, -1.000000000000000000 ) ) ;
#68233 = CARTESIAN_POINT ( 'NONE',  ( 5.949073730962466833, -6.475225279485573360, -27.94053387008862188 ) ) ;
#68234 = PLANE ( 'NONE',  #79652 ) ;
#68235 = CARTESIAN_POINT ( 'NONE',  ( 13.10664265030973930, 5.965225279485574461, -28.64597719988137570 ) ) ;
#68237 = EDGE_CURVE ( 'NONE', #1158, #92467, #95990, .T. ) ;
#68236 = CARTESIAN_POINT ( 'NONE',  ( 0.1862606309321278575, -19.90735222434816976, -1.500000000000002220 ) ) ;
#68238 = CARTESIAN_POINT ( 'NONE',  ( -68.62287095715005592, -23.47593901973091235, -1.443836447539006196 ) ) ;
#68239 = CARTESIAN_POINT ( 'NONE',  ( -11.78406182805296254, 15.88391379356440503, -1.500000000000002220 ) ) ;
#68240 = CARTESIAN_POINT ( 'NONE',  ( -126.5893510134409325, -24.51419770103158413, 9.386484678747162747 ) ) ;
#68241 = VECTOR ( 'NONE', #62116, 1000.000000000000114 ) ;
#68242 = CARTESIAN_POINT ( 'NONE',  ( -1.044871794871793602, -6.376774720514418959, 20.44941907051282115 ) ) ;
#68243 = CARTESIAN_POINT ( 'NONE',  ( -37.52287095715008292, -23.73907113217657994, -1.053371485781499306 ) ) ;
#68244 = CARTESIAN_POINT ( 'NONE',  ( 16.32338804990218151, -12.73490195939593406, 11.49999999999999645 ) ) ;
#68245 = LINE ( 'NONE', #75341, #35404 ) ;
#68246 = EDGE_CURVE ( 'NONE', #24236, #54115, #21187, .T. ) ;
#68247 = CARTESIAN_POINT ( 'NONE',  ( -108.5228709571500616, -29.50247984919015209, -1.443849546365048253 ) ) ;
#68248 = CARTESIAN_POINT ( 'NONE',  ( -35.58953762381672448, -23.47596703998600276, 11.44779298504227505 ) ) ;
#68249 = CARTESIAN_POINT ( 'NONE',  ( 7.533951754900199305, 21.46025436219600024, 11.49999999999999645 ) ) ;
#68250 = ORIENTED_EDGE ( 'NONE', *, *, #76942, .T. ) ;
#68251 = CARTESIAN_POINT ( 'NONE',  ( -91.62287095715004170, -23.94994826722565762, -0.6494450866342749151 ) ) ;
#68252 = EDGE_CURVE ( 'NONE', #51004, #72503, #80358, .T. ) ;
#68253 = CARTESIAN_POINT ( 'NONE',  ( -28.47875734969026240, -6.475225279485573360, 26.43402280011862615 ) ) ;
#68254 = CARTESIAN_POINT ( 'NONE',  ( 13.23653054071972512, 15.24542462990338088, 11.49999999999998934 ) ) ;
#68255 = CARTESIAN_POINT ( 'NONE',  ( 9.071512145086501278, 0.000000000000000000, -3.687490859131162591 ) ) ;
#68256 = ADVANCED_FACE ( 'NONE', ( #12077 ), #41557, .F. ) ;
#68257 = CARTESIAN_POINT ( 'NONE',  ( -41.46446907970767626, -25.28258282913159860, 4.252216095719075994 ) ) ;
#68258 = EDGE_LOOP ( 'NONE', ( #2773, #68595, #29871, #62541 ) ) ;
#68259 = ADVANCED_FACE ( 'NONE', ( #20688 ), #28810, .T. ) ;
#68260 = ORIENTED_EDGE ( 'NONE', *, *, #36053, .T. ) ;
#68261 = DIRECTION ( 'NONE',  ( 0.000000000000000000, 2.173523156925980399E-06, -0.9999999999976378895 ) ) ;
#68262 = CARTESIAN_POINT ( 'NONE',  ( 15.42672287639063100, 16.92133821996916865, -1.500000000000002220 ) ) ;
#68264 = ADVANCED_FACE ( 'NONE', ( #73492 ), #89720, .T. ) ;
#68263 = CARTESIAN_POINT ( 'NONE',  ( -111.3776484685884185, -25.28710546256126079, 4.332404433089555695 ) ) ;
#68265 = CARTESIAN_POINT ( 'NONE',  ( 20.55956107658784404, -6.795330137259728787, -1.500000000000002220 ) ) ;
#68266 = DIRECTION ( 'NONE',  ( 1.000000000000000000, 3.773278334444167608E-23, 8.201307833595939069E-29 ) ) ;
#68267 = CARTESIAN_POINT ( 'NONE',  ( -127.5892766125946451, -24.66019654487200441, 8.947790411086106843 ) ) ;
#68268 = CARTESIAN_POINT ( 'NONE',  ( 17.92008016455634589, 10.74458801173053324, 11.49999999999999645 ) ) ;
#68269 = VERTEX_POINT ( 'NONE', #81102 ) ;
#68270 = PLANE ( 'NONE',  #99949 ) ;
#68271 = CARTESIAN_POINT ( 'NONE',  ( -15.01370250125036421, 16.05796621403891677, 11.49999999999998934 ) ) ;
#68272 = CARTESIAN_POINT ( 'NONE',  ( -105.5461398891562936, -25.00182538069147142, 7.747789668545045139 ) ) ;
#68273 = CARTESIAN_POINT ( 'NONE',  ( -40.50110916354886825, -25.29087034907446707, 2.834725585562781092 ) ) ;
#68274 = ORIENTED_EDGE ( 'NONE', *, *, #100279, .T. ) ;
#68275 = DIRECTION ( 'NONE',  ( 3.773278334444166432E-23, -1.000000000000000000, 0.000000000000000000 ) ) ;
#68276 = CARTESIAN_POINT ( 'NONE',  ( 22.74089357256066535, 1.682774720514426114, -19.20396252371061863 ) ) ;
#68277 = ORIENTED_EDGE ( 'NONE', *, *, #84330, .F. ) ;
#68278 = CARTESIAN_POINT ( 'NONE',  ( -72.63498091499847931, -24.15620529776628089, 10.23563542870660825 ) ) ;
#68279 = VERTEX_POINT ( 'NONE', #5474 ) ;
#68280 = B_SPLINE_CURVE_WITH_KNOTS ( 'NONE', 3,
 ( #57517, #87952, #71228, #17936, #11325, #95057 ),
 .UNSPECIFIED., .F., .F.,
 ( 4, 2, 4 ),
 ( 0.000000000000000000, 0.001381645775336347781, 0.002763291550672695562 ),
 .UNSPECIFIED. ) ;
#68281 = ORIENTED_EDGE ( 'NONE', *, *, #47680, .F. ) ;
#68282 = LINE ( 'NONE', #61183, #30706 ) ;
#68283 = DIRECTION ( 'NONE',  ( -3.773278334453079030E-23, 0.9999999999976377785, 2.173523156925979128E-06 ) ) ;
#68284 = CARTESIAN_POINT ( 'NONE',  ( -57.64982222934394684, -23.73766607897670866, -1.055555164236458454 ) ) ;
#68285 = CARTESIAN_POINT ( 'NONE',  ( -12.12210191164509965, 16.44476101713275185, -1.500000000000002220 ) ) ;
#68286 = ORIENTED_EDGE ( 'NONE', *, *, #34481, .T. ) ;
#68287 = CARTESIAN_POINT ( 'NONE',  ( -2.285970405126252825, -5.876774720514407413, 19.14905311829361167 ) ) ;
#68288 = CARTESIAN_POINT ( 'NONE',  ( -92.52287095715007581, -24.51387760970725083, 9.387446482453409402 ) ) ;
#68289 = DIRECTION ( 'NONE',  ( 0.000000000000000000, 0.000000000000000000, 1.000000000000000000 ) ) ;
#68290 = CARTESIAN_POINT ( 'NONE',  ( -8.160000000000000142, 9.789768006247301813, -0.8564937190954607926 ) ) ;
#68291 = VERTEX_POINT ( 'NONE', #11583 ) ;
#68292 = CARTESIAN_POINT ( 'NONE',  ( -30.47287095715007510, -23.47596699454220470, 11.42688508591989560 ) ) ;
#68293 = CARTESIAN_POINT ( 'NONE',  ( -29.54485641382474626, -24.63645763816374412, 6.867484160806894167 ) ) ;
#68294 = CARTESIAN_POINT ( 'NONE',  ( 13.57807927624399902, 15.74560944506941951, -1.500000000000002220 ) ) ;
#68295 = VECTOR ( 'NONE', #82076, 1000.000000000000000 ) ;
#68296 = ORIENTED_EDGE ( 'NONE', *, *, #28043, .F. ) ;
#68297 = B_SPLINE_CURVE_WITH_KNOTS ( 'NONE', 3,
 ( #71323, #64740, #19019, #57110 ),
 .UNSPECIFIED., .F., .F.,
 ( 4, 4 ),
 ( 0.000000000000000000, 9.999999999998897304E-05 ),
 .UNSPECIFIED. ) ;
#68299 = ORIENTED_EDGE ( 'NONE', *, *, #54590, .F. ) ;
#68298 = CARTESIAN_POINT ( 'NONE',  ( -54.62287095715004170, -23.94994826722515668, -0.6494450866351753060 ) ) ;
#68300 = CARTESIAN_POINT ( 'NONE',  ( -89.81226385320383088, -25.23397913219354649, 6.409327625488847602 ) ) ;
#68301 = ORIENTED_EDGE ( 'NONE', *, *, #55778, .T. ) ;
#68302 = EDGE_LOOP ( 'NONE', ( #51657, #6740, #54986, #38441 ) ) ;
#68303 = CARTESIAN_POINT ( 'NONE',  ( 1.600000000000000755, 0.000000000000000000, 0.000000000000000000 ) ) ;
#68304 = DIRECTION ( 'NONE',  ( -3.773278334453079030E-23, 0.9999999999976377785, 2.173523156925979128E-06 ) ) ;
#68305 = FACE_OUTER_BOUND ( 'NONE', #38571, .T. ) ;
#68306 = DIRECTION ( 'NONE',  ( -3.773278334453079030E-23, 0.9999999999976377785, 2.173523156925979128E-06 ) ) ;
#68308 = CARTESIAN_POINT ( 'NONE',  ( -92.51226550044627572, -24.15620529776627734, 10.23563542870659937 ) ) ;
#68307 = B_SPLINE_CURVE_WITH_KNOTS ( 'NONE', 3,
 ( #71685, #32105, #33114, #2678, #23989, #95010 ),
 .UNSPECIFIED., .F., .F.,
 ( 4, 2, 4 ),
 ( 0.000000000000000000, 0.001380764517854767568, 0.002761529035709535135 ),
 .UNSPECIFIED. ) ;
#68309 = LINE ( 'NONE', #99240, #30294 ) ;
#68311 = ORIENTED_EDGE ( 'NONE', *, *, #68744, .F. ) ;
#68310 = CARTESIAN_POINT ( 'NONE',  ( 17.13038851031509680, -14.05419017248541813, 11.49999999999999645 ) ) ;
#68312 = CARTESIAN_POINT ( 'NONE',  ( -108.5505322218205464, -24.51314013834316086, 0.6176544820404235026 ) ) ;
#68313 = CARTESIAN_POINT ( 'NONE',  ( -18.78231125015805958, 12.62931641965373153, -1.500000000000002220 ) ) ;
#68315 = ORIENTED_EDGE ( 'NONE', *, *, #14124, .T. ) ;
#68314 = CARTESIAN_POINT ( 'NONE',  ( -87.55620429048337883, -23.47593901973091235, -1.443836447539002865 ) ) ;
#68316 = CIRCLE ( 'NONE', #82923, 130.7884398600581335 ) ;
#68317 = VERTEX_POINT ( 'NONE', #36421 ) ;
#68318 = APPROVAL_PERSON_ORGANIZATION ( #91419, #83531, #77186 ) ;
#68319 = CARTESIAN_POINT ( 'NONE',  ( -10.13340495651384288, -4.304508339349029988, 30.35717091805029355 ) ) ;
#68320 = EDGE_CURVE ( 'NONE', #22811, #80400, #27317, .T. ) ;
#68321 = CARTESIAN_POINT ( 'NONE',  ( 0.3675393366473880818, 20.13074986235200470, 11.49999999999998934 ) ) ;
#68322 = FACE_OUTER_BOUND ( 'NONE', #78365, .T. ) ;
#68323 = VERTEX_POINT ( 'NONE', #4976 ) ;
#68324 = EDGE_CURVE ( 'NONE', #54335, #70415, #44737, .T. ) ;
#68325 = CARTESIAN_POINT ( 'NONE',  ( -103.5562042904833930, -24.64965694238575011, 8.947790433994194714 ) ) ;
#68326 = CARTESIAN_POINT ( 'NONE',  ( -22.22805510923732086, 2.117028069546627922, -1.500000000000002220 ) ) ;
#68327 = EDGE_CURVE ( 'NONE', #654, #56438, #5834, .T. ) ;
#68328 = VERTEX_POINT ( 'NONE', #13573 ) ;
#68329 = ORIENTED_EDGE ( 'NONE', *, *, #59066, .T. ) ;
#68330 = CARTESIAN_POINT ( 'NONE',  ( -76.52287095715007581, -24.64965694238408034, 8.947790433994198267 ) ) ;
#68331 = CARTESIAN_POINT ( 'NONE',  ( -80.85315749703953259, -25.04053079579781382, 7.527282393074037792 ) ) ;
#68332 = CARTESIAN_POINT ( 'NONE',  ( 9.071512145086501278, 0.000000000000000000, -3.687490859131163479 ) ) ;
#68333 = EDGE_CURVE ( 'NONE', #47870, #6498, #93643, .T. ) ;
#68334 = CARTESIAN_POINT ( 'NONE',  ( -102.5562042904834072, -23.47593901973091235, -1.443836447539001089 ) ) ;
#68335 = ADVANCED_FACE ( 'NONE', ( #98813 ), #23177, .T. ) ;
#68336 = CARTESIAN_POINT ( 'NONE',  ( 0.000000000000000000, -5.356774720514425603, 6.000000000000000888 ) ) ;
#68337 = CARTESIAN_POINT ( 'NONE',  ( 6.866622826037362515, -18.30913693658520103, 11.49999999999998934 ) ) ;
#68338 = PLANE ( 'NONE',  #74983 ) ;
#68339 = EDGE_CURVE ( 'NONE', #50965, #26504, #70095, .T. ) ;
#68340 = CARTESIAN_POINT ( 'NONE',  ( -2.231587876719630437, -21.34735720706076378, 11.49999999999998934 ) ) ;
#68341 = CARTESIAN_POINT ( 'NONE',  ( -2.750773227259631692, -5.876774720514411854, 19.84584863393302001 ) ) ;
#68342 = CARTESIAN_POINT ( 'NONE',  ( -6.660000000000001030, -9.074990544709798712, -0.7360493640965781736 ) ) ;
#68343 = CARTESIAN_POINT ( 'NONE',  ( -115.5562042904833930, -24.99132157543166954, 2.256160258750668834 ) ) ;
#68344 = CARTESIAN_POINT ( 'NONE',  ( -7.509321099650855480, 21.62252279970214985, -1.500000000000002220 ) ) ;
#68345 = AXIS2_PLACEMENT_3D ( 'NONE', #35986, #51219, #66959 ) ;
#68346 = COORDINATED_UNIVERSAL_TIME_OFFSET ( 0, 0, .AHEAD. ) ;
#68347 = CARTESIAN_POINT ( 'NONE',  ( -106.5159469206628842, -24.15620529776629510, 10.23563542870659582 ) ) ;
#68348 = PLANE ( 'NONE',  #3688 ) ;
#68349 = CARTESIAN_POINT ( 'NONE',  ( -0.003041637939312698616, 19.98351707251910980, 11.49999999999999645 ) ) ;
#68350 = CARTESIAN_POINT ( 'NONE',  ( -50.52287095715006870, -24.52232992886363405, 0.6492154411905944889 ) ) ;
#68351 = CARTESIAN_POINT ( 'NONE',  ( -74.64913626771259203, -23.48786465467241058, 11.44779295918254824 ) ) ;
#68352 = CARTESIAN_POINT ( 'NONE',  ( 21.57151214508649772, -9.529487854913506695, 0.000000000000000000 ) ) ;
#68353 = ORIENTED_EDGE ( 'NONE', *, *, #63224, .T. ) ;
#68354 = CARTESIAN_POINT ( 'NONE',  ( -89.52287095715006160, -24.64898659630528854, 1.056161002820827921 ) ) ;
#68355 = EDGE_CURVE ( 'NONE', #55838, #7066, #8471, .T. ) ;
#68356 = CARTESIAN_POINT ( 'NONE',  ( -0.02075734969026423599, -3.316774720514426456, -29.05397719988137339 ) ) ;
#68357 = CARTESIAN_POINT ( 'NONE',  ( 6.244050601037331560, 20.82503750550150912, 11.49999999999998934 ) ) ;
#68358 = CARTESIAN_POINT ( 'NONE',  ( -4.886549725601808447, -6.376774720514410077, 19.15251819062245175 ) ) ;
#68359 = CARTESIAN_POINT ( 'NONE',  ( 17.47348308817029405, 8.859467055162037141, -1.500000000000002220 ) ) ;
#68360 = CARTESIAN_POINT ( 'NONE',  ( -99.29687923781919778, -25.26138073939643292, 6.149712181314777482 ) ) ;
#68361 = EDGE_CURVE ( 'NONE', #36016, #45083, #35061, .T. ) ;
#68362 = VERTEX_POINT ( 'NONE', #31304 ) ;
#68363 = APPROVAL_STATUS ( 'not_yet_approved' ) ;
#68364 = CARTESIAN_POINT ( 'NONE',  ( -108.8968792378192632, -25.08859304705472937, 7.294522420277893993 ) ) ;
#68365 = CARTESIAN_POINT ( 'NONE',  ( 3.509873074917118085, -5.965225279485572685, 29.15869884040363758 ) ) ;
#68366 = CARTESIAN_POINT ( 'NONE',  ( 20.06376955418885899, 4.186446014007643157, 11.49999999999999645 ) ) ;
#68367 = CARTESIAN_POINT ( 'NONE',  ( -59.52287095715006160, -23.48786465467241769, 11.44779295918254824 ) ) ;
#68368 = CIRCLE ( 'NONE', #87848, 1.699999999999996625 ) ;
#68369 = ADVANCED_FACE ( 'NONE', ( #61278 ), #76966, .T. ) ;
#68370 = CARTESIAN_POINT ( 'NONE',  ( -2.499999999999993339, 19.99999999999999645, 2.100000000000000089 ) ) ;
#68371 = ORIENTED_EDGE ( 'NONE', *, *, #15865, .F. ) ;
#68372 = CARTESIAN_POINT ( 'NONE',  ( 31.13513474936814163, -4.540774720514427543, 3.331262582247520143 ) ) ;
#68373 = LINE ( 'NONE', #38914, #80214 ) ;
#68374 = CARTESIAN_POINT ( 'NONE',  ( -101.5562042904833788, -23.48783264082478439, -1.443836473390061936 ) ) ;
#68375 = CARTESIAN_POINT ( 'NONE',  ( -123.5228709571499763, -23.95044443724992789, 10.65354141964648527 ) ) ;
#68376 = ORGANIZATION ( 'NAUO-ORG12', 'UNSPECIFIED', 'UNSPECIFIED' ) ;
#68377 = CARTESIAN_POINT ( 'NONE',  ( -42.62287095715004170, -24.33927499327853994, 9.819080762295818943 ) ) ;
#68378 = EDGE_CURVE ( 'NONE', #79832, #60562, #52650, .T. ) ;
#68379 = CIRCLE ( 'NONE', #8474, 4.299999999999999822 ) ;
#68380 = CARTESIAN_POINT ( 'NONE',  ( 23.03040035405544472, 1.057182387018521963, 11.49999999999999645 ) ) ;
#68381 = CARTESIAN_POINT ( 'NONE',  ( 12.37853024107498534, -19.16169124346054176, 11.49999999999998934 ) ) ;
#68382 = CARTESIAN_POINT ( 'NONE',  ( -70.27422298781921484, -25.30458796900497376, 4.851635164322918747 ) ) ;
#68383 = CARTESIAN_POINT ( 'NONE',  ( -5.837039262820512775, -6.376774720514413630, 19.76512419871795245 ) ) ;
#68384 = LINE ( 'NONE', #29811, #51722 ) ;
#68385 = SECURITY_CLASSIFICATION ( '', '', #74826 ) ;
#68386 = CARTESIAN_POINT ( 'NONE',  ( 0.000000000000000000, 5.356774720514425603, 0.000000000000000000 ) ) ;
#68387 = CARTESIAN_POINT ( 'NONE',  ( -110.5169900288274647, -24.15503026093914229, -0.2815557561904443729 ) ) ;
#68388 = ADVANCED_FACE ( 'NONE', ( #30301 ), #71906, .T. ) ;
#68389 = CARTESIAN_POINT ( 'NONE',  ( -12.72821696145241255, -17.84489267850806726, 11.49999999999998934 ) ) ;
#68390 = CARTESIAN_POINT ( 'NONE',  ( -87.58953762381671027, -24.65952944569304961, 1.056160979905701458 ) ) ;
#68391 = CARTESIAN_POINT ( 'NONE',  ( -87.62358879123520694, -24.66019654487200441, 8.947790411086112172 ) ) ;
#68392 = CARTESIAN_POINT ( 'NONE',  ( -29.49875734969026198, 5.965225279485572685, 7.870022800118625206 ) ) ;
#68393 = CARTESIAN_POINT ( 'NONE',  ( -78.63379020606802783, -24.15543982623907127, -0.2315651400026641771 ) ) ;
#68394 = FACE_OUTER_BOUND ( 'NONE', #89836, .T. ) ;
#68395 = CARTESIAN_POINT ( 'NONE',  ( -122.6228709571500133, -24.51387760970724017, 9.387446482453405849 ) ) ;
#68396 = ORIENTED_EDGE ( 'NONE', *, *, #32985, .T. ) ;
#68397 = CARTESIAN_POINT ( 'NONE',  ( 0.3735783541106268979, -20.45636175344465713, -1.500000000000002220 ) ) ;
#68398 = VERTEX_POINT ( 'NONE', #15573 ) ;
#68399 = VERTEX_POINT ( 'NONE', #29805 ) ;
#68400 = ORIENTED_EDGE ( 'NONE', *, *, #99248, .T. ) ;
#68401 = ORIENTED_EDGE ( 'NONE', *, *, #80061, .F. ) ;
#68402 = CARTESIAN_POINT ( 'NONE',  ( 22.88022663504679599, 2.825535151426334934, 11.49999999999998934 ) ) ;
#68403 = CARTESIAN_POINT ( 'NONE',  ( -61.57930669521469724, -24.65952944569304961, 1.056160979905699682 ) ) ;
#68404 = CARTESIAN_POINT ( 'NONE',  ( 14.48468284575590204, 14.13777120147990729, -1.500000000000002220 ) ) ;
#68405 = EDGE_LOOP ( 'NONE', ( #99432, #61597, #45693, #61296 ) ) ;
#68406 = CARTESIAN_POINT ( 'NONE',  ( -29.26978116671819663, -25.09101794427064291, 3.118813907533751983 ) ) ;
#68407 = CARTESIAN_POINT ( 'NONE',  ( -41.86995616089614458, -25.28979658489737048, 4.210709715701590028 ) ) ;
#68408 = CARTESIAN_POINT ( 'NONE',  ( -49.62287095715005592, -29.50248528299804818, 1.056150453629033370 ) ) ;
#68409 = FACE_OUTER_BOUND ( 'NONE', #2171, .T. ) ;
#68411 = ORIENTED_EDGE ( 'NONE', *, *, #46789, .T. ) ;
#68410 = CARTESIAN_POINT ( 'NONE',  ( -9.048234560742015375, 19.43086790383670603, 11.49999999999999645 ) ) ;
#68412 = DIRECTION ( 'NONE',  ( 0.000000000000000000, 0.9999999999976377785, 2.173523156925979128E-06 ) ) ;
#68413 = CARTESIAN_POINT ( 'NONE',  ( -34.62287095715005592, -23.72747288104469732, -1.053458166803227902 ) ) ;
#68414 = EDGE_LOOP ( 'NONE', ( #29231, #72677, #12399, #70169 ) ) ;
#68415 = CARTESIAN_POINT ( 'NONE',  ( -20.39401028033356766, -3.670942005906183692, 11.49999999999998934 ) ) ;
#68417 = ORIENTED_EDGE ( 'NONE', *, *, #39707, .T. ) ;
#68416 = CARTESIAN_POINT ( 'NONE',  ( -28.98875734969026396, -5.965225279485572685, -0.08597719988137648983 ) ) ;
#68418 = VECTOR ( 'NONE', #85660, 1000.000000000000000 ) ;
#68419 = B_SPLINE_SURFACE_WITH_KNOTS ( 'NONE', 3, 3, ( 
 ( #40015, #10066, #55759, #1968 ),
 ( #55258, #41027, #32910, #62880 ),
 ( #46641, #79068, #54756, #16172 ),
 ( #93288, #62362, #25789, #47641 ),
 ( #71980, #15674, #16671, #78557 ),
 ( #23783, #95304, #85691, #77559 ),
 ( #69963, #24779, #86686, #32407 ) ),
 .UNSPECIFIED., .F., .F., .F.,
 ( 4, 3, 4 ),
 ( 4, 4 ),
 ( 0.7945040050992232539, 0.8970133687736493444, 0.9995227324480754350 ),
 ( 0.06951166112253108487, 0.07055647687300854731 ),
 .UNSPECIFIED. ) ;
#68421 = CARTESIAN_POINT ( 'NONE',  ( -91.52287095715010423, -24.35013146730204525, 9.818937971375097717 ) ) ;
#68420 = B_SPLINE_CURVE_WITH_KNOTS ( 'NONE', 3,
 ( #59708, #91135, #52086, #74903 ),
 .UNSPECIFIED., .F., .F.,
 ( 4, 4 ),
 ( 0.000000000000000000, 9.999999999999592548E-05 ),
 .UNSPECIFIED. ) ;
#68422 = ORIENTED_EDGE ( 'NONE', *, *, #7526, .T. ) ;
#68423 = CARTESIAN_POINT ( 'NONE',  ( 4.531089049250198286, -6.376774720514404748, 18.46391971337801508 ) ) ;
#68424 = ORIENTED_EDGE ( 'NONE', *, *, #7544, .F. ) ;
#68425 = CARTESIAN_POINT ( 'NONE',  ( 14.12621959167996977, 16.79361087625908056, 11.49999999999999645 ) ) ;
#68426 = CARTESIAN_POINT ( 'NONE',  ( -37.55288945954268343, -23.96169478059712432, 10.65365249895718591 ) ) ;
#68427 = CARTESIAN_POINT ( 'NONE',  ( 11.36372850657041589, -19.49111573544105624, 11.49999999999998934 ) ) ;
#68428 = CARTESIAN_POINT ( 'NONE',  ( -20.02981537788295441, -6.213780249082809348, 11.49999999999998934 ) ) ;
#68429 = CARTESIAN_POINT ( 'NONE',  ( -109.4421867512570401, -25.31228852508138516, 5.310510576710047559 ) ) ;
#68430 = CARTESIAN_POINT ( 'NONE',  ( 5.696197030082937651, -6.376774720514422512, 21.05387829558662816 ) ) ;
#68431 = VERTEX_POINT ( 'NONE', #60773 ) ;
#68432 = AXIS2_PLACEMENT_3D ( 'NONE', #92312, #20795, #22286 ) ;
#68433 = ORIENTED_EDGE ( 'NONE', *, *, #88185, .T. ) ;
#68434 = VERTEX_POINT ( 'NONE', #77464 ) ;
#68435 = VECTOR ( 'NONE', #68745, 1000.000000000000000 ) ;
#68436 = CARTESIAN_POINT ( 'NONE',  ( -66.62727618262151452, -24.51314013834316441, 0.6176544820404136216 ) ) ;
#68437 = CARTESIAN_POINT ( 'NONE',  ( -2.508422780830330989, 21.39056295969660582, -1.500000000000002220 ) ) ;
#68438 = LINE ( 'NONE', #98372, #58641 ) ;
#68439 = ORIENTED_EDGE ( 'NONE', *, *, #52057, .T. ) ;
#68440 = CARTESIAN_POINT ( 'NONE',  ( -20.28541985502614509, -5.886007371444655689, -1.500000000000002220 ) ) ;
#68441 = LINE ( 'NONE', #53727, #78968 ) ;
#68442 = ADVANCED_FACE ( 'NONE', ( #7965 ), #38919, .T. ) ;
#68443 = CARTESIAN_POINT ( 'NONE',  ( -65.05438548721848235, 6.376774720514426953, 0.7300228001186309656 ) ) ;
#68444 = CARTESIAN_POINT ( 'NONE',  ( -0.02075734969026423599, -5.356774720514425603, -0.08597719988137648983 ) ) ;
#68445 = CARTESIAN_POINT ( 'NONE',  ( -99.29687923781919778, -25.25133594952260552, 6.149712203147405631 ) ) ;
#68446 = CARTESIAN_POINT ( 'NONE',  ( -0.7614568544629641833, -5.876774720514408301, 19.18727597066020962 ) ) ;
#68447 = CARTESIAN_POINT ( 'NONE',  ( 4.265775719338400052, 21.77767432286298543, -1.500000000000002220 ) ) ;
#68448 = EDGE_CURVE ( 'NONE', #11793, #29710, #8968, .T. ) ;
#68449 = CARTESIAN_POINT ( 'NONE',  ( -71.50229426790137666, -24.34968618360933945, 0.1864209137778822800 ) ) ;
#68450 = ADVANCED_FACE ( 'NONE', ( #26197 ), #40428, .F. ) ;
#68451 = ORIENTED_EDGE ( 'NONE', *, *, #82074, .F. ) ;
#68452 = CARTESIAN_POINT ( 'NONE',  ( -108.9857387129618758, -25.29479647189234015, 4.484512479850331523 ) ) ;
#68453 = FACE_OUTER_BOUND ( 'NONE', #98628, .T. ) ;
#68454 = CARTESIAN_POINT ( 'NONE',  ( -41.86995616089613748, -25.31624451996179914, 4.210709658216391205 ) ) ;
#68455 = ADVANCED_FACE ( 'NONE', ( #63281 ), #88107, .F. ) ;
#68456 = CARTESIAN_POINT ( 'NONE',  ( 0.1553305729023591875, -1.423459158329792640, 2.407412430484044816E-32 ) ) ;
#68457 = AXIS2_PLACEMENT_3D ( 'NONE', #53992, #84920, #15404 ) ;
#68458 = CARTESIAN_POINT ( 'NONE',  ( -15.63568348323273227, -11.59263941501104966, 11.49999999999998934 ) ) ;
#68459 = LOCAL_TIME ( 0, 54, 15.00000000000000000, #90930 ) ;
#68460 = CARTESIAN_POINT ( 'NONE',  ( -15.06583839362908961, -15.15408912208086534, 11.49999999999998934 ) ) ;
#68461 = CARTESIAN_POINT ( 'NONE',  ( -62.51546559041052120, -23.73766607897669445, -1.055555164236454901 ) ) ;
#68462 = CARTESIAN_POINT ( 'NONE',  ( -90.25664208330698557, -25.26877915520014639, 5.947789088310639904 ) ) ;
#68463 = CARTESIAN_POINT ( 'NONE',  ( -79.62287095715007013, -23.96127896941631619, -0.6493128931037847051 ) ) ;
#68464 = LINE ( 'NONE', #99399, #42553 ) ;
#68465 = CARTESIAN_POINT ( 'NONE',  ( 19.70651319644445465, -11.07993823016455792, -1.500000000000002220 ) ) ;
#68466 = B_SPLINE_CURVE_WITH_KNOTS ( 'NONE', 3,
 ( #38942, #24217, #382, #31330, #62299, #54683, #85614, #55192, #16103, #47072, #70400, #78494, #11001, #27231 ),
 .UNSPECIFIED., .F., .F.,
 ( 4, 2, 2, 2, 2, 2, 4 ),
 ( 0.000000000000000000, 0.0002390712444983297737, 0.0004781424889966595475, 0.0009562849779933203960, 0.001434427466989981245, 0.001673498711488311669, 0.001912569955986642093 ),
 .UNSPECIFIED. ) ;
#68467 = VECTOR ( 'NONE', #77426, 1000.000000000000000 ) ;
#68468 = ORIENTED_EDGE ( 'NONE', *, *, #12569, .F. ) ;
#68469 = CARTESIAN_POINT ( 'NONE',  ( -39.52287095715006870, -29.50247984919015209, -1.443849546365060466 ) ) ;
#68470 = CARTESIAN_POINT ( 'NONE',  ( -57.62287095715004881, -24.66019654487199020, 8.947790411086131712 ) ) ;
#68471 = CARTESIAN_POINT ( 'NONE',  ( 16.01007288495529224, -11.65062672332236104, 11.49999999999999645 ) ) ;
#68472 = CIRCLE ( 'NONE', #81439, 1.399999999999988143 ) ;
#68473 = CARTESIAN_POINT ( 'NONE',  ( 6.660000000000001030, -10.77121780415746599, 1.154761385154455366 ) ) ;
#68474 = EDGE_LOOP ( 'NONE', ( #88889, #57737, #91101, #24303 ) ) ;
#68475 = LINE ( 'NONE', #60381, #436 ) ;
#68476 = LINE ( 'NONE', #99409, #14179 ) ;
#68477 = CARTESIAN_POINT ( 'NONE',  ( 1.064956243273112557, 21.61254047163424019, 11.49999999999998934 ) ) ;
#68478 = CARTESIAN_POINT ( 'NONE',  ( -27.60906388276667656, -24.79421432578786977, 7.602479806744845803 ) ) ;
#68479 = CARTESIAN_POINT ( 'NONE',  ( 18.22972481837485859, -6.773019484731225504, -1.500000000000002220 ) ) ;
#68480 = CARTESIAN_POINT ( 'NONE',  ( -129.6228709571500133, -24.51387760970727214, 9.387446482453416507 ) ) ;
#68481 = DIRECTION ( 'NONE',  ( -0.9496245541219264785, -6.845827386180410961E-16, -0.3133898629642195011 ) ) ;
#68482 = CARTESIAN_POINT ( 'NONE',  ( 12.93213199337649044, -14.99640713134888692, -1.500000000000002220 ) ) ;
#68483 = ORIENTED_EDGE ( 'NONE', *, *, #28257, .F. ) ;
#68484 = CARTESIAN_POINT ( 'NONE',  ( 15.76184642470745700, 12.85868457875834103, 11.49999999999999645 ) ) ;
#68485 = CARTESIAN_POINT ( 'NONE',  ( -80.52209458990078872, -23.48783264082477018, -1.443836473390096131 ) ) ;
#68487 = AXIS2_PLACEMENT_3D ( 'NONE', #6671, #15782, #29505 ) ;
#68486 = LINE ( 'NONE', #69487, #44170 ) ;
#68488 = ORIENTED_EDGE ( 'NONE', *, *, #12535, .T. ) ;
#68489 = CARTESIAN_POINT ( 'NONE',  ( -0.04073145180001176008, -22.52269934801777040, 8.549170486301877148 ) ) ;
#68490 = LINE ( 'NONE', #29417, #96299 ) ;
#68491 = CARTESIAN_POINT ( 'NONE',  ( 30.56234178131493451, -2.630409229859051568, 24.79707536756607666 ) ) ;
#68492 = CARTESIAN_POINT ( 'NONE',  ( -82.55620429048337883, -23.48786465467241058, 11.44779295918255180 ) ) ;
#68493 = CARTESIAN_POINT ( 'NONE',  ( -50.74135369471817825, -25.12871364012075048, 7.068779736917301548 ) ) ;
#68494 = CARTESIAN_POINT ( 'NONE',  ( -19.74138705131307248, -3.616033589355840849, -1.500000000000002220 ) ) ;
#68495 = B_SPLINE_CURVE_WITH_KNOTS ( 'NONE', 3,
 ( #66523, #58886, #26933, #20297, #97440, #49788 ),
 .UNSPECIFIED., .F., .F.,
 ( 4, 2, 4 ),
 ( 6.391158118952235087E-06, 0.001387004593080775738, 0.002767618028042598960 ),
 .UNSPECIFIED. ) ;
#68496 = CARTESIAN_POINT ( 'NONE',  ( 5.184553252003285984, 5.965225279485572685, -28.06387035751381731 ) ) ;
#68497 = VERTEX_POINT ( 'NONE', #1373 ) ;
#68498 = CARTESIAN_POINT ( 'NONE',  ( -63.95380932530888884, -23.56000036390796382, 11.50199999999999889 ) ) ;
#68499 = ADVANCED_FACE ( 'NONE', ( #71383 ), #39919, .F. ) ;
#68500 = CARTESIAN_POINT ( 'NONE',  ( -7.509321099650855480, 21.62252279970214985, 11.49999999999999645 ) ) ;
#68501 = CARTESIAN_POINT ( 'NONE',  ( -49.84984290111637506, -25.31297183315718158, 4.578679947858303123 ) ) ;
#68502 = AXIS2_PLACEMENT_3D ( 'NONE', #98276, #36893, #45518 ) ;
#68503 = DIRECTION ( 'NONE',  ( -3.773278334453079030E-23, 0.9999999999976377785, 2.173523156925979128E-06 ) ) ;
#68504 = CARTESIAN_POINT ( 'NONE',  ( -12.84880425037203011, -5.965225279485592225, -26.59900746623528534 ) ) ;
#68505 = DIRECTION ( 'NONE',  ( 1.000000000000000000, 3.491481338843133355E-15, 2.352173255807796056E-16 ) ) ;
#68506 = EDGE_CURVE ( 'NONE', #20975, #48508, #87093, .T. ) ;
#68507 = DIRECTION ( 'NONE',  ( -0.000000000000000000, -1.000000000000000000, -0.000000000000000000 ) ) ;
#68508 = EDGE_CURVE ( 'NONE', #94949, #46688, #94353, .T. ) ;
#68509 = PLANE ( 'NONE',  #71220 ) ;
#68510 = ORIENTED_EDGE ( 'NONE', *, *, #39914, .T. ) ;
#68511 = CARTESIAN_POINT ( 'NONE',  ( 3.729398819442638846, -20.01364129133569136, -1.500000000000002220 ) ) ;
#68512 = ORIENTED_EDGE ( 'NONE', *, *, #5711, .F. ) ;
#68513 = CARTESIAN_POINT ( 'NONE',  ( -8.204236019480731557, -21.45505762417899831, 11.49999999999998934 ) ) ;
#68514 = DIRECTION ( 'NONE',  ( 0.000000000000000000, 2.173523156925980399E-06, -0.9999999999976378895 ) ) ;
#68515 = ORIENTED_EDGE ( 'NONE', *, *, #6222, .T. ) ;
#68516 = CARTESIAN_POINT ( 'NONE',  ( -101.2400011396082817, -25.16928559910140706, 6.818282878674360781 ) ) ;
#68517 = CARTESIAN_POINT ( 'NONE',  ( -116.5228709571500474, -23.73934037231757443, 11.05740245334327909 ) ) ;
#68518 = B_SPLINE_CURVE_WITH_KNOTS ( 'NONE', 3,
 ( #98159, #30657, #15920, #61628, #46888, #63629, #69728, #8318, #24034, #47890, #206, #1715, #15422, #23019, #32651, #92548, #63124, #78316, #71227, #54008, #31151, #56011, #85945 ),
 .UNSPECIFIED., .F., .F.,
 ( 4, 1, 1, 1, 1, 1, 1, 1, 1, 1, 1, 1, 1, 1, 1, 1, 1, 1, 1, 1, 4 ),
 ( 0.000000000000000000, 0.07295106587586808189, 0.1415836941865457888, 0.2059264601708682696, 0.2653013571846069008, 0.3205972327139294809, 0.3718165030988108688, 0.4187897697094533633, 0.4616987286157644976, 0.5021335821035667335, 0.5408043152926478303, 0.5781805253279665990, 0.6142968652075149194, 0.6496782432647882910, 0.6842994600896379342, 0.7183589527723613921, 0.7520808646475963810, 0.8176524386023853452, 0.8797220764054369813, 0.9399655597309874988, 1.000000000000000000 ),
 .UNSPECIFIED. ) ;
#68519 = VECTOR ( 'NONE', #60752, 1000.000000000000000 ) ;
#68520 = CARTESIAN_POINT ( 'NONE',  ( -96.62287095715009855, -23.94994826722515668, -0.6494450866351711982 ) ) ;
#68522 = ORIENTED_EDGE ( 'NONE', *, *, #24806, .F. ) ;
#68521 = CARTESIAN_POINT ( 'NONE',  ( -21.26230640008892792, -0.7210608269398429693, 11.49999999999999645 ) ) ;
#68523 = APPROVAL_PERSON_ORGANIZATION ( #4963, #42550, #51138 ) ;
#68524 = VERTEX_POINT ( 'NONE', #32306 ) ;
#68525 = CARTESIAN_POINT ( 'NONE',  ( 21.60277357391871433, -5.133695162202882578, 11.49999999999998934 ) ) ;
#68526 = CARTESIAN_POINT ( 'NONE',  ( -9.109090448966927767, 18.51201596650851400, -1.500000000000002220 ) ) ;
#68527 = ORIENTED_EDGE ( 'NONE', *, *, #78638, .F. ) ;
#68529 = ORIENTED_EDGE ( 'NONE', *, *, #35979, .T. ) ;
#68528 = VECTOR ( 'NONE', #42171, 1000.000000000000227 ) ;
#68530 = CARTESIAN_POINT ( 'NONE',  ( -4.495793269230770939, -6.376774720514410077, 19.27714342948718595 ) ) ;
#68531 = CARTESIAN_POINT ( 'NONE',  ( 3.714529970114099022, -5.876774720514425177, 21.83853177191107520 ) ) ;
#68532 = VERTEX_POINT ( 'NONE', #10466 ) ;
#68533 = ORIENTED_EDGE ( 'NONE', *, *, #60214, .T. ) ;
#68534 = AXIS2_PLACEMENT_3D ( 'NONE', #65337, #11508, #74895 ) ;
#68535 = LINE ( 'NONE', #92861, #3277 ) ;
#68536 = DIRECTION ( 'NONE',  ( -0.000000000000000000, -1.000000000000000000, -0.000000000000000000 ) ) ;
#68537 = CARTESIAN_POINT ( 'NONE',  ( 18.58881047053902691, 9.431966241625852732, -1.500000000000002220 ) ) ;
#68538 = CARTESIAN_POINT ( 'NONE',  ( -6.457742198559264679, -20.83860622980983024, 11.49999999999999645 ) ) ;
#68539 = CARTESIAN_POINT ( 'NONE',  ( -40.45231480346743069, -25.31583771044696718, 5.081397513335677907 ) ) ;
#68540 = DIRECTION ( 'NONE',  ( 1.000000000000000000, -7.960204194457801640E-17, 0.000000000000000000 ) ) ;
#68541 = CARTESIAN_POINT ( 'NONE',  ( 22.31695869535024102, -2.478243017838637652, -1.500000000000002220 ) ) ;
#68542 = CARTESIAN_POINT ( 'NONE',  ( -50.72939492065860634, -25.26334739434139820, 4.679804835100300764 ) ) ;
#68543 = EDGE_CURVE ( 'NONE', #20514, #31325, #57169, .T. ) ;
#68544 = ORIENTED_EDGE ( 'NONE', *, *, #42918, .T. ) ;
#68545 = CARTESIAN_POINT ( 'NONE',  ( 13.57151214508650305, 0.000000000000000000, -1.500000000000000666 ) ) ;
#68546 = PLANE ( 'NONE',  #31254 ) ;
#68547 = B_SPLINE_SURFACE_WITH_KNOTS ( 'NONE', 3, 3, ( 
 ( #65993, #96910, #13156, #89799 ),
 ( #97892, #27405, #4574, #65493 ),
 ( #90295, #81690, #96414, #18777 ),
 ( #49759, #12163, #35523, #81185 ),
 ( #80686, #59347, #73580, #43131 ),
 ( #58364, #42148, #26404, #28388 ),
 ( #74567, #12665, #89302, #74082 ) ),
 .UNSPECIFIED., .F., .F., .F.,
 ( 4, 3, 4 ),
 ( 4, 4 ),
 ( 0.3389043340504379054, 0.5146335846998002506, 0.6903628353491626513 ),
 ( 0.7862494037672983493, 0.8171928712212183088 ),
 .UNSPECIFIED. ) ;
#68548 = VERTEX_POINT ( 'NONE', #18575 ) ;
#68549 = VERTEX_POINT ( 'NONE', #33810 ) ;
#68550 = DIRECTION ( 'NONE',  ( 0.000000000000000000, -1.000000000000000000, 0.000000000000000000 ) ) ;
#68551 = VERTEX_POINT ( 'NONE', #33301 ) ;
#68552 = CARTESIAN_POINT ( 'NONE',  ( -21.31669061289120037, -0.5855882196083471714, -1.500000000000002220 ) ) ;
#68553 = ORIENTED_EDGE ( 'NONE', *, *, #73823, .T. ) ;
#68554 = FACE_OUTER_BOUND ( 'NONE', #80919, .T. ) ;
#68555 = CARTESIAN_POINT ( 'NONE',  ( -17.04133944854041616, 12.32129857345222845, 11.49999999999998934 ) ) ;
#68556 = CARTESIAN_POINT ( 'NONE',  ( -30.48449779480992561, -24.66625093156569903, 1.095666116063856776 ) ) ;
#68557 = EDGE_CURVE ( 'NONE', #91720, #91650, #86592, .T. ) ;
#68558 = B_SPLINE_CURVE_WITH_KNOTS ( 'NONE', 3,
 ( #44833, #67182, #37704, #61058, #60065, #6255 ),
 .UNSPECIFIED., .F., .F.,
 ( 4, 2, 4 ),
 ( 6.391158118952235087E-06, 0.001387004593080777906, 0.002767618028042603297 ),
 .UNSPECIFIED. ) ;
#68559 = CARTESIAN_POINT ( 'NONE',  ( -113.5228709571500474, -24.50321055353803601, 9.387540953477508054 ) ) ;
#68560 = B_SPLINE_CURVE_WITH_KNOTS ( 'NONE', 3,
 ( #11722, #82733, #58425, #81743, #58911, #89854 ),
 .UNSPECIFIED., .F., .F.,
 ( 4, 2, 4 ),
 ( 6.391158118970788496E-06, 0.001387004593080791133, 0.002767618028042611537 ),
 .UNSPECIFIED. ) ;
#68561 = CARTESIAN_POINT ( 'NONE',  ( -4.926336369345164279, 5.965225279485592225, -28.61095484066304451 ) ) ;
#68562 = CARTESIAN_POINT ( 'NONE',  ( 16.65356921002588919, 14.36988287374134821, -1.500000000000002220 ) ) ;
#68563 = CARTESIAN_POINT ( 'NONE',  ( -87.63898554099732507, -23.73766607897671221, -1.055555164236430032 ) ) ;
#68564 = ORIENTED_EDGE ( 'NONE', *, *, #20896, .F. ) ;
#68565 = CARTESIAN_POINT ( 'NONE',  ( -122.5185765871470238, -24.66019654487200086, 8.947790411086110396 ) ) ;
#68566 = AXIS2_PLACEMENT_3D ( 'NONE', #5264, #50450, #73292 ) ;
#68567 = EDGE_CURVE ( 'NONE', #80888, #84261, #97931, .T. ) ;
#68568 = ADVANCED_FACE ( 'NONE', ( #80478 ), #49548, .F. ) ;
#68569 = CARTESIAN_POINT ( 'NONE',  ( -84.59927232378923634, -23.73791477778912196, 11.05961554403170588 ) ) ;
#68570 = AXIS2_PLACEMENT_3D ( 'NONE', #69233, #52023, #5839 ) ;
#68571 = EDGE_CURVE ( 'NONE', #31523, #85746, #51950, .T. ) ;
#68572 = CARTESIAN_POINT ( 'NONE',  ( -41.62287095715005592, -23.73907113216990084, -1.053371485793234807 ) ) ;
#68573 = LINE ( 'NONE', #29495, #96691 ) ;
#68574 = CARTESIAN_POINT ( 'NONE',  ( 10.72677997844354536, -18.41129465587203740, -1.500000000000002220 ) ) ;
#68575 = LINE ( 'NONE', #69577, #80649 ) ;
#68576 = EDGE_CURVE ( 'NONE', #34762, #93291, #26616, .T. ) ;
#68577 = CARTESIAN_POINT ( 'NONE',  ( -29.49875734969025842, -0.3587747205144265483, 25.61802280011862720 ) ) ;
#68578 = DIRECTION ( 'NONE',  ( -3.773278334453079618E-23, 0.9999999999976377785, 2.173523156925979975E-06 ) ) ;
#68579 = DIRECTION ( 'NONE',  ( 0.000000000000000000, -0.9999999999976377785, -2.173523156925979128E-06 ) ) ;
#68580 = CARTESIAN_POINT ( 'NONE',  ( -18.83616483605274539, -12.25834331966736102, -1.500000000000002220 ) ) ;
#68581 = CARTESIAN_POINT ( 'NONE',  ( -109.9087718796684356, -25.21970293610405633, 6.713732480141158199 ) ) ;
#68582 = ORIENTED_EDGE ( 'NONE', *, *, #85269, .T. ) ;
#68583 = DIRECTION ( 'NONE',  ( 0.000000000000000000, -0.9999999999976377785, -2.173523156925979128E-06 ) ) ;
#68584 = CARTESIAN_POINT ( 'NONE',  ( -19.61951575358169819, -0.1233725505697131491, 11.49999999999999645 ) ) ;
#68585 = CARTESIAN_POINT ( 'NONE',  ( -68.62287095715004170, -23.72747288104441665, -1.053458166803662444 ) ) ;
#68586 = DIRECTION ( 'NONE',  ( -0.000000000000000000, -1.000000000000000000, -0.000000000000000000 ) ) ;
#68587 = EDGE_CURVE ( 'NONE', #86142, #75490, #53218, .T. ) ;
#68588 = ORIENTED_EDGE ( 'NONE', *, *, #97538, .F. ) ;
#68589 = CARTESIAN_POINT ( 'NONE',  ( -69.06683892470179842, -25.29165132073142885, 5.590026102521621354 ) ) ;
#68590 = DIRECTION ( 'NONE',  ( 0.000000000000000000, -1.000000000000000000, 0.000000000000000000 ) ) ;
#68591 = CARTESIAN_POINT ( 'NONE',  ( -124.6234875168763665, -24.66019654487200441, 8.947790411086108620 ) ) ;
#68592 = CARTESIAN_POINT ( 'NONE',  ( -25.53604547899276156, -24.92361880405457697, 5.314701426448082522 ) ) ;
#68593 = AXIS2_PLACEMENT_3D ( 'NONE', #66397, #89214, #43045 ) ;
#68594 = CARTESIAN_POINT ( 'NONE',  ( 3.669390655483735220, -19.36157329643844704, -1.500000000000002220 ) ) ;
#68595 = ORIENTED_EDGE ( 'NONE', *, *, #27342, .F. ) ;
#68596 = CARTESIAN_POINT ( 'NONE',  ( 8.159923944623203695, 3.316774720514428232, -28.14238247154670347 ) ) ;
#68597 = CARTESIAN_POINT ( 'NONE',  ( -10.34999999999999254, 4.999999999999999112, 2.100000000000000089 ) ) ;
#68598 = AXIS2_PLACEMENT_3D ( 'NONE', #98641, #59111, #21021 ) ;
#68599 = APPROVAL_STATUS ( 'not_yet_approved' ) ;
#68600 = ORIENTED_EDGE ( 'NONE', *, *, #24774, .F. ) ;
#68601 = CARTESIAN_POINT ( 'NONE',  ( -109.6228709571500843, -23.96177878511308990, 10.65340807706329684 ) ) ;
#68602 = CARTESIAN_POINT ( 'NONE',  ( -1.394533802543915124, -6.376774720514413630, 20.19722303762275573 ) ) ;
#68603 = CARTESIAN_POINT ( 'NONE',  ( -55.48559462693079780, -24.73486907724917572, 1.287355809206960355 ) ) ;
#68604 = PLANE ( 'NONE',  #68766 ) ;
#68605 = CARTESIAN_POINT ( 'NONE',  ( -7.326923076923076650, -6.376774720514417183, 20.36318108974359831 ) ) ;
#68606 = CARTESIAN_POINT ( 'NONE',  ( -31.79944283184905274, -24.86441978397624553, 8.247789967200544581 ) ) ;
#68607 = AXIS2_PLACEMENT_3D ( 'NONE', #34521, #72094, #89305 ) ;
#68608 = CARTESIAN_POINT ( 'NONE',  ( -107.5222082047791190, -23.48783264082479505, -1.443836473390060826 ) ) ;
#68609 = CARTESIAN_POINT ( 'NONE',  ( -19.95764006394758638, 0.7380318605572177004, 11.49999999999998934 ) ) ;
#68610 = ADVANCED_FACE ( 'NONE', ( #19075 ), #89593, .T. ) ;
#68611 = CARTESIAN_POINT ( 'NONE',  ( -95.55620429048337883, -25.00182538069145721, 7.747789668545099317 ) ) ;
#68612 = CARTESIAN_POINT ( 'NONE',  ( -51.45327580174686943, -25.31044044580817243, 4.639198480576497197 ) ) ;
#68613 = EDGE_LOOP ( 'NONE', ( #63819, #35211, #97216, #92701 ) ) ;
#68614 = EDGE_CURVE ( 'NONE', #33873, #30676, #5929, .T. ) ;
#68615 = CARTESIAN_POINT ( 'NONE',  ( -119.5172027492807416, -24.65952944569305672, 1.056160979905715003 ) ) ;
#68616 = DIRECTION ( 'NONE',  ( -3.773278334453079030E-23, 0.9999999999976377785, 2.173523156925979128E-06 ) ) ;
#68617 = LINE ( 'NONE', #55403, #44509 ) ;
#68618 = FACE_OUTER_BOUND ( 'NONE', #24027, .T. ) ;
#68619 = CARTESIAN_POINT ( 'NONE',  ( -28.27781825664440873, -25.26026305157151697, 1.715749184898614166 ) ) ;
#68620 = CARTESIAN_POINT ( 'NONE',  ( -1.358974358974357921, -6.376774720514420736, 20.75510817307693046 ) ) ;
#68621 = B_SPLINE_SURFACE_WITH_KNOTS ( 'NONE', 3, 3, ( 
 ( #61063, #53949, #67684, #38201 ),
 ( #69157, #52949, #90996, #52447 ),
 ( #21467, #6259, #37218, #99095 ),
 ( #79264, #1659, #62559, #24481 ),
 ( #17878, #55447, #25987, #55952 ),
 ( #86387, #1156, #16365, #78254 ),
 ( #56459, #56959, #54946, #47831 ),
 ( #8767, #77748, #85886, #8264 ),
 ( #32092, #86882, #39202, #41223 ),
 ( #72176, #47331, #93989, #15862 ) ),
 .UNSPECIFIED., .F., .F., .F.,
 ( 4, 3, 3, 4 ),
 ( 4, 4 ),
 ( 0.7022005934544800487, 0.7765311282028792839, 0.8508616629512784080, 0.9995227324480768782 ),
 ( 0.9496086015441148609, 0.9511872794485528582 ),
 .UNSPECIFIED. ) ;
#68622 = CARTESIAN_POINT ( 'NONE',  ( -79.62287095715004170, -23.96177878511308634, 10.65340807706329862 ) ) ;
#68623 = ADVANCED_FACE ( 'NONE', ( #11468 ), #42441, .F. ) ;
#68624 = CARTESIAN_POINT ( 'NONE',  ( 0.1309051665272248643, -5.876774720514413630, 19.34190049657482291 ) ) ;
#68625 = VERTEX_POINT ( 'NONE', #96699 ) ;
#68626 = APPLICATION_CONTEXT ( 'configuration controlled 3d designs of mechanical parts and assemblies' ) ;
#68627 =( BOUNDED_SURFACE ( )  B_SPLINE_SURFACE ( 3, 2, ( 
 ( #54359, #45736, #91898 ),
 ( #38619, #84287, #69579 ),
 ( #6666, #83790, #14269 ),
 ( #6169, #60482, #37620 ) ),
 .UNSPECIFIED., .F., .F., .T. ) 
 B_SPLINE_SURFACE_WITH_KNOTS ( ( 4, 4 ),
 ( 3, 3 ),
 ( 0.004439845973569162343, 0.004703938444645663561 ),
 ( 0.000000000000000000, 1.000000000000000000 ),
 .UNSPECIFIED. ) 
 GEOMETRIC_REPRESENTATION_ITEM ( )  RATIONAL_B_SPLINE_SURFACE ( (
 ( 1.000000000000000000, 0.9005394799515968884, 1.000000000000000000),
 ( 1.000000000000000000, 0.9005352985759393913, 1.000000000000000000),
 ( 1.000000000000000000, 0.8990570573199260229, 1.000000000000000000),
 ( 1.000000000000000000, 0.8962098481621323387, 1.000000000000000000) ) ) 
 REPRESENTATION_ITEM ( '' )  SURFACE ( )  );
#68628 = CARTESIAN_POINT ( 'NONE',  ( -3.898967980886277829, 19.90457959416237088, 11.49999999999998934 ) ) ;
#68629 = CARTESIAN_POINT ( 'NONE',  ( -122.6239442167820215, -24.51314013834316086, 0.6176544820404212821 ) ) ;
#68630 = EDGE_CURVE ( 'NONE', #72664, #13329, #3875, .T. ) ;
#68631 = CARTESIAN_POINT ( 'NONE',  ( -117.6228709571500417, -24.65952944569305316, 1.056160979905706121 ) ) ;
#68632 = AXIS2_PLACEMENT_3D ( 'NONE', #51710, #36979, #82649 ) ;
#68633 = CARTESIAN_POINT ( 'NONE',  ( 282.9764569301858046, -0.6647747205144264315, 20.79159422840526616 ) ) ;
#68634 = EDGE_LOOP ( 'NONE', ( #12354, #28870, #7780, #14743 ) ) ;
#68635 = FACE_OUTER_BOUND ( 'NONE', #83703, .T. ) ;
#68636 = CARTESIAN_POINT ( 'NONE',  ( -10.54059822343757880, -6.376774720514426953, 22.82308057603841078 ) ) ;
#68637 = CARTESIAN_POINT ( 'NONE',  ( -2.706554608146168217, 19.95013100808389339, -1.500000000000002220 ) ) ;
#68638 = VECTOR ( 'NONE', #11483, 1000.000000000000114 ) ;
#68639 = CARTESIAN_POINT ( 'NONE',  ( 20.24497096899912307, 5.935080660949433096, 11.49999999999999645 ) ) ;
#68640 = CARTESIAN_POINT ( 'NONE',  ( -32.52287095715007581, -24.51283580621450398, 0.6167428607045326583 ) ) ;
#68641 = CARTESIAN_POINT ( 'NONE',  ( 12.17348956504948987, -18.45705692928949659, -1.500000000000002220 ) ) ;
#68643 = CARTESIAN_POINT ( 'NONE',  ( 18.67943556539783856, 8.552475402716291697, -1.500000000000002220 ) ) ;
#68642 = APPROVAL ( #53011, 'UNSPECIFIED' ) ;
#68644 = DIRECTION ( 'NONE',  ( 1.000000000000000000, 3.773278334444168195E-23, 8.201307811038811694E-29 ) ) ;
#68645 = B_SPLINE_CURVE_WITH_KNOTS ( 'NONE', 3,
 ( #80990, #25697, #11473, #48560, #9974, #40928, #71890, #2374, #33305, #10472, #41430, #75856, #91584, #68263 ),
 .UNSPECIFIED., .F., .F.,
 ( 4, 2, 2, 2, 2, 2, 4 ),
 ( 0.000000000000000000, 0.0002036734231732265489, 0.0004073468463464530978, 0.0008146936926928669475, 0.001222040539039280851, 0.001425713962212487532, 0.001629387385385694430 ),
 .UNSPECIFIED. ) ;
#68646 = CARTESIAN_POINT ( 'NONE',  ( -126.6228709571500559, -23.47593901973091235, -1.443836447538995760 ) ) ;
#68647 = VERTEX_POINT ( 'NONE', #4858 ) ;
#68648 = CARTESIAN_POINT ( 'NONE',  ( -70.62287095715005592, -29.50248789122583659, 2.256150453626215580 ) ) ;
#68649 = ORIENTED_EDGE ( 'NONE', *, *, #88534, .F. ) ;
#68650 = DIRECTION ( 'NONE',  ( 1.000000000000000000, 0.000000000000000000, 0.000000000000000000 ) ) ;
#68651 = CARTESIAN_POINT ( 'NONE',  ( -72.58953762381673869, -24.64965694238406968, 8.947790433994660120 ) ) ;
#68652 = ORIENTED_EDGE ( 'NONE', *, *, #52755, .F. ) ;
#68653 = ORIENTED_EDGE ( 'NONE', *, *, #44528, .T. ) ;
#68654 = ORIENTED_EDGE ( 'NONE', *, *, #92154, .T. ) ;
#68655 = PLANE ( 'NONE',  #61580 ) ;
#68656 = DIRECTION ( 'NONE',  ( 0.000000000000000000, 0.000000000000000000, 1.000000000000000000 ) ) ;
#68657 = DIRECTION ( 'NONE',  ( -0.000000000000000000, 2.173523156925979552E-06, -0.9999999999976378895 ) ) ;
#68658 = CARTESIAN_POINT ( 'NONE',  ( -17.42616458466809704, -11.11377323884725321, -1.500000000000002220 ) ) ;
#68659 = CARTESIAN_POINT ( 'NONE',  ( 20.55510029441247610, -6.647428040031946317, 11.49999999999999645 ) ) ;
#68660 = ORIENTED_EDGE ( 'NONE', *, *, #38133, .F. ) ;
#68661 = DIRECTION ( 'NONE',  ( 0.000000000000000000, -9.130123557772668088E-16, -1.000000000000000000 ) ) ;
#68662 = CARTESIAN_POINT ( 'NONE',  ( -57.62287095715004881, -24.64965695001468404, 8.947790433994185832 ) ) ;
#68663 = CARTESIAN_POINT ( 'NONE',  ( -22.37156870845955225, 0.5457896250522937809, -1.500000000000002220 ) ) ;
#68664 = CARTESIAN_POINT ( 'NONE',  ( -111.5228709571500616, -23.47596703998600631, 11.44779298504228038 ) ) ;
#68665 = CARTESIAN_POINT ( 'NONE',  ( -84.63259839552451069, -24.15543982623907482, -0.2315651400026629836 ) ) ;
#68666 = VERTEX_POINT ( 'NONE', #66783 ) ;
#68667 = CARTESIAN_POINT ( 'NONE',  ( 30.45304879119406039, 4.772774720514425972, -10.07140455160086212 ) ) ;
#68668 = CARTESIAN_POINT ( 'NONE',  ( 6.666194146093591399, -6.376774720514413630, 19.75460921626947908 ) ) ;
#68669 = CARTESIAN_POINT ( 'NONE',  ( 2.299058169534009100, 20.76012671103276475, 11.49999999999998934 ) ) ;
#68670 = ORIENTED_EDGE ( 'NONE', *, *, #54318, .T. ) ;
#68672 = ORIENTED_EDGE ( 'NONE', *, *, #74063, .F. ) ;
#68671 = CARTESIAN_POINT ( 'NONE',  ( -67.59731500115069025, -23.96169478059713853, 10.65365249895717881 ) ) ;
#68673 = ORIENTED_EDGE ( 'NONE', *, *, #78154, .T. ) ;
#68674 = VECTOR ( 'NONE', #89686, 1000.000000000000114 ) ;
#68675 = CARTESIAN_POINT ( 'NONE',  ( -109.5890780322650357, -24.35071581493543746, 9.817618358456025263 ) ) ;
#68676 = CARTESIAN_POINT ( 'NONE',  ( 9.297385241821217505, 19.04214385377821017, -1.500000000000002220 ) ) ;
#68677 = EDGE_LOOP ( 'NONE', ( #21126, #61069, #32203, #34592 ) ) ;
#68678 = CARTESIAN_POINT ( 'NONE',  ( -117.6242417137320615, -24.51314013834316086, 0.6176544820404201719 ) ) ;
#68679 = FACE_OUTER_BOUND ( 'NONE', #85017, .T. ) ;
#68680 = CARTESIAN_POINT ( 'NONE',  ( -19.96617879207914825, 8.700599545123990808, -1.500000000000002220 ) ) ;
#68681 = CARTESIAN_POINT ( 'NONE',  ( -7.024122139145243082, -6.376774720514408301, 19.17707164986947532 ) ) ;
#68682 = VECTOR ( 'NONE', #85551, 1000.000000000000114 ) ;
#68683 = DIRECTION ( 'NONE',  ( 0.000000000000000000, 0.000000000000000000, 1.000000000000000000 ) ) ;
#68684 = CARTESIAN_POINT ( 'NONE',  ( -80.52287095715006160, -23.47593901973090169, -1.443836447538996648 ) ) ;
#68685 = CARTESIAN_POINT ( 'NONE',  ( 12.24854465327799424, 17.96525243877979605, -1.500000000000002220 ) ) ;
#68686 = CARTESIAN_POINT ( 'NONE',  ( -79.01600328727082001, -25.22409940181762167, 6.494944116009313539 ) ) ;
#68687 = EDGE_CURVE ( 'NONE', #29538, #18147, #85910, .T. ) ;
#68689 = VERTEX_POINT ( 'NONE', #26700 ) ;
#68688 = CARTESIAN_POINT ( 'NONE',  ( 17.40631026334068565, 13.93540124644318645, 11.49999999999999645 ) ) ;
#68690 = CARTESIAN_POINT ( 'NONE',  ( -40.62287095715005592, -29.50250786944525672, 11.44777988621624232 ) ) ;
#68691 = DIRECTION ( 'NONE',  ( -0.1736481776669261679, 0.9848077530122087975, 0.000000000000000000 ) ) ;
#68692 = DIRECTION ( 'NONE',  ( 0.000000000000000000, -1.000000000000000000, 0.000000000000000000 ) ) ;
#68693 = ORIENTED_EDGE ( 'NONE', *, *, #72561, .F. ) ;
#68694 = VERTEX_POINT ( 'NONE', #65784 ) ;
#68695 = ORIENTED_EDGE ( 'NONE', *, *, #70865, .T. ) ;
#68696 = EDGE_CURVE ( 'NONE', #40720, #6280, #58157, .T. ) ;
#68697 = CARTESIAN_POINT ( 'NONE',  ( -126.2228709571500644, -23.47596703998600987, 11.44779298504227860 ) ) ;
#68698 = CARTESIAN_POINT ( 'NONE',  ( 19.29917393477590437, 8.764703196630867055, -1.500000000000002220 ) ) ;
#68699 = CARTESIAN_POINT ( 'NONE',  ( 10.54059822343757880, -5.876774720514426953, 22.82308057603841078 ) ) ;
#68700 = ADVANCED_FACE ( 'NONE', ( #59152 ), #50534, .F. ) ;
#68701 = CARTESIAN_POINT ( 'NONE',  ( -79.20032202190461135, -25.03138152274833672, 6.885560112372425934 ) ) ;
#68702 = CARTESIAN_POINT ( 'NONE',  ( -82.62287095715005592, -29.50248528299804818, 1.056150453629038477 ) ) ;
#68703 = B_SPLINE_CURVE_WITH_KNOTS ( 'NONE', 3,
 ( #24092, #1771, #94611, #39822, #77372, #31206 ),
 .UNSPECIFIED., .F., .F.,
 ( 4, 2, 4 ),
 ( 1.570887131794638196E-05, 0.001396322306279762591, 0.002776935741241578874 ),
 .UNSPECIFIED. ) ;
#68704 = CARTESIAN_POINT ( 'NONE',  ( -81.42380231474228935, -29.50249428492551829, 5.197779886230994073 ) ) ;
#68705 = CARTESIAN_POINT ( 'NONE',  ( -9.862393454161701101, 16.67994275214481092, -1.500000000000002220 ) ) ;
#68706 = CARTESIAN_POINT ( 'NONE',  ( -39.02475006312682382, -25.32724636324322987, 4.398074533285874388 ) ) ;
#68707 = VERTEX_POINT ( 'NONE', #28694 ) ;
#68708 = CARTESIAN_POINT ( 'NONE',  ( -13.34961138979462270, 14.11212085816309880, 11.49999999999999645 ) ) ;
#68709 = DIRECTION ( 'NONE',  ( 0.000000000000000000, 0.000000000000000000, 1.000000000000000000 ) ) ;
#68710 = ADVANCED_FACE ( 'NONE', ( #73869 ), #90094, .F. ) ;
#68711 = ORIENTED_EDGE ( 'NONE', *, *, #28062, .T. ) ;
#68712 = CIRCLE ( 'NONE', #24943, 1.835999999999983423 ) ;
#68713 = CARTESIAN_POINT ( 'NONE',  ( -64.62287095715005592, -29.50247984919015209, -1.443849546365056913 ) ) ;
#68714 = DIRECTION ( 'NONE',  ( -0.000000000000000000, 1.000000000000000000, -0.000000000000000000 ) ) ;
#68715 = LINE ( 'NONE', #99631, #60125 ) ;
#68716 = CARTESIAN_POINT ( 'NONE',  ( -2.340448316220725467, 19.49152957720520618, 11.49999999999998934 ) ) ;
#68717 = AXIS2_PLACEMENT_3D ( 'NONE', #7735, #90481, #99075 ) ;
#68718 = CARTESIAN_POINT ( 'NONE',  ( -41.39099037118809576, -25.31583651791034129, 4.532732261260102646 ) ) ;
#68719 = ORIENTED_EDGE ( 'NONE', *, *, #47826, .F. ) ;
#68720 = CARTESIAN_POINT ( 'NONE',  ( -10.34410514300256523, -18.92461576200269491, 11.49999999999998934 ) ) ;
#68721 = CARTESIAN_POINT ( 'NONE',  ( -33.48322934098876402, -24.51419770103157347, 9.386484678747185839 ) ) ;
#68722 = CARTESIAN_POINT ( 'NONE',  ( -79.62287095715007013, -24.66019654487199375, 8.947790411086128159 ) ) ;
#68723 = CARTESIAN_POINT ( 'NONE',  ( -99.52924129105133488, -25.18439473889998581, 3.929520434774139037 ) ) ;
#68724 = CARTESIAN_POINT ( 'NONE',  ( 1.912052097559287844, -22.98750448113701239, -1.500000000000002220 ) ) ;
#68725 = COORDINATED_UNIVERSAL_TIME_OFFSET ( 0, 0, .AHEAD. ) ;
#68726 = DIRECTION ( 'NONE',  ( -0.000000000000000000, -1.000000000000000000, -0.000000000000000000 ) ) ;
#68727 = CARTESIAN_POINT ( 'NONE',  ( -51.30672089287874371, -25.29249258120279009, 4.255736650380444352 ) ) ;
#68728 = CARTESIAN_POINT ( 'NONE',  ( -12.53166870608491479, 15.75175023352509385, 11.49999999999999645 ) ) ;
#68729 = CARTESIAN_POINT ( 'NONE',  ( -8.160000000000000142, 0.1579206558577706254, 7.788828319098143105 ) ) ;
#68730 = CARTESIAN_POINT ( 'NONE',  ( -32.52200297606397328, -23.48786465467240347, 11.44779295918255535 ) ) ;
#68731 = CARTESIAN_POINT ( 'NONE',  ( -109.3600771921758223, -25.27538837853246179, 4.143864369237199696 ) ) ;
#68732 = DIRECTION ( 'NONE',  ( 0.000000000000000000, 2.173523156925980399E-06, -0.9999999999976378895 ) ) ;
#68733 = CARTESIAN_POINT ( 'NONE',  ( -30.93930316463115915, -23.47596703998600276, 11.44779298504227683 ) ) ;
#68734 = EDGE_CURVE ( 'NONE', #95233, #20446, #98248, .T. ) ;
#68735 = CARTESIAN_POINT ( 'NONE',  ( 17.36586316225375981, 9.700842922841564686, 11.49999999999998934 ) ) ;
#68736 = CARTESIAN_POINT ( 'NONE',  ( -118.5895376238167245, -23.48786465467241769, 11.44779295918253759 ) ) ;
#68737 = CARTESIAN_POINT ( 'NONE',  ( 7.891737972721761807, -18.10977644326358771, -1.500000000000002220 ) ) ;
#68738 = CARTESIAN_POINT ( 'NONE',  ( -56.59304687066833139, -24.15543982623907127, -0.2315651400026670359 ) ) ;
#68739 = EDGE_CURVE ( 'NONE', #62167, #65645, #986, .T. ) ;
#68740 = CARTESIAN_POINT ( 'NONE',  ( -40.43756433397305727, -25.29116518533085056, 2.832404424262111586 ) ) ;
#68741 = CARTESIAN_POINT ( 'NONE',  ( -2.104002878010082789, -6.376774720514410077, 19.15289935703627222 ) ) ;
#68742 = CARTESIAN_POINT ( 'NONE',  ( -10.67548511050313209, -17.69376651829569269, 11.49999999999999645 ) ) ;
#68743 = CARTESIAN_POINT ( 'NONE',  ( -39.56136241089613037, -25.27985553519108564, 5.536731371927209544 ) ) ;
#68744 = EDGE_CURVE ( 'NONE', #40707, #43478, #7497, .T. ) ;
#68745 = DIRECTION ( 'NONE',  ( -0.000000000000000000, 1.000000000000000000, -0.000000000000000000 ) ) ;
#68747 = EDGE_CURVE ( 'NONE', #29553, #77786, #44765, .T. ) ;
#68746 = CARTESIAN_POINT ( 'NONE',  ( 13.97002500213282516, -17.90638934399130733, 11.49999999999999645 ) ) ;
#68748 = ORIENTED_EDGE ( 'NONE', *, *, #79350, .F. ) ;
#68749 = CARTESIAN_POINT ( 'NONE',  ( 30.45304879119406039, -1.477225279485574028, -10.07140455160086390 ) ) ;
#68750 = CARTESIAN_POINT ( 'NONE',  ( -69.74137862423624767, -25.15171692517981583, 6.930849537325211251 ) ) ;
#68751 = CARTESIAN_POINT ( 'NONE',  ( -12.46103870137906711, 15.87156016069071462, -1.500000000000002220 ) ) ;
#68752 = CARTESIAN_POINT ( 'NONE',  ( -63.54362810327751276, -24.34968618360933235, 0.1864209137778804204 ) ) ;
#68753 = CARTESIAN_POINT ( 'NONE',  ( -84.62287095715005592, -29.50248528299804818, 1.056150453629038477 ) ) ;
#68754 = ORIENTED_EDGE ( 'NONE', *, *, #48087, .T. ) ;
#68755 = ORIENTED_EDGE ( 'NONE', *, *, #11150, .F. ) ;
#68756 = CARTESIAN_POINT ( 'NONE',  ( -10.58858228176428540, -0.3587747205144061202, -27.03148018517017803 ) ) ;
#68757 = CARTESIAN_POINT ( 'NONE',  ( 21.13568926591755925, -8.834425160694816981, -1.500000000000002220 ) ) ;
#68758 = CARTESIAN_POINT ( 'NONE',  ( -50.83488094104556154, -25.18439667156625816, 3.373740327774851000 ) ) ;
#68759 = CARTESIAN_POINT ( 'NONE',  ( 4.348677445931066643, 21.19853102677161871, -1.500000000000002220 ) ) ;
#68760 = LINE ( 'NONE', #14457, #12324 ) ;
#68761 = CARTESIAN_POINT ( 'NONE',  ( -3.826923076923074429, -6.376774720514427841, 21.75000000000000355 ) ) ;
#68762 = CARTESIAN_POINT ( 'NONE',  ( -20.37482282770194075, 4.769447832466558346, 11.49999999999999645 ) ) ;
#68763 = ORIENTED_EDGE ( 'NONE', *, *, #54149, .T. ) ;
#68764 = CARTESIAN_POINT ( 'NONE',  ( -114.9228709571500673, -23.47596703998600276, 11.44779298504227860 ) ) ;
#68765 = CARTESIAN_POINT ( 'NONE',  ( -18.24146354680218707, 12.35505607031776165, -1.500000000000002220 ) ) ;
#68766 = AXIS2_PLACEMENT_3D ( 'NONE', #7189, #61500, #21902 ) ;
#68767 = EDGE_CURVE ( 'NONE', #34072, #96024, #22058, .T. ) ;
#68768 = EDGE_CURVE ( 'NONE', #31190, #98513, #53039, .T. ) ;
#68769 = CARTESIAN_POINT ( 'NONE',  ( -105.5507813405130264, -24.52399227489126687, 9.353111116836517525 ) ) ;
#68770 = CARTESIAN_POINT ( 'NONE',  ( -28.81656857143860861, -25.21724860399139700, 6.988806608617056604 ) ) ;
#68771 = ORIENTED_EDGE ( 'NONE', *, *, #19324, .F. ) ;
#68772 = CARTESIAN_POINT ( 'NONE',  ( -73.52287095715007581, -23.47593901973090169, -1.443836447538996870 ) ) ;
#68773 = DIRECTION ( 'NONE',  ( 0.000000000000000000, 0.000000000000000000, 1.000000000000000000 ) ) ;
#68774 = ORIENTED_EDGE ( 'NONE', *, *, #11411, .F. ) ;
#68775 = FACE_OUTER_BOUND ( 'NONE', #6375, .T. ) ;
#68776 = ORIENTED_EDGE ( 'NONE', *, *, #48369, .T. ) ;
#68777 = EDGE_LOOP ( 'NONE', ( #72826, #73762, #27728, #73421 ) ) ;
#68778 = CARTESIAN_POINT ( 'NONE',  ( -71.58790182756980869, -24.35071581493543391, 9.817618358456021710 ) ) ;
#68779 = FACE_OUTER_BOUND ( 'NONE', #31422, .T. ) ;
#68780 = CARTESIAN_POINT ( 'NONE',  ( -57.63796154297044438, -24.15543982623907127, -0.2315651400026663420 ) ) ;
#68781 = CARTESIAN_POINT ( 'NONE',  ( 14.46511082492616573, -14.46070965572739730, -1.500000000000002220 ) ) ;
#68782 = VECTOR ( 'NONE', #95740, 1000.000000000000114 ) ;
#68783 = ORIENTED_EDGE ( 'NONE', *, *, #96068, .F. ) ;
#68784 = CARTESIAN_POINT ( 'NONE',  ( -3.103301570662693187, -5.876774720514418071, 20.14409848895067512 ) ) ;
#68785 = ADVANCED_FACE ( 'NONE', ( #60160 ), #6845, .T. ) ;
#68786 = CARTESIAN_POINT ( 'NONE',  ( -30.63208233338743725, -23.87624887660336981, 11.01174216661999772 ) ) ;
#68787 = CARTESIAN_POINT ( 'NONE',  ( 13.87573923102662121, 3.316774720514425123, -28.27006591627376508 ) ) ;
#68788 = CARTESIAN_POINT ( 'NONE',  ( -2.790049085472659396, -22.09070898310802633, -1.500000000000002220 ) ) ;
#68789 = ADVANCED_FACE ( 'NONE', ( #5851 ), #37801, .T. ) ;
#68790 = CARTESIAN_POINT ( 'NONE',  ( -4.141439336867657417, -6.376774720514418959, 20.56083401959468304 ) ) ;
#68791 = PLANE ( 'NONE',  #12407 ) ;
#68792 = ORIENTED_EDGE ( 'NONE', *, *, #30567, .T. ) ;
#68793 = CARTESIAN_POINT ( 'NONE',  ( 2.449489742783179214, -1.473225279485573358, 2.499999999999999112 ) ) ;
#68794 = CARTESIAN_POINT ( 'NONE',  ( -28.54076794517382965, -25.26248034578510371, 8.057460879817709198 ) ) ;
#68795 = CARTESIAN_POINT ( 'NONE',  ( 20.70993026999094511, 1.908435391604796028, 11.49999999999998934 ) ) ;
#68796 = ORIENTED_EDGE ( 'NONE', *, *, #48598, .T. ) ;
#68798 = ORIENTED_EDGE ( 'NONE', *, *, #24101, .T. ) ;
#68797 = CARTESIAN_POINT ( 'NONE',  ( 4.413617546364139166, -6.376774720514406525, 18.86076033669171181 ) ) ;
#68799 = CARTESIAN_POINT ( 'NONE',  ( -119.2228709571500787, -23.47596703998600276, 11.44779298504227683 ) ) ;
#68800 = ORIENTED_EDGE ( 'NONE', *, *, #59642, .F. ) ;
#68801 = ORIENTED_EDGE ( 'NONE', *, *, #28977, .T. ) ;
#68802 = CARTESIAN_POINT ( 'NONE',  ( 7.777929354962648922, 10.59658755993304524, -0.9270812835540120922 ) ) ;
#68803 = CARTESIAN_POINT ( 'NONE',  ( -50.55649023882089921, -25.10935758318566968, 2.837765538655498077 ) ) ;
#68804 = CARTESIAN_POINT ( 'NONE',  ( -77.62287095715005592, -29.50250243563736774, 8.947779886222141599 ) ) ;
#68805 = CARTESIAN_POINT ( 'NONE',  ( 1.949999999999999956, -0.1925000000000001155, -0.1925000000000000600 ) ) ;
#68806 = CARTESIAN_POINT ( 'NONE',  ( -92.50938377975539595, -24.35071581493542681, 9.817618358456023486 ) ) ;
#68807 = DIRECTION ( 'NONE',  ( -0.000000000000000000, 1.000000000000000000, -0.000000000000000000 ) ) ;
#68808 = ADVANCED_FACE ( 'NONE', ( #7842 ), #76344, .F. ) ;
#68810 = ORIENTED_EDGE ( 'NONE', *, *, #27450, .T. ) ;
#68809 = CARTESIAN_POINT ( 'NONE',  ( 2.574831182292884435, -22.01391258260016315, 11.49999999999999645 ) ) ;
#68811 = FACE_OUTER_BOUND ( 'NONE', #18298, .T. ) ;
#68812 = CARTESIAN_POINT ( 'NONE',  ( 5.572475817582897228, 21.94689365879375131, -1.500000000000002220 ) ) ;
#68814 = ORIENTED_EDGE ( 'NONE', *, *, #65153, .T. ) ;
#68813 = CARTESIAN_POINT ( 'NONE',  ( -124.6228709571500559, -23.47593901973091235, -1.443836447538997536 ) ) ;
#68815 = ORIENTED_EDGE ( 'NONE', *, *, #58597, .F. ) ;
#68816 = AXIS2_PLACEMENT_3D ( 'NONE', #56769, #94802, #41032 ) ;
#68817 = CARTESIAN_POINT ( 'NONE',  ( -112.9228709571500673, -23.47596703998600631, 11.44779298504227860 ) ) ;
#68818 = ADVANCED_FACE ( 'NONE', ( #100165 ), #29187, .F. ) ;
#68819 = CARTESIAN_POINT ( 'NONE',  ( -8.609638109768802394, 18.19638482192696216, 11.49999999999998934 ) ) ;
#68820 = EDGE_CURVE ( 'NONE', #62489, #45200, #77450, .T. ) ;
#68821 = B_SPLINE_SURFACE_WITH_KNOTS ( 'NONE', 3, 3, ( 
 ( #65767, #98172, #58143, #42914 ),
 ( #59635, #21047, #52016, #52515 ),
 ( #89080, #4840, #5334, #73853 ),
 ( #82945, #97683, #83446, #91065 ),
 ( #97188, #19556, #20060, #50515 ),
 ( #81473, #35793, #44909, #11947 ),
 ( #59137, #35302, #27683, #51521 ) ),
 .UNSPECIFIED., .F., .F., .F.,
 ( 4, 3, 4 ),
 ( 4, 4 ),
 ( 0.0004766839783825173532, 0.1029713700210899696, 0.2054660560637974198 ),
 ( 0.1695371245961057594, 0.1706280732699167746 ),
 .UNSPECIFIED. ) ;
#68822 = FACE_OUTER_BOUND ( 'NONE', #30096, .T. ) ;
#68823 = ORIENTED_EDGE ( 'NONE', *, *, #87484, .F. ) ;
#68824 = CARTESIAN_POINT ( 'NONE',  ( -126.5228709571500616, -24.65952944569305316, 1.056160979905707675 ) ) ;
#68825 = CARTESIAN_POINT ( 'NONE',  ( 21.86734719908870872, 4.625976558377421277, -1.500000000000002220 ) ) ;
#68826 = EDGE_CURVE ( 'NONE', #20337, #10587, #90768, .T. ) ;
#68827 = VERTEX_POINT ( 'NONE', #13453 ) ;
#68828 = ORIENTED_EDGE ( 'NONE', *, *, #68134, .T. ) ;
#68829 = CARTESIAN_POINT ( 'NONE',  ( 15.32643653063177958, -2.682774720514426559, -27.14485409495429380 ) ) ;
#68830 = PLANE ( 'NONE',  #62096 ) ;
#68831 = CARTESIAN_POINT ( 'NONE',  ( -60.52287095715006160, -29.50248528299804818, 1.056150453629034924 ) ) ;
#68832 = CARTESIAN_POINT ( 'NONE',  ( -119.6228709571500559, -23.47593901973091235, -1.443836447538997536 ) ) ;
#68833 = ADVANCED_FACE ( 'NONE', ( #29686 ), #44428, .T. ) ;
#68834 = CARTESIAN_POINT ( 'NONE',  ( -73.52287095715007581, -24.64965694238407323, 8.947790433994200043 ) ) ;
#68835 = CARTESIAN_POINT ( 'NONE',  ( 19.50827032651345405, -1.201405007418623994, -1.500000000000002220 ) ) ;
#68836 = CARTESIAN_POINT ( 'NONE',  ( 29.73860345376319003, -4.772774720514425972, -8.849814207987163783 ) ) ;
#68837 = CARTESIAN_POINT ( 'NONE',  ( 5.910897418159350103, -20.63055655796343757, -1.500000000000002220 ) ) ;
#68838 = CARTESIAN_POINT ( 'NONE',  ( -25.60037597819128763, -24.57999985355001016, 3.875573678034330616 ) ) ;
#68839 = CARTESIAN_POINT ( 'NONE',  ( -120.5228709571500332, -23.85196035786901803, -0.8779234886475113520 ) ) ;
#68840 = PLANE ( 'NONE',  #94602 ) ;
#68842 = AXIS2_PLACEMENT_3D ( 'NONE', #1368, #42803, #40917 ) ;
#68841 = CARTESIAN_POINT ( 'NONE',  ( -6.237877366497927234, -22.00199818733190327, -1.500000000000002220 ) ) ;
#68843 = DATE_TIME_ROLE ( 'classification_date' ) ;
#68844 = CARTESIAN_POINT ( 'NONE',  ( -101.9507253916653440, -25.25287247409162816, 6.236250661346385726 ) ) ;
#68845 = LINE ( 'NONE', #29778, #24745 ) ;
#68846 = CARTESIAN_POINT ( 'NONE',  ( -4.560224734120114753, 19.45435480350565882, 11.49999999999999645 ) ) ;
#68847 = CARTESIAN_POINT ( 'NONE',  ( 8.971512145086503409, -1.028487854913504140, -5.500000000000000000 ) ) ;
#68848 = CARTESIAN_POINT ( 'NONE',  ( -74.54564100032425245, -24.35071581493544102, 9.817618358456019934 ) ) ;
#68849 = DIRECTION ( 'NONE',  ( -1.000000000000000000, 0.000000000000000000, 0.000000000000000000 ) ) ;
#68850 = ORIENTED_EDGE ( 'NONE', *, *, #39792, .F. ) ;
#68851 = FACE_OUTER_BOUND ( 'NONE', #7694, .T. ) ;
#68852 = DIRECTION ( 'NONE',  ( -0.09721092304694051167, 0.000000000000000000, 0.9952638024365005887 ) ) ;
#68853 = CARTESIAN_POINT ( 'NONE',  ( 20.36105213711617878, 7.643125777291208678, 11.49999999999998934 ) ) ;
#68854 = CARTESIAN_POINT ( 'NONE',  ( -65.92287095715006728, -23.47596703998600631, 11.44779298504227860 ) ) ;
#68855 = CARTESIAN_POINT ( 'NONE',  ( -16.94305004876727239, 9.801747318927828800, -1.500000000000002220 ) ) ;
#68856 = PLANE ( 'NONE',  #52308 ) ;
#68857 = EDGE_CURVE ( 'NONE', #7606, #22830, #72631, .T. ) ;
#68858 = APPROVAL_STATUS ( 'not_yet_approved' ) ;
#68859 = CARTESIAN_POINT ( 'NONE',  ( -30.65075040189094580, -23.47621662958674804, 11.44779298504227683 ) ) ;
#68860 = CARTESIAN_POINT ( 'NONE',  ( 3.714529970114099022, -5.876774720514426065, 21.83853177191107520 ) ) ;
#68861 = CARTESIAN_POINT ( 'NONE',  ( 17.35315496411208613, -10.91789592880838811, 11.49999999999999645 ) ) ;
#68862 = CARTESIAN_POINT ( 'NONE',  ( -94.52287095715006160, -24.64898659630367916, 1.056161002820827921 ) ) ;
#68863 = CARTESIAN_POINT ( 'NONE',  ( 27.53860345374771867, -4.772774720514425972, -9.482392034746242260 ) ) ;
#68864 = VERTEX_POINT ( 'NONE', #7335 ) ;
#68865 = DIRECTION ( 'NONE',  ( 0.000000000000000000, 0.000000000000000000, -1.000000000000000000 ) ) ;
#68866 = CARTESIAN_POINT ( 'NONE',  ( -40.25588136632453740, -25.28892425241502551, 3.308431897907366359 ) ) ;
#68867 = CARTESIAN_POINT ( 'NONE',  ( -125.5209391444894749, -24.15602025860897584, 10.28564288303534013 ) ) ;
#68868 = CARTESIAN_POINT ( 'NONE',  ( 30.09341516180546350, 1.477225279485574028, -11.39311774897855933 ) ) ;
#68869 = DIRECTION ( 'NONE',  ( 0.000000000000000000, 0.9999999999976377785, 2.173523156925979128E-06 ) ) ;
#68870 = CARTESIAN_POINT ( 'NONE',  ( 33.00535138976610483, -5.965225279485572685, -12.97242311383961066 ) ) ;
#68871 = CARTESIAN_POINT ( 'NONE',  ( 14.65057173600216345, 17.85730367728733725, 11.49999999999999645 ) ) ;
#68872 = CARTESIAN_POINT ( 'NONE',  ( -10.93939140624874007, -20.02795264745160608, -1.500000000000002220 ) ) ;
#68873 = CARTESIAN_POINT ( 'NONE',  ( 4.127614219445591814, -5.876774720514408301, 18.60403502951120558 ) ) ;
#68874 = CARTESIAN_POINT ( 'NONE',  ( 21.57151214508649772, 0.000000000000000000, 1.500000000000000666 ) ) ;
#68875 = CARTESIAN_POINT ( 'NONE',  ( -123.5228709571500616, -24.65952944569304961, 1.056160979905705899 ) ) ;
#68876 = VECTOR ( 'NONE', #43287, 1000.000000000000114 ) ;
#68877 = CARTESIAN_POINT ( 'NONE',  ( -109.5948960647422723, -25.15277794460069671, 6.986250878905949868 ) ) ;
#68878 = DIRECTION ( 'NONE',  ( -1.000000000000000000, 0.000000000000000000, 0.000000000000000000 ) ) ;
#68879 = CARTESIAN_POINT ( 'NONE',  ( 21.74639208212181529, -2.611101805624240768, -1.500000000000002220 ) ) ;
#68880 = CARTESIAN_POINT ( 'NONE',  ( -5.755030174389611730, -5.876774720514410077, 19.56655654527324728 ) ) ;
#68881 = EDGE_CURVE ( 'NONE', #6691, #11783, #22548, .T. ) ;
#68882 = CARTESIAN_POINT ( 'NONE',  ( -50.62287095715007723, -24.15431212366392444, -0.2830839119429141570 ) ) ;
#68883 = CARTESIAN_POINT ( 'NONE',  ( -41.02757408530191441, -25.31561146209963198, 4.926386051049478354 ) ) ;
#68884 = DIRECTION ( 'NONE',  ( 0.000000000000000000, -1.000000000000000000, -2.816109538923387391E-16 ) ) ;
#68885 = FACE_OUTER_BOUND ( 'NONE', #60051, .T. ) ;
#68886 = ORIENTED_EDGE ( 'NONE', *, *, #12306, .T. ) ;
#68887 = CARTESIAN_POINT ( 'NONE',  ( 16.50020720150075348, -12.08490501797973238, -1.500000000000002220 ) ) ;
#68888 = ORIENTED_EDGE ( 'NONE', *, *, #2603, .F. ) ;
#68889 = ORIENTED_EDGE ( 'NONE', *, *, #72369, .T. ) ;
#68890 = ORIENTED_EDGE ( 'NONE', *, *, #45302, .T. ) ;
#68891 = ORIENTED_EDGE ( 'NONE', *, *, #31509, .F. ) ;
#68892 = CARTESIAN_POINT ( 'NONE',  ( -22.22199965279648737, -6.226755796435518242, 11.49999999999998934 ) ) ;
#68893 = CARTESIAN_POINT ( 'NONE',  ( -40.80038310650994759, -25.18341647909762671, 3.283321612209681550 ) ) ;
#68894 = CARTESIAN_POINT ( 'NONE',  ( 20.05691770114479766, 3.104179615465487707, -1.500000000000002220 ) ) ;
#68895 = ORIENTED_EDGE ( 'NONE', *, *, #22674, .T. ) ;
#68896 = EDGE_CURVE ( 'NONE', #48223, #47437, #61662, .T. ) ;
#68897 = CARTESIAN_POINT ( 'NONE',  ( -26.08159193753483507, -24.86405713208039359, 6.759032221908315208 ) ) ;
#68898 = EDGE_CURVE ( 'NONE', #44666, #56810, #2749, .T. ) ;
#68899 = CARTESIAN_POINT ( 'NONE',  ( -87.62287095715008434, -24.51387760970723306, 9.387446482453421837 ) ) ;
#68900 = ADVANCED_FACE ( 'NONE', ( #8845 ), #85460, .T. ) ;
#68901 = B_SPLINE_CURVE_WITH_KNOTS ( 'NONE', 3,
 ( #34541, #80209, #88326, #26925, #58878, #10702, #26430, #12685, #43648, #73108, #57894, #3597, #74586, #50767, #66514, #5076 ),
 .UNSPECIFIED., .F., .F.,
 ( 4, 2, 2, 2, 2, 2, 2, 4 ),
 ( 0.000000000000000000, 0.0002571301802276845013, 0.0005142603604553690026, 0.001028520720910736704, 0.001285650901138406677, 0.001542781081366076217, 0.001799911261593746190, 0.002057041441821416163 ),
 .UNSPECIFIED. ) ;
#68902 = LINE ( 'NONE', #68408, #85305 ) ;
#68903 = CARTESIAN_POINT ( 'NONE',  ( -70.59774629277985980, -24.15503026093916006, -0.2815557561904372674 ) ) ;
#68905 = ORIENTED_EDGE ( 'NONE', *, *, #42097, .F. ) ;
#68904 = CARTESIAN_POINT ( 'NONE',  ( -17.32345979880200204, -12.59856583755568415, 11.49999999999999645 ) ) ;
#68906 = CARTESIAN_POINT ( 'NONE',  ( -100.5562042904834072, -23.47593901973091235, -1.443836447539001089 ) ) ;
#68907 = CARTESIAN_POINT ( 'NONE',  ( -20.27875734969026311, 3.456774720514426136, 24.00402280011862288 ) ) ;
#68908 = EDGE_CURVE ( 'NONE', #12709, #90732, #24061, .T. ) ;
#68909 = ORIENTED_EDGE ( 'NONE', *, *, #3220, .T. ) ;
#68910 = CARTESIAN_POINT ( 'NONE',  ( 11.71144010791963730, -17.07555522294065753, -1.500000000000002220 ) ) ;
#68911 = AXIS2_PLACEMENT_3D ( 'NONE', #82113, #90226, #5484 ) ;
#68912 = EDGE_LOOP ( 'NONE', ( #7986, #39608, #1292, #59081 ) ) ;
#68914 = ORIENTED_EDGE ( 'NONE', *, *, #47264, .T. ) ;
#68913 = FACE_OUTER_BOUND ( 'NONE', #42709, .T. ) ;
#68915 = CARTESIAN_POINT ( 'NONE',  ( -28.59443407473934329, -23.99887327325441788, -0.2315644524145782090 ) ) ;
#68916 = ORIENTED_EDGE ( 'NONE', *, *, #86551, .F. ) ;
#68917 = CARTESIAN_POINT ( 'NONE',  ( 4.531089049250198286, -5.876774720514402972, 18.46391971337801508 ) ) ;
#68918 = CARTESIAN_POINT ( 'NONE',  ( -65.48792298204898543, -24.83618233451449697, 1.606449574219540155 ) ) ;
#68919 = EDGE_CURVE ( 'NONE', #53307, #40253, #31455, .T. ) ;
#68920 = CARTESIAN_POINT ( 'NONE',  ( -21.79611004543898289, 2.820803583321412678, 11.49999999999999645 ) ) ;
#68921 = CIRCLE ( 'NONE', #96447, 18.35000000000000142 ) ;
#68922 = DIRECTION ( 'NONE',  ( 0.000000000000000000, 0.000000000000000000, 1.000000000000000000 ) ) ;
#68923 = CARTESIAN_POINT ( 'NONE',  ( 4.940617368476682536, -22.01678987175928981, -1.500000000000002220 ) ) ;
#68924 = AXIS2_PLACEMENT_3D ( 'NONE', #48575, #86612, #17098 ) ;
#68925 = CARTESIAN_POINT ( 'NONE',  ( -3.838044578953509145, 20.63102806057878880, -1.500000000000002220 ) ) ;
#68926 = DIRECTION ( 'NONE',  ( -3.773278334453079030E-23, 0.9999999999976377785, 2.173523156925979128E-06 ) ) ;
#68927 = DIRECTION ( 'NONE',  ( -0.06283980576413537855, 0.000000000000000000, -0.9980236263794188822 ) ) ;
#68929 = EDGE_CURVE ( 'NONE', #43843, #79545, #35040, .T. ) ;
#68928 = ORIENTED_EDGE ( 'NONE', *, *, #84145, .F. ) ;
#68930 = ORIENTED_EDGE ( 'NONE', *, *, #99782, .T. ) ;
#68931 = ORIENTED_EDGE ( 'NONE', *, *, #33554, .F. ) ;
#68932 = CARTESIAN_POINT ( 'NONE',  ( -88.52287095715006160, -24.33927499327854349, 9.819080762295801179 ) ) ;
#68933 = ADVANCED_FACE ( 'NONE', ( #47918 ), #55538, .T. ) ;
#68934 = CARTESIAN_POINT ( 'NONE',  ( 11.68953838083566588, 18.09531432177502808, -1.500000000000002220 ) ) ;
#68935 = B_SPLINE_CURVE_WITH_KNOTS ( 'NONE', 3,
 ( #32782, #63762, #58627, #13931, #83947, #12438 ),
 .UNSPECIFIED., .F., .F.,
 ( 4, 2, 4 ),
 ( 6.384118678607784034E-06, 0.001386860460828371082, 0.002767336802978134086 ),
 .UNSPECIFIED. ) ;
#68936 = CARTESIAN_POINT ( 'NONE',  ( -105.5228709571500616, -24.51254535375846189, 9.355368624242128561 ) ) ;
#68937 = ORIENTED_EDGE ( 'NONE', *, *, #16769, .F. ) ;
#68938 = CARTESIAN_POINT ( 'NONE',  ( -18.40674794014382698, -10.35651468716735657, -1.500000000000002220 ) ) ;
#68939 = FACE_OUTER_BOUND ( 'NONE', #8066, .T. ) ;
#68940 = CARTESIAN_POINT ( 'NONE',  ( -64.64729366872971639, -23.73766607897670156, -1.055555164236459564 ) ) ;
#68941 = FACE_OUTER_BOUND ( 'NONE', #56173, .T. ) ;
#68942 = DIRECTION ( 'NONE',  ( 0.000000000000000000, 0.9513357669802769978, -0.3081562241202474572 ) ) ;
#68943 = CARTESIAN_POINT ( 'NONE',  ( -0.4909855769230799249, -5.876774720514410077, 19.14743589743590491 ) ) ;
#68944 = CARTESIAN_POINT ( 'NONE',  ( 12.10043277420606778, 18.60588626676543100, -1.500000000000002220 ) ) ;
#68945 = CARTESIAN_POINT ( 'NONE',  ( -40.52287095715006870, -23.47593901973090169, -1.443836447538997092 ) ) ;
#68946 = EDGE_CURVE ( 'NONE', #95392, #76295, #85969, .T. ) ;
#68947 = ORIENTED_EDGE ( 'NONE', *, *, #36647, .F. ) ;
#68948 = CARTESIAN_POINT ( 'NONE',  ( -51.81420417462592809, -25.31633237273065618, 5.643201719655072779 ) ) ;
#68949 = CARTESIAN_POINT ( 'NONE',  ( -67.62287095715005592, -24.64898659630367916, 1.056161002820824368 ) ) ;
#68950 = CARTESIAN_POINT ( 'NONE',  ( 10.46399479596398052, -3.316774720514422903, -27.03001098546561209 ) ) ;
#68951 = EDGE_CURVE ( 'NONE', #46913, #62281, #3616, .T. ) ;
#68952 = CARTESIAN_POINT ( 'NONE',  ( 2.000000000000000000, 0.000000000000000000, 0.000000000000000000 ) ) ;
#68953 = CARTESIAN_POINT ( 'NONE',  ( 1.255614643274026276, -19.41590359075080841, -1.500000000000002220 ) ) ;
#68954 = VECTOR ( 'NONE', #48164, 1000.000000000000114 ) ;
#68955 = CARTESIAN_POINT ( 'NONE',  ( -21.18999663186871274, 2.814949255606389311, -1.500000000000002220 ) ) ;
#68956 = DIRECTION ( 'NONE',  ( -0.000000000000000000, -1.000000000000000000, -0.000000000000000000 ) ) ;
#68957 = CARTESIAN_POINT ( 'NONE',  ( -90.70915032798693289, -25.26877915520014639, 5.947789088310639904 ) ) ;
#68958 = LINE ( 'NONE', #22262, #14640 ) ;
#68959 = CARTESIAN_POINT ( 'NONE',  ( 8.071512145086501278, -1.028487854913507915, -3.750000000000000444 ) ) ;
#68960 = CARTESIAN_POINT ( 'NONE',  ( -9.076218414377828836, -20.82814578352222767, -1.500000000000002220 ) ) ;
#68961 = ORIENTED_EDGE ( 'NONE', *, *, #74513, .T. ) ;
#68962 = FACE_OUTER_BOUND ( 'NONE', #22461, .T. ) ;
#68963 = CARTESIAN_POINT ( 'NONE',  ( -62.62287095715004881, -23.73934037231756733, 11.05740245334329153 ) ) ;
#68964 = CARTESIAN_POINT ( 'NONE',  ( -17.91562471463183570, -8.470225615102204841, 11.49999999999999645 ) ) ;
#68965 = DIRECTION ( 'NONE',  ( 0.000000000000000000, 0.000000000000000000, -1.000000000000000000 ) ) ;
#68966 = ORIENTED_EDGE ( 'NONE', *, *, #16436, .T. ) ;
#68967 = CARTESIAN_POINT ( 'NONE',  ( -5.891025641025639636, -5.876774720514419847, 20.75510817307693046 ) ) ;
#68968 = CARTESIAN_POINT ( 'NONE',  ( -75.52287095715009002, -24.83620972994592435, 8.398175272781367440 ) ) ;
#68969 = CARTESIAN_POINT ( 'NONE',  ( 18.46943957830784555, -11.30625484363265265, 11.49999999999998934 ) ) ;
#68970 = CARTESIAN_POINT ( 'NONE',  ( 7.150000000000004796, -2.000000000000001776, 18.24068255301867936 ) ) ;
#68971 = CARTESIAN_POINT ( 'NONE',  ( -7.106217341473486826, 18.08270997100935418, -1.500000000000002220 ) ) ;
#68972 = DIRECTION ( 'NONE',  ( 0.000000000000000000, -0.9999999999976377785, -2.173523156925979975E-06 ) ) ;
#68973 = CARTESIAN_POINT ( 'NONE',  ( -82.62287095715005592, -23.48786465467241413, 11.44779295918254647 ) ) ;
#68974 = CARTESIAN_POINT ( 'NONE',  ( 6.388261542594571019, -18.74682169789839392, 11.49999999999998934 ) ) ;
#68975 = B_SPLINE_CURVE_WITH_KNOTS ( 'NONE', 3,
 ( #100196, #92111, #93104, #22579 ),
 .UNSPECIFIED., .F., .F.,
 ( 4, 4 ),
 ( 0.000000000000000000, 0.0001000000000000028644 ),
 .UNSPECIFIED. ) ;
#68976 = ORIENTED_EDGE ( 'NONE', *, *, #73723, .T. ) ;
#68977 = CARTESIAN_POINT ( 'NONE',  ( -12.35269427871797987, -16.12754648828645543, 11.49999999999999645 ) ) ;
#68978 = DIRECTION ( 'NONE',  ( -1.000000000000000000, -3.773278334444166432E-23, -8.201307841325785021E-29 ) ) ;
#68979 = B_SPLINE_CURVE_WITH_KNOTS ( 'NONE', 3,
 ( #34110, #94494, #49848, #33601, #40215, #72672, #1658, #33101, #71168, #41222, #3171, #64585, #32595, #71670, #2168, #65083, #94994, #11262 ),
 .UNSPECIFIED., .F., .F.,
 ( 4, 2, 2, 2, 2, 2, 2, 2, 4 ),
 ( 0.000000000000000000, 0.0005980878512858794297, 0.001196175702571757558, 0.001794263553857635470, 0.002392351405143513382, 0.002990439256429391728, 0.003588527107715270073, 0.004186614959001148419, 0.004784702810287026764 ),
 .UNSPECIFIED. ) ;
#68980 = VECTOR ( 'NONE', #62162, 1000.000000000000000 ) ;
#68981 = FACE_OUTER_BOUND ( 'NONE', #60921, .T. ) ;
#68982 = VERTEX_POINT ( 'NONE', #71252 ) ;
#68983 = CARTESIAN_POINT ( 'NONE',  ( -30.59128290392954597, -24.93418366566757882, 8.369064737642425200 ) ) ;
#68984 = FACE_OUTER_BOUND ( 'NONE', #47859, .T. ) ;
#68985 = CARTESIAN_POINT ( 'NONE',  ( -49.63502199369077772, -25.25214439884339157, 4.997542013878374156 ) ) ;
#68986 = VECTOR ( 'NONE', #51848, 1000.000000000000000 ) ;
#68987 = CARTESIAN_POINT ( 'NONE',  ( -40.64475957891966118, -24.40133493613049609, 9.663955038902802386 ) ) ;
#68988 = VECTOR ( 'NONE', #93904, 1000.000000000000000 ) ;
#68989 = CARTESIAN_POINT ( 'NONE',  ( -127.6228709571500559, -24.64965695001469115, 8.947790433994173398 ) ) ;
#68990 = CARTESIAN_POINT ( 'NONE',  ( -19.29710791919172053, 5.528754708966634901, 11.49999999999998934 ) ) ;
#68991 = AXIS2_PLACEMENT_3D ( 'NONE', #98989, #90394, #29479 ) ;
#68992 = CARTESIAN_POINT ( 'NONE',  ( -74.62287095715005592, -23.47593901973091235, -1.443836447539006196 ) ) ;
#68993 = VERTEX_POINT ( 'NONE', #63150 ) ;
#68994 = DIRECTION ( 'NONE',  ( 0.000000000000000000, 0.000000000000000000, -1.000000000000000000 ) ) ;
#68995 = CIRCLE ( 'NONE', #91656, 24.00000000000000000 ) ;
#68996 = CARTESIAN_POINT ( 'NONE',  ( -22.23020047961643186, 5.420056861400933457, 11.49999999999999645 ) ) ;
#68997 = CARTESIAN_POINT ( 'NONE',  ( -20.99730734726578874, -8.693733401623333634, -1.500000000000002220 ) ) ;
#68998 = CARTESIAN_POINT ( 'NONE',  ( -30.47287095715008576, -23.78427885734157954, -0.9431990486725588818 ) ) ;
#68999 = CARTESIAN_POINT ( 'NONE',  ( -97.55620429048340725, -23.47593901973091235, -1.443836447539001089 ) ) ;
#69000 = CARTESIAN_POINT ( 'NONE',  ( -38.52201939144443799, -23.48786465467240347, 11.44779295918255002 ) ) ;
#69001 = CARTESIAN_POINT ( 'NONE',  ( -108.5228709571500758, -23.47593901973090524, -1.443836447538996204 ) ) ;
#69002 = CARTESIAN_POINT ( 'NONE',  ( 32.90495245295455362, 3.622774720514437607, -13.06061886496134861 ) ) ;
#69003 = LINE ( 'NONE', #46173, #59858 ) ;
#69004 = ORIENTED_EDGE ( 'NONE', *, *, #28822, .F. ) ;
#69005 = EDGE_CURVE ( 'NONE', #65202, #84765, #54466, .T. ) ;
#69006 = CARTESIAN_POINT ( 'NONE',  ( 20.27773211485958527, -1.686570798567030183, -1.500000000000002220 ) ) ;
#69008 = EDGE_CURVE ( 'NONE', #65701, #6520, #88255, .T. ) ;
#69007 = ORIENTED_EDGE ( 'NONE', *, *, #38598, .T. ) ;
#69009 = CARTESIAN_POINT ( 'NONE',  ( -10.52143791818333085, 20.43947972196396989, -1.500000000000002220 ) ) ;
#69010 = DIRECTION ( 'NONE',  ( 0.000000000000000000, -2.173523156925979552E-06, 0.9999999999976378895 ) ) ;
#69011 = EDGE_CURVE ( 'NONE', #56283, #26914, #62649, .T. ) ;
#69012 = ORIENTED_EDGE ( 'NONE', *, *, #92299, .F. ) ;
#69013 = DIRECTION ( 'NONE',  ( 0.000000000000000000, 0.000000000000000000, -1.000000000000000000 ) ) ;
#69014 = EDGE_CURVE ( 'NONE', #87739, #62329, #83378, .T. ) ;
#69016 = EDGE_CURVE ( 'NONE', #9746, #3529, #79351, .T. ) ;
#69015 = DIRECTION ( 'NONE',  ( 0.000000000000000000, 0.000000000000000000, -1.000000000000000000 ) ) ;
#69017 = CARTESIAN_POINT ( 'NONE',  ( -51.55335675300738529, -23.96169478059712787, 10.65365249895718236 ) ) ;
#69019 = ORIENTED_EDGE ( 'NONE', *, *, #87170, .F. ) ;
#69018 = CARTESIAN_POINT ( 'NONE',  ( 17.84191302092929021, 11.53353326677314961, 11.49999999999999645 ) ) ;
#69020 = B_SPLINE_CURVE_WITH_KNOTS ( 'NONE', 3,
 ( #4090, #88831, #19299, #20286 ),
 .UNSPECIFIED., .F., .F.,
 ( 4, 4 ),
 ( 0.000000000000000000, 0.0001000000000000167422 ),
 .UNSPECIFIED. ) ;
#69021 = EDGE_LOOP ( 'NONE', ( #91021, #20939, #87385 ) ) ;
#69022 = CARTESIAN_POINT ( 'NONE',  ( 4.129723114849880083, -21.82631191821171512, 11.49999999999998934 ) ) ;
#69023 = CARTESIAN_POINT ( 'NONE',  ( -15.36756058500021282, 13.76162614515376426, 11.49999999999998934 ) ) ;
#69024 = VERTEX_POINT ( 'NONE', #73744 ) ;
#69025 = ORIENTED_EDGE ( 'NONE', *, *, #88517, .F. ) ;
#69026 = CARTESIAN_POINT ( 'NONE',  ( -109.8219511710470897, -25.31627459236276323, 5.738454807850723149 ) ) ;
#69027 = CARTESIAN_POINT ( 'NONE',  ( -40.34542624296162927, -25.12112790398598605, 2.835882484633130307 ) ) ;
#69028 = ORIENTED_EDGE ( 'NONE', *, *, #21559, .F. ) ;
#69029 = DIRECTION ( 'NONE',  ( 0.000000000000000000, 0.000000000000000000, 1.000000000000000000 ) ) ;
#69030 = VERTEX_POINT ( 'NONE', #3258 ) ;
#69031 = CARTESIAN_POINT ( 'NONE',  ( -89.40841769935767047, -25.22391154813773895, 6.409327647370974823 ) ) ;
#69032 = CARTESIAN_POINT ( 'NONE',  ( -35.55620429048339304, -23.48786465467240347, 11.44779295918255180 ) ) ;
#69033 = CARTESIAN_POINT ( 'NONE',  ( 14.06386034339543478, -15.33156129944631729, -1.500000000000002220 ) ) ;
#69034 = CARTESIAN_POINT ( 'NONE',  ( 10.97640485992876691, 18.82695874702771377, 11.49999999999999645 ) ) ;
#69035 = CARTESIAN_POINT ( 'NONE',  ( -40.81961785418572930, -25.31583757272871082, 5.018035748688583375 ) ) ;
#69036 = DIRECTION ( 'NONE',  ( 0.000000000000000000, -1.000000000000000000, 0.000000000000000000 ) ) ;
#69037 = CARTESIAN_POINT ( 'NONE',  ( -8.346146134265904237, -20.86121191590761015, -1.500000000000002220 ) ) ;
#69038 = VECTOR ( 'NONE', #53761, 1000.000000000000000 ) ;
#69039 = CARTESIAN_POINT ( 'NONE',  ( -38.52287095715006870, -23.47593901973090169, -1.443836447538997092 ) ) ;
#69040 = VERTEX_POINT ( 'NONE', #18954 ) ;
#69041 = CARTESIAN_POINT ( 'NONE',  ( 11.62916340711181284, -5.965225279485572685, 28.75961759920349792 ) ) ;
#69042 = CARTESIAN_POINT ( 'NONE',  ( -101.5468792378191978, -25.24282061761980955, 6.236250683194342059 ) ) ;
#69043 = EDGE_CURVE ( 'NONE', #70639, #35626, #47106, .T. ) ;
#69044 = ORIENTED_EDGE ( 'NONE', *, *, #17015, .F. ) ;
#69045 = ORIENTED_EDGE ( 'NONE', *, *, #39711, .T. ) ;
#69046 = ORIENTED_EDGE ( 'NONE', *, *, #8362, .F. ) ;
#69047 = CIRCLE ( 'NONE', #22022, 2.350000000000000089 ) ;
#69048 = CARTESIAN_POINT ( 'NONE',  ( -15.71168838272081558, 14.50144224353281786, -1.500000000000002220 ) ) ;
#69049 = EDGE_LOOP ( 'NONE', ( #72900, #41215, #87817, #89430 ) ) ;
#69050 = AXIS2_PLACEMENT_3D ( 'NONE', #92252, #55721, #38970 ) ;
#69051 = CARTESIAN_POINT ( 'NONE',  ( -14.96386864383857329, 14.77685607883014640, -1.500000000000002220 ) ) ;
#69052 = CARTESIAN_POINT ( 'NONE',  ( -30.46621203179166670, -25.14181536550043461, 2.712646531854225440 ) ) ;
#69053 = CARTESIAN_POINT ( 'NONE',  ( -110.4037686302767867, -25.19528510359861073, 3.295747964419194709 ) ) ;
#69054 = AXIS2_PLACEMENT_3D ( 'NONE', #41156, #57396, #72109 ) ;
#69055 = CARTESIAN_POINT ( 'NONE',  ( 2.903846153846159517, -5.876774720514415407, 19.99999999999999289 ) ) ;
#69056 = CARTESIAN_POINT ( 'NONE',  ( 20.22059317821533853, 8.664326447042464352, -1.500000000000002220 ) ) ;
#69057 = CARTESIAN_POINT ( 'NONE',  ( 29.73860345376319358, -5.356774720514427379, 1.647607965253214957 ) ) ;
#69058 = VERTEX_POINT ( 'NONE', #12831 ) ;
#69059 = CARTESIAN_POINT ( 'NONE',  ( -30.64427850938831099, -23.56000036390796382, 11.50200000000000067 ) ) ;
#69060 = AXIS2_PLACEMENT_3D ( 'NONE', #38628, #68586, #7173 ) ;
#69061 = DIRECTION ( 'NONE',  ( 0.000000000000000000, -1.000000000000000000, 0.000000000000000000 ) ) ;
#69062 = EDGE_CURVE ( 'NONE', #42104, #8769, #81859, .T. ) ;
#69063 = CARTESIAN_POINT ( 'NONE',  ( -84.63607584393763261, -23.96169478059713498, 10.65365249895717881 ) ) ;
#69064 = CARTESIAN_POINT ( 'NONE',  ( -127.5228709571500616, -23.47596703998600631, 11.44779298504227683 ) ) ;
#69065 = CARTESIAN_POINT ( 'NONE',  ( -0.05081623857416547180, -22.39214385819346376, 8.640809912072077381 ) ) ;
#69066 = CARTESIAN_POINT ( 'NONE',  ( 20.09692647535021948, 7.048664716645152595, 11.49999999999998934 ) ) ;
#69067 = CARTESIAN_POINT ( 'NONE',  ( -29.62287095715004881, -24.57400415421967566, 8.947790463233827651 ) ) ;
#69068 = CARTESIAN_POINT ( 'NONE',  ( -27.61766922344000363, -24.97064402808534567, 2.278554500308590303 ) ) ;
#69069 = EDGE_CURVE ( 'NONE', #67077, #75528, #65168, .T. ) ;
#69070 = CARTESIAN_POINT ( 'NONE',  ( -122.5562042904834072, -24.65952944569305316, 1.056160979905704789 ) ) ;
#69071 = CARTESIAN_POINT ( 'NONE',  ( -85.62287095715005592, -23.47596703998600631, 11.44779298504227860 ) ) ;
#69072 = CARTESIAN_POINT ( 'NONE',  ( -16.74547196562220464, 15.07928529822544661, -1.500000000000002220 ) ) ;
#69073 = CARTESIAN_POINT ( 'NONE',  ( -109.9079352936591931, -25.32390614315827193, 4.358500768180118889 ) ) ;
#69074 = VERTEX_POINT ( 'NONE', #49430 ) ;
#69075 = CARTESIAN_POINT ( 'NONE',  ( 0.000000000000000000, -5.876774720514426953, 0.000000000000000000 ) ) ;
#69076 = CARTESIAN_POINT ( 'NONE',  ( 6.560884470684795744, 18.50665934316380756, 11.49999999999999645 ) ) ;
#69077 = CARTESIAN_POINT ( 'NONE',  ( -81.62287095715005592, -29.50247984919015209, -1.443849546365053582 ) ) ;
#69078 = CARTESIAN_POINT ( 'NONE',  ( -100.6228709571500701, -24.91570333823099759, 8.075032458375556388 ) ) ;
#69079 = VERTEX_POINT ( 'NONE', #58531 ) ;
#69080 = CARTESIAN_POINT ( 'NONE',  ( -69.38891176720768783, -25.30450784505188011, 5.175863248522402316 ) ) ;
#69081 = CARTESIAN_POINT ( 'NONE',  ( -84.55620429048339304, -23.47593901973091235, -1.443836447539004642 ) ) ;
#69082 = VECTOR ( 'NONE', #13032, 1000.000000000000227 ) ;
#69083 = CARTESIAN_POINT ( 'NONE',  ( -0.6023826358649750912, 19.72334862104828090, -1.500000000000002220 ) ) ;
#69084 = B_SPLINE_CURVE_WITH_KNOTS ( 'NONE', 3,
 ( #68224, #60124, #27668, #43888 ),
 .UNSPECIFIED., .F., .F.,
 ( 4, 4 ),
 ( 0.000000000000000000, 9.999999999998897304E-05 ),
 .UNSPECIFIED. ) ;
#69085 = ORIENTED_EDGE ( 'NONE', *, *, #1726, .T. ) ;
#69086 = CARTESIAN_POINT ( 'NONE',  ( 11.32485880260453293, 6.376774720514427841, -25.00877359051251148 ) ) ;
#69087 = DIRECTION ( 'NONE',  ( 0.000000000000000000, -2.173523156925979552E-06, 0.9999999999976378895 ) ) ;
#69088 = APPLICATION_PROTOCOL_DEFINITION ( 'international standard', 'config_control_design', 1994, #68626 ) ;
#69089 = EDGE_LOOP ( 'NONE', ( #65703, #55054, #4508, #66581 ) ) ;
#69090 = CARTESIAN_POINT ( 'NONE',  ( -124.5228709571500616, -24.50321055353805733, 9.387540953477520489 ) ) ;
#69091 = DIRECTION ( 'NONE',  ( -1.000000000000000000, 0.000000000000000000, 0.000000000000000000 ) ) ;
#69092 = DIRECTION ( 'NONE',  ( 0.000000000000000000, 1.000000000000000000, 0.000000000000000000 ) ) ;
#69093 = DIRECTION ( 'NONE',  ( -3.773278334453079030E-23, 0.9999999999976377785, 2.173523156925979128E-06 ) ) ;
#69094 = DIRECTION ( 'NONE',  ( 0.000000000000000000, 0.9967269304714136968, 0.08084198211964954695 ) ) ;
#69095 = CARTESIAN_POINT ( 'NONE',  ( -67.55620429048340725, -24.64965694238574656, 8.947790433994198267 ) ) ;
#69096 = CARTESIAN_POINT ( 'NONE',  ( 0.3910256410256441884, -5.876774720514426953, 21.75000000000000000 ) ) ;
#69097 = CARTESIAN_POINT ( 'NONE',  ( -19.61284664649099696, 3.773188449817356904, 11.49999999999998934 ) ) ;
#69098 = CARTESIAN_POINT ( 'NONE',  ( -100.2631815169052203, -25.27532862745151121, 2.837685666037238708 ) ) ;
#69099 = CARTESIAN_POINT ( 'NONE',  ( -45.53465330854339044, -24.63419186844611630, 9.035850630976932862 ) ) ;
#69100 = ORIENTED_EDGE ( 'NONE', *, *, #93583, .F. ) ;
#69101 = AXIS2_PLACEMENT_3D ( 'NONE', #61241, #92163, #76925 ) ;
#69102 = B_SPLINE_CURVE_WITH_KNOTS ( 'NONE', 3,
 ( #89307, #26905, #81695, #22138 ),
 .UNSPECIFIED., .F., .F.,
 ( 4, 4 ),
 ( 0.9711935055097813407, 0.9801999367818968745 ),
 .UNSPECIFIED. ) ;
#69103 = DIRECTION ( 'NONE',  ( -0.6599726524652340665, -3.117967031984456719E-15, 0.7512896232465900992 ) ) ;
#69104 = CARTESIAN_POINT ( 'NONE',  ( -80.54796053850395765, -24.40133493613049964, 9.663955038902802386 ) ) ;
#69105 = FACE_OUTER_BOUND ( 'NONE', #1002, .T. ) ;
#69106 = DIRECTION ( 'NONE',  ( 0.1827036106964188000, -3.614007241618350743E-15, -0.9831680378442393398 ) ) ;
#69107 = CARTESIAN_POINT ( 'NONE',  ( -71.62287095715005592, -24.64898659630528854, 1.056161002820824368 ) ) ;
#69108 = CARTESIAN_POINT ( 'NONE',  ( -1.409217194013772101, -6.376774720514417183, 20.11414146978959749 ) ) ;
#69109 = CARTESIAN_POINT ( 'NONE',  ( -37.62287095715004170, -23.95044443724991368, 10.65354141964649237 ) ) ;
#69111 = VECTOR ( 'NONE', #37835, 1000.000000000000114 ) ;
#69110 = DIRECTION ( 'NONE',  ( -3.773278334453079030E-23, 0.9999999999976377785, 2.173523156925979128E-06 ) ) ;
#69112 = ORIENTED_EDGE ( 'NONE', *, *, #65627, .T. ) ;
#69113 = ADVANCED_FACE ( 'NONE', ( #67153 ), #18458, .F. ) ;
#69114 = VECTOR ( 'NONE', #54938, 999.9999999999998863 ) ;
#69115 = CARTESIAN_POINT ( 'NONE',  ( 2.300710779914242110, 20.15441874099239783, 11.49999999999998934 ) ) ;
#69116 = B_SPLINE_CURVE_WITH_KNOTS ( 'NONE', 3,
 ( #9880, #72794, #74282, #43835, #59569, #4279, #20482, #88514, #11880, #18990, #57579, #90009, #66199, #90501, #74768 ),
 .UNSPECIFIED., .F., .F.,
 ( 4, 1, 1, 1, 1, 1, 1, 1, 1, 1, 1, 1, 4 ),
 ( 0.000000000000000000, 0.1128134007444584058, 0.2253938839207300371, 0.3395948145627014636, 0.4596754102248630236, 0.5217351900879338977, 0.5839258387389175686, 0.6481741447653697197, 0.7138810381130681337, 0.7810044549073911213, 0.8514509275565554924, 0.9240506926641786078, 1.000000000000000000 ),
 .UNSPECIFIED. ) ;
#69117 = CARTESIAN_POINT ( 'NONE',  ( -76.62287095715005592, -23.96177878511308990, 10.65340807706330395 ) ) ;
#69118 = LINE ( 'NONE', #45792, #3141 ) ;
#69119 = ADVANCED_FACE ( 'NONE', ( #80864 ), #49934, .T. ) ;
#69120 = VECTOR ( 'NONE', #51352, 1000.000000000000114 ) ;
#69121 = CARTESIAN_POINT ( 'NONE',  ( -90.52287095715003318, -24.51163499207180507, 0.6490370598555487147 ) ) ;
#69122 = ADVANCED_FACE ( 'NONE', ( #65663 ), #60455, .F. ) ;
#69123 = ORIENTED_EDGE ( 'NONE', *, *, #15883, .F. ) ;
#69124 = FACE_OUTER_BOUND ( 'NONE', #43989, .T. ) ;
#69125 = CARTESIAN_POINT ( 'NONE',  ( 14.11618873683251252, 14.29484301466228047, -1.500000000000002220 ) ) ;
#69126 = ADVANCED_FACE ( 'NONE', ( #34692 ), #96579, .F. ) ;
#69127 = CARTESIAN_POINT ( 'NONE',  ( 9.758084087097168791, -18.66043984184860349, 11.49999999999999645 ) ) ;
#69128 = CARTESIAN_POINT ( 'NONE',  ( -64.52287095715010423, -24.66019654487200441, 8.947790411086119278 ) ) ;
#69129 = CARTESIAN_POINT ( 'NONE',  ( 6.025212951983072607, -21.27585971943098642, 11.49999999999998934 ) ) ;
#69130 = EDGE_CURVE ( 'NONE', #18512, #63950, #90626, .T. ) ;
#69131 = CARTESIAN_POINT ( 'NONE',  ( 15.21836549854886123, 13.79734045396011943, 11.49999999999998934 ) ) ;
#69132 = FACE_OUTER_BOUND ( 'NONE', #32674, .T. ) ;
#69133 = CARTESIAN_POINT ( 'NONE',  ( -126.6228709571500559, -23.72747288104470798, -1.053458166803224794 ) ) ;
#69134 = ORIENTED_EDGE ( 'NONE', *, *, #26470, .T. ) ;
#69135 = CARTESIAN_POINT ( 'NONE',  ( -87.52287095715006160, -29.50250243563736774, 8.947779886222139822 ) ) ;
#69136 = VERTEX_POINT ( 'NONE', #41816 ) ;
#69137 = CARTESIAN_POINT ( 'NONE',  ( -6.020540257910568904, -6.376774720514411854, 19.49847411603315095 ) ) ;
#69138 = CARTESIAN_POINT ( 'NONE',  ( -64.55620429048337883, -24.64965694238574301, 8.947790433994201820 ) ) ;
#69139 = ORIENTED_EDGE ( 'NONE', *, *, #6710, .F. ) ;
#69140 = VERTEX_POINT ( 'NONE', #20442 ) ;
#69141 = ORIENTED_EDGE ( 'NONE', *, *, #86313, .F. ) ;
#69142 = PLANE ( 'NONE',  #29183 ) ;
#69143 = DIRECTION ( 'NONE',  ( -0.000000000000000000, -1.000000000000000000, 0.000000000000000000 ) ) ;
#69145 = ADVANCED_FACE ( 'NONE', ( #97576 ), #58042, .F. ) ;
#69144 = LINE ( 'NONE', #54932, #9851 ) ;
#69146 = CARTESIAN_POINT ( 'NONE',  ( -13.08992234710881064, 15.94516925376868244, -1.500000000000002220 ) ) ;
#69147 = CARTESIAN_POINT ( 'NONE',  ( -16.79864850723062020, -13.61054813162024679, 11.49999999999999645 ) ) ;
#69148 = VERTEX_POINT ( 'NONE', #19450 ) ;
#69149 = LINE ( 'NONE', #38694, #85554 ) ;
#69150 = VECTOR ( 'NONE', #18372, 1000.000000000000000 ) ;
#69151 = CARTESIAN_POINT ( 'NONE',  ( -0.7638880233336636794, -9.374108182320437521, 9.000000000000000000 ) ) ;
#69152 = CARTESIAN_POINT ( 'NONE',  ( -18.60458529277170214, -12.42720982490441095, 11.49999999999998934 ) ) ;
#69153 = CARTESIAN_POINT ( 'NONE',  ( -93.52287095715007581, -23.94994826722565762, -0.6494450866342732498 ) ) ;
#69154 = CARTESIAN_POINT ( 'NONE',  ( -84.62620519360169169, -24.51314013834316441, 0.6176544820404183955 ) ) ;
#69155 = ORIENTED_EDGE ( 'NONE', *, *, #17492, .T. ) ;
#69156 = DIRECTION ( 'NONE',  ( 0.000000000000000000, 0.9999999999976377785, 2.173523156925979975E-06 ) ) ;
#69157 = CARTESIAN_POINT ( 'NONE',  ( -35.62660692631806114, -24.92592662359561118, 8.075495903017992916 ) ) ;
#69158 = CARTESIAN_POINT ( 'NONE',  ( -115.5228709571500616, -24.99132157543084531, 2.256160258750667502 ) ) ;
#69159 = VECTOR ( 'NONE', #56869, 1000.000000000000000 ) ;
#69160 = CARTESIAN_POINT ( 'NONE',  ( -18.75169668496848985, 9.291489096422434812, 11.49999999999998934 ) ) ;
#69161 = ORIENTED_EDGE ( 'NONE', *, *, #69471, .T. ) ;
#69162 = B_SPLINE_CURVE_WITH_KNOTS ( 'NONE', 3,
 ( #98142, #50493, #52492, #66239, #81445, #83420 ),
 .UNSPECIFIED., .F., .F.,
 ( 4, 2, 4 ),
 ( 0.000000000000000000, 0.001380764517854766050, 0.002761529035709532100 ),
 .UNSPECIFIED. ) ;
#69164 = ORIENTED_EDGE ( 'NONE', *, *, #44984, .T. ) ;
#69163 = CARTESIAN_POINT ( 'NONE',  ( -86.62608619482172401, -24.51314013834315375, 0.6176544820404177294 ) ) ;
#69165 = ORIENTED_EDGE ( 'NONE', *, *, #49336, .T. ) ;
#69166 = CARTESIAN_POINT ( 'NONE',  ( -109.6247146858308952, -24.51419770103157347, 9.386484678747171628 ) ) ;
#69167 = CARTESIAN_POINT ( 'NONE',  ( 21.18767802922067034, -0.7184367399587067160, -1.500000000000002220 ) ) ;
#69168 = ORIENTED_EDGE ( 'NONE', *, *, #42902, .T. ) ;
#69169 = CARTESIAN_POINT ( 'NONE',  ( -118.5228709571500758, -24.65952944569305316, 1.056160979905705899 ) ) ;
#69170 = CARTESIAN_POINT ( 'NONE',  ( -99.33919073176147663, -25.26221170829777307, 6.423374375703298611 ) ) ;
#69171 = CARTESIAN_POINT ( 'NONE',  ( 20.57308398666954119, -7.222494929537193187, 11.49999999999998934 ) ) ;
#69172 = CARTESIAN_POINT ( 'NONE',  ( -89.40841769935767047, -25.22391154813773895, 6.409327647370974823 ) ) ;
#69173 = CARTESIAN_POINT ( 'NONE',  ( -55.62287095715005592, -29.50250243563736774, 8.947779886222145151 ) ) ;
#69174 = CARTESIAN_POINT ( 'NONE',  ( 7.479587785762670471, -5.876774720514417183, 20.73799387832858088 ) ) ;
#69175 = CARTESIAN_POINT ( 'NONE',  ( 8.107222467604051630, 20.28165043084963060, -1.500000000000002220 ) ) ;
#69176 = CARTESIAN_POINT ( 'NONE',  ( -71.49027787591442973, -25.31639574635540058, 5.369049132701282367 ) ) ;
#69177 = VERTEX_POINT ( 'NONE', #35192 ) ;
#69178 = CARTESIAN_POINT ( 'NONE',  ( 26.29980976416808858, 5.126432557820720604, -7.297634155824876956 ) ) ;
#69179 = CYLINDRICAL_SURFACE ( 'NONE', #52408, 1.836000000000000743 ) ;
#69180 = EDGE_CURVE ( 'NONE', #88744, #33854, #36319, .T. ) ;
#69181 = VERTEX_POINT ( 'NONE', #77215 ) ;
#69182 = VECTOR ( 'NONE', #84666, 1000.000000000000000 ) ;
#69183 = VERTEX_POINT ( 'NONE', #44801 ) ;
#69184 = ORIENTED_EDGE ( 'NONE', *, *, #11907, .T. ) ;
#69185 = DIRECTION ( 'NONE',  ( 1.611864046919725738E-15, -7.253388211138766116E-15, 1.000000000000000000 ) ) ;
#69186 = CARTESIAN_POINT ( 'NONE',  ( 9.480266252741309074, -18.97159823121752709, -1.500000000000002220 ) ) ;
#69187 = DIRECTION ( 'NONE',  ( 1.000000000000000000, -0.000000000000000000, -0.000000000000000000 ) ) ;
#69188 = CARTESIAN_POINT ( 'NONE',  ( -130.5728709571500588, -24.13759587396042150, -0.5132947483565719615 ) ) ;
#69189 = CARTESIAN_POINT ( 'NONE',  ( 21.89392097122634340, -4.278466574096848163, -16.39911395417462003 ) ) ;
#69190 = CIRCLE ( 'NONE', #77286, 1.306876713926001354 ) ;
#69191 = CARTESIAN_POINT ( 'NONE',  ( 5.464387484610083057, -5.876774720514420736, 21.31215092858952431 ) ) ;
#69192 = CARTESIAN_POINT ( 'NONE',  ( -14.46832242630667942, -12.86894606327920876, -1.500000000000002220 ) ) ;
#69193 = EDGE_CURVE ( 'NONE', #71418, #22347, #21542, .T. ) ;
#69194 = CARTESIAN_POINT ( 'NONE',  ( -45.67376222244715933, -23.48783264082476663, -1.443836473390103237 ) ) ;
#69195 = VERTEX_POINT ( 'NONE', #7719 ) ;
#69196 = VECTOR ( 'NONE', #57956, 1000.000000000000114 ) ;
#69197 = CARTESIAN_POINT ( 'NONE',  ( -19.16120753946698585, -3.443109951913609024, 11.49999999999999645 ) ) ;
#69198 = DIRECTION ( 'NONE',  ( -3.773278334453079618E-23, 0.9999999999976377785, 2.173523156925979975E-06 ) ) ;
#69199 = VECTOR ( 'NONE', #43237, 1000.000000000000000 ) ;
#69200 = DIRECTION ( 'NONE',  ( 0.8243327689506978473, -1.230443507394594390E-06, 0.5661055431918692316 ) ) ;
#69201 = EDGE_CURVE ( 'NONE', #40087, #35826, #69118, .T. ) ;
#69202 = ORIENTED_EDGE ( 'NONE', *, *, #82531, .T. ) ;
#69203 = CARTESIAN_POINT ( 'NONE',  ( -78.58953762381672448, -23.47596703998600276, 11.44779298504227683 ) ) ;
#69204 = CARTESIAN_POINT ( 'NONE',  ( -59.52287095715006160, -23.48786465467241769, 11.44779295918254824 ) ) ;
#69205 = B_SPLINE_CURVE_WITH_KNOTS ( 'NONE', 3,
 ( #89578, #28179, #13936, #66265 ),
 .UNSPECIFIED., .F., .F.,
 ( 4, 4 ),
 ( 0.000000000000000000, 9.999999999998898659E-05 ),
 .UNSPECIFIED. ) ;
#69206 = CARTESIAN_POINT ( 'NONE',  ( -61.64687923781919920, -29.50248939449842922, 2.947779886236309377 ) ) ;
#69207 = CARTESIAN_POINT ( 'NONE',  ( -93.59418282098891950, -23.96169478059713498, 10.65365249895717170 ) ) ;
#69208 = CARTESIAN_POINT ( 'NONE',  ( 19.58216393897113505, 1.562425146961006650, -1.500000000000002220 ) ) ;
#69209 = DIRECTION ( 'NONE',  ( 0.000000000000000000, 1.000000000000000000, 0.000000000000000000 ) ) ;
#69210 = ORIENTED_EDGE ( 'NONE', *, *, #15917, .T. ) ;
#69211 = CARTESIAN_POINT ( 'NONE',  ( 2.580163054138214562, 21.43444414123800712, 11.49999999999998934 ) ) ;
#69212 = CARTESIAN_POINT ( 'NONE',  ( -95.52287095715007581, -24.63345952396256067, 9.038047939301502964 ) ) ;
#69213 = CARTESIAN_POINT ( 'NONE',  ( -40.63310824160917889, -24.73486907724916861, 1.287355809206965240 ) ) ;
#69214 = CARTESIAN_POINT ( 'NONE',  ( -90.52287095715003318, -25.00182538069145366, 7.747789668545104647 ) ) ;
#69215 = CARTESIAN_POINT ( 'NONE',  ( -6.685540227124203483, -22.02754839873749404, -1.500000000000002220 ) ) ;
#69216 = APPROVAL ( #45531, 'UNKNOWN' ) ;
#69217 = CALENDAR_DATE ( 2026, 9, 10 ) ;
#69218 = CARTESIAN_POINT ( 'NONE',  ( -93.59740075403963999, -23.73766607897670511, -1.055555164236453791 ) ) ;
#69219 = PLANE ( 'NONE',  #87986 ) ;
#69220 = CARTESIAN_POINT ( 'NONE',  ( -2.107266074560359748, -20.09985696230311447, 11.49999999999999645 ) ) ;
#69221 = CARTESIAN_POINT ( 'NONE',  ( -33.52287095715006160, -23.48786465467240347, 11.44779295918255357 ) ) ;
#69222 = DIRECTION ( 'NONE',  ( 0.000000000000000000, 0.000000000000000000, -1.000000000000000000 ) ) ;
#69223 =( BOUNDED_SURFACE ( )  B_SPLINE_SURFACE ( 3, 2, ( 
 ( #18079, #79975, #82961 ),
 ( #89591, #43918, #60157 ),
 ( #67266, #28192, #36804 ),
 ( #67765, #4854, #36307 ),
 ( #13450, #29683, #97199 ),
 ( #13949, #20072, #75848 ),
 ( #11960, #51035, #59653 ),
 ( #28689, #20565, #37305 ),
 ( #43429, #91080, #81978 ),
 ( #90584, #44926, #27698 ),
 ( #29182, #35806, #98687 ),
 ( #59149, #12460, #6346 ) ),
 .UNSPECIFIED., .F., .F., .T. ) 
 B_SPLINE_SURFACE_WITH_KNOTS ( ( 4, 2, 2, 2, 2, 4 ),
 ( 3, 3 ),
 ( 5.963111948670274387E-19, 0.0004805055694112242209, 0.0007207583541168360603, 0.0009610111388224478997, 0.001441516708233671470, 0.001922022277644895149 ),
 ( 0.000000000000000000, 1.000000000000000000 ),
 .UNSPECIFIED. ) 
 GEOMETRIC_REPRESENTATION_ITEM ( )  RATIONAL_B_SPLINE_SURFACE ( (
 ( 1.000000000000000000, 0.6532382444175209857, 1.000000000000000000),
 ( 1.000000000000000000, 0.6532227097440629349, 1.000000000000000000),
 ( 1.000000000000000000, 0.6547852517831300734, 1.000000000000000000),
 ( 1.000000000000000000, 0.6591574828660964336, 1.000000000000000000),
 ( 1.000000000000000000, 0.6609310395923762016, 1.000000000000000000),
 ( 1.000000000000000000, 0.6650742797340818413, 1.000000000000000000),
 ( 1.000000000000000000, 0.6674600455423553846, 1.000000000000000000),
 ( 1.000000000000000000, 0.6751670852230186037, 1.000000000000000000),
 ( 1.000000000000000000, 0.6812390391297645786, 1.000000000000000000),
 ( 1.000000000000000000, 0.6938890553660238547, 1.000000000000000000),
 ( 1.000000000000000000, 0.7006220437376451393, 1.000000000000000000),
 ( 1.000000000000000000, 0.7071067811865475727, 1.000000000000000000) ) ) 
 REPRESENTATION_ITEM ( '' )  SURFACE ( )  );
#69224 = CARTESIAN_POINT ( 'NONE',  ( -110.3641915914744800, -25.10921374192945166, 2.833513679721968881 ) ) ;
#69225 = CARTESIAN_POINT ( 'NONE',  ( -126.6228709571500843, -23.47596703998600631, 11.44779298504227860 ) ) ;
#69226 = CARTESIAN_POINT ( 'NONE',  ( -111.2332490450528582, -25.29779265843440328, 3.802241964366937399 ) ) ;
#69227 = CARTESIAN_POINT ( 'NONE',  ( 4.721227339208565965, -19.33841413273825793, 11.49999999999998934 ) ) ;
#69228 = DIRECTION ( 'NONE',  ( 0.000000000000000000, 0.000000000000000000, -1.000000000000000000 ) ) ;
#69229 = CARTESIAN_POINT ( 'NONE',  ( 18.24360591643979035, -7.691401616277519615, -1.500000000000002220 ) ) ;
#69230 = VECTOR ( 'NONE', #61583, 1000.000000000000114 ) ;
#69231 = CARTESIAN_POINT ( 'NONE',  ( -56.61227192276419373, -23.48783264082477018, -1.443836473390095909 ) ) ;
#69232 = CARTESIAN_POINT ( 'NONE',  ( -40.37522208020789805, -25.10925592908469284, 2.834757886433481033 ) ) ;
#69233 = CARTESIAN_POINT ( 'NONE',  ( 22.02124265030973760, -4.543225279485573864, 16.20402280011862217 ) ) ;
#69234 = CARTESIAN_POINT ( 'NONE',  ( -19.01758589260300525, -8.224767016273846210, 11.49999999999999645 ) ) ;
#69235 = CIRCLE ( 'NONE', #20634, 129.7684398600581517 ) ;
#69236 = CARTESIAN_POINT ( 'NONE',  ( -115.5228709571500616, -29.50250786944525672, 11.44777988621622811 ) ) ;
#69237 = CARTESIAN_POINT ( 'NONE',  ( -49.95596087352405590, -25.31439292586784262, 5.268391321001662853 ) ) ;
#69238 = CARTESIAN_POINT ( 'NONE',  ( -12.51292883401962541, 18.98408452820241266, 11.49999999999999645 ) ) ;
#69239 = EDGE_LOOP ( 'NONE', ( #69481, #95652, #53926, #61792 ) ) ;
#69240 = B_SPLINE_SURFACE_WITH_KNOTS ( 'NONE', 3, 3, ( 
 ( #79027, #41486, #79536, #88661 ),
 ( #40483, #17134, #19130, #32871 ),
 ( #50102, #11520, #34869, #73435 ),
 ( #25247, #3932, #64346, #95762 ),
 ( #2425, #63844, #96762, #40985 ),
 ( #49108, #56220, #33358, #25754 ),
 ( #27261, #86648, #87150, #95264 ) ),
 .UNSPECIFIED., .F., .F., .F.,
 ( 4, 3, 4 ),
 ( 4, 4 ),
 ( 0.0004766839783819443524, 0.1029713700210896227, 0.2054660560637973088 ),
 ( 0.2695625693603935225, 0.2706996695906280781 ),
 .UNSPECIFIED. ) ;
#69241 = DIRECTION ( 'NONE',  ( -1.000000000000000000, -3.773278334444167608E-23, -8.201307833595939069E-29 ) ) ;
#69242 = DIRECTION ( 'NONE',  ( -3.773278334453079618E-23, 0.9999999999976377785, 2.173523156925978705E-06 ) ) ;
#69243 = B_SPLINE_CURVE_WITH_KNOTS ( 'NONE', 3,
 ( #13796, #69090, #53881, #582, #84813, #75695 ),
 .UNSPECIFIED., .F., .F.,
 ( 4, 2, 4 ),
 ( 0.000000000000000000, 0.001380901958385394833, 0.002761803916770789666 ),
 .UNSPECIFIED. ) ;
#69244 = CARTESIAN_POINT ( 'NONE',  ( 12.02422309597069017, 16.21794576832014556, -1.500000000000002220 ) ) ;
#69245 = CARTESIAN_POINT ( 'NONE',  ( -114.6228709571500559, -29.50247984919015209, -1.443849546365048253 ) ) ;
#69246 = DIRECTION ( 'NONE',  ( 3.773278334444166432E-23, -1.000000000000000000, 0.000000000000000000 ) ) ;
#69247 = ORIENTED_EDGE ( 'NONE', *, *, #67671, .F. ) ;
#69248 = VECTOR ( 'NONE', #63227, 1000.000000000000000 ) ;
#69249 = VERTEX_POINT ( 'NONE', #99056 ) ;
#69250 = DIRECTION ( 'NONE',  ( -3.773278334444167608E-23, 1.000000000000000000, 0.000000000000000000 ) ) ;
#69251 = CARTESIAN_POINT ( 'NONE',  ( 16.30191990219073972, -16.09819076282585826, -1.500000000000002220 ) ) ;
#69252 = CARTESIAN_POINT ( 'NONE',  ( -51.10270014058699672, -25.27420619311879335, 3.552653933812367715 ) ) ;
#69253 = CARTESIAN_POINT ( 'NONE',  ( -12.93760099376155104, 17.33828479246177423, -1.500000000000002220 ) ) ;
#69254 = CARTESIAN_POINT ( 'NONE',  ( -123.6248516269914859, -24.15543982623907482, -0.2315651400026560169 ) ) ;
#69255 = CARTESIAN_POINT ( 'NONE',  ( -34.54553770641572896, -24.15543982623907127, -0.2315651400026575435 ) ) ;
#69256 = ADVANCED_FACE ( 'NONE', ( #46287 ), #29557, .T. ) ;
#69257 = CARTESIAN_POINT ( 'NONE',  ( -20.86263692406621928, 1.606387762444034362, 11.49999999999999645 ) ) ;
#69258 = ORIENTED_EDGE ( 'NONE', *, *, #30062, .T. ) ;
#69259 = CARTESIAN_POINT ( 'NONE',  ( -115.5228709571500616, -23.47596703998600631, 11.44779298504227860 ) ) ;
#69260 = CARTESIAN_POINT ( 'NONE',  ( -0.4018715335629812202, -22.01094342083549193, 11.49999999999998934 ) ) ;
#69261 = ADVANCED_FACE ( 'NONE', ( #83844 ), #99549, .F. ) ;
#69262 = VECTOR ( 'NONE', #41460, 1000.000000000000114 ) ;
#69263 = DIRECTION ( 'NONE',  ( 0.7512896232465892110, -0.000000000000000000, 0.6599726524652350657 ) ) ;
#69264 = CARTESIAN_POINT ( 'NONE',  ( -40.43756433397305727, -25.10925768246707435, 2.832404819642281524 ) ) ;
#69265 = ORIENTED_EDGE ( 'NONE', *, *, #75310, .T. ) ;
#69266 = DIRECTION ( 'NONE',  ( 0.000000000000000000, 1.000000000000000000, 0.000000000000000000 ) ) ;
#69267 = DIRECTION ( 'NONE',  ( 0.8219392559241307517, 0.5637660281018075370, 0.08114015731558725519 ) ) ;
#69268 = VERTEX_POINT ( 'NONE', #51915 ) ;
#69269 = CARTESIAN_POINT ( 'NONE',  ( -72.62691082383823016, -24.51419770103156281, 9.386484678747185839 ) ) ;
#69270 = ORIENTED_EDGE ( 'NONE', *, *, #83381, .F. ) ;
#69271 = VECTOR ( 'NONE', #4310, 1000.000000000000000 ) ;
#69272 = VERTEX_POINT ( 'NONE', #21929 ) ;
#69273 = CARTESIAN_POINT ( 'NONE',  ( -71.51636059175528715, -23.73791477778911840, 11.05961554403170766 ) ) ;
#69274 = DIRECTION ( 'NONE',  ( 0.000000000000000000, 0.000000000000000000, 1.000000000000000000 ) ) ;
#69276 = EDGE_CURVE ( 'NONE', #59593, #81901, #91955, .T. ) ;
#69275 = CARTESIAN_POINT ( 'NONE',  ( -61.62287095715004881, -23.48783264082478439, -1.443836473390069042 ) ) ;
#69277 = CARTESIAN_POINT ( 'NONE',  ( 5.889875310795558150, 19.62242631308348706, -1.500000000000002220 ) ) ;
#69278 = EDGE_LOOP ( 'NONE', ( #43202, #7649, #59198, #60183 ) ) ;
#69279 = CARTESIAN_POINT ( 'NONE',  ( -2.369893591381136755, -5.876774720514409189, 19.15221817653405623 ) ) ;
#69280 = CARTESIAN_POINT ( 'NONE',  ( -44.48768996415131483, -24.51314013834316086, 0.6176544820404110681 ) ) ;
#69281 = CARTESIAN_POINT ( 'NONE',  ( -124.5228709571500616, -29.50250243563736774, 8.947779886222134493 ) ) ;
#69282 = CARTESIAN_POINT ( 'NONE',  ( 15.07672925556244969, 16.42598562245719407, -1.500000000000002220 ) ) ;
#69283 = DIRECTION ( 'NONE',  ( -3.773278334453079030E-23, 0.9999999999976377785, 2.173523156925979128E-06 ) ) ;
#69284 = CARTESIAN_POINT ( 'NONE',  ( -28.55620429048338949, -24.49160925498320296, 8.947790452558288976 ) ) ;
#69285 = ORIENTED_EDGE ( 'NONE', *, *, #49034, .F. ) ;
#69286 = B_SPLINE_CURVE_WITH_KNOTS ( 'NONE', 3,
 ( #38235, #73943, #99131, #4440, #43001, #69191, #52982, #77287, #30624, #29630, #60605, #35390, #83411, #22000, #53982 ),
 .UNSPECIFIED., .F., .F.,
 ( 4, 1, 1, 1, 1, 1, 1, 1, 1, 1, 1, 1, 4 ),
 ( 0.000000000000000000, 0.08594794314412859682, 0.1691252118806910454, 0.2503991071860492412, 0.3322897361388358339, 0.4133642879158805905, 0.4941722833711898466, 0.5760217353866382561, 0.6607569692540066209, 0.7457831259137440716, 0.8300435929752246755, 0.9140275458206831294, 1.000000000000000000 ),
 .UNSPECIFIED. ) ;
#69287 = CARTESIAN_POINT ( 'NONE',  ( -29.26673851950083716, -24.93593727437086471, 2.461460217553469665 ) ) ;
#69288 = CARTESIAN_POINT ( 'NONE',  ( -29.66400988275576367, -24.63645681146989119, 6.487136769355695165 ) ) ;
#69289 = CARTESIAN_POINT ( 'NONE',  ( -20.61801493038525379, 2.926015819835423581, -1.500000000000002220 ) ) ;
#69290 = VERTEX_POINT ( 'NONE', #75233 ) ;
#69292 = ORIENTED_EDGE ( 'NONE', *, *, #17447, .F. ) ;
#69291 = CARTESIAN_POINT ( 'NONE',  ( 4.639502537026700679, -6.376774720514415407, 19.60647575951318800 ) ) ;
#69293 = CARTESIAN_POINT ( 'NONE',  ( -50.56357725185049645, -25.25854568647407206, 7.098062045694851996 ) ) ;
#69294 = ORIENTED_EDGE ( 'NONE', *, *, #30413, .F. ) ;
#69295 = VERTEX_POINT ( 'NONE', #52911 ) ;
#69296 = CARTESIAN_POINT ( 'NONE',  ( -2.899999999999996358, 33.29999999999999716, 2.100000000000000089 ) ) ;
#69297 = CARTESIAN_POINT ( 'NONE',  ( -50.38191529551148307, -25.27412227713961457, 2.832404461305267240 ) ) ;
#69298 = CARTESIAN_POINT ( 'NONE',  ( -111.3758925029758871, -25.19402559689468646, 6.830252627919830566 ) ) ;
#69299 = CARTESIAN_POINT ( 'NONE',  ( -29.49875734969026198, -5.965225279485572685, 0.1180228001186258285 ) ) ;
#69300 = CARTESIAN_POINT ( 'NONE',  ( -109.7069964148890904, -25.14173549452716472, 2.952782056881928963 ) ) ;
#69301 = DIRECTION ( 'NONE',  ( 1.084136044942898696E-16, 0.000000000000000000, -1.000000000000000000 ) ) ;
#69303 = ORIENTED_EDGE ( 'NONE', *, *, #57370, .T. ) ;
#69302 = CARTESIAN_POINT ( 'NONE',  ( -15.83042281971428977, -15.45127431894796466, 11.49999999999999645 ) ) ;
#69304 = DIRECTION ( 'NONE',  ( -1.000000000000000000, -0.000000000000000000, -0.000000000000000000 ) ) ;
#69305 = ORIENTED_EDGE ( 'NONE', *, *, #6389, .T. ) ;
#69306 = CARTESIAN_POINT ( 'NONE',  ( 22.64978874513612439, 0.4204215919581203442, 11.49999999999998934 ) ) ;
#69307 = VECTOR ( 'NONE', #57846, 1000.000000000000000 ) ;
#69309 = EDGE_LOOP ( 'NONE', ( #98730, #87101, #65170, #85979 ) ) ;
#69308 = CARTESIAN_POINT ( 'NONE',  ( -27.75922577455652984, -24.80591230451047480, 7.602030938097199098 ) ) ;
#69310 = ADVANCED_FACE ( 'NONE', ( #6719 ), #36678, .F. ) ;
#69311 = ORIENTED_EDGE ( 'NONE', *, *, #52545, .T. ) ;
#69312 = CARTESIAN_POINT ( 'NONE',  ( -68.22287095715007865, -23.47596703998600631, 11.44779298504227860 ) ) ;
#69313 = EDGE_CURVE ( 'NONE', #43106, #26765, #82580, .T. ) ;
#69314 = CARTESIAN_POINT ( 'NONE',  ( -14.78635263257777233, 13.65558988533819473, -1.500000000000002220 ) ) ;
#69315 = DIRECTION ( 'NONE',  ( 0.000000000000000000, -2.173523156925980399E-06, 0.9999999999976378895 ) ) ;
#69316 = EDGE_LOOP ( 'NONE', ( #98045, #6412, #45748, #50003 ) ) ;
#69317 = FACE_OUTER_BOUND ( 'NONE', #29579, .T. ) ;
#69318 = CARTESIAN_POINT ( 'NONE',  ( -20.85237562250380350, -7.973873963886685345, -1.500000000000002220 ) ) ;
#69319 = ORIENTED_EDGE ( 'NONE', *, *, #60001, .T. ) ;
#69320 = VERTEX_POINT ( 'NONE', #68631 ) ;
#69321 = CARTESIAN_POINT ( 'NONE',  ( -101.3040450898205620, -25.25341214910569931, 6.746837293798033208 ) ) ;
#69322 = FACE_OUTER_BOUND ( 'NONE', #40358, .T. ) ;
#69323 = PLANE ( 'NONE',  #66876 ) ;
#69324 = DIRECTION ( 'NONE',  ( -0.09824042138329590335, 0.9951627101165078093, 3.519298150595267489E-15 ) ) ;
#69325 = AXIS2_PLACEMENT_3D ( 'NONE', #80075, #87186, #71477 ) ;
#69326 = FACE_OUTER_BOUND ( 'NONE', #72026, .T. ) ;
#69327 = CARTESIAN_POINT ( 'NONE',  ( 4.865394487973861537, 18.91859722749940786, 11.49999999999998934 ) ) ;
#69328 = DIRECTION ( 'NONE',  ( -1.000000000000000000, -3.773278334444167608E-23, -8.201307833595939069E-29 ) ) ;
#69329 = CARTESIAN_POINT ( 'NONE',  ( -8.581294335678165908, -19.67629172487136557, -1.500000000000002220 ) ) ;
#69330 = CARTESIAN_POINT ( 'NONE',  ( -2.532641601674031850, -5.876774720514408301, 19.55266968305501507 ) ) ;
#69331 = CARTESIAN_POINT ( 'NONE',  ( -46.58953762381671737, -23.47596703998600276, 11.44779298504227505 ) ) ;
#69332 = CARTESIAN_POINT ( 'NONE',  ( -59.62287095715004881, -23.48783264082478794, -1.443836473390069042 ) ) ;
#69333 = CARTESIAN_POINT ( 'NONE',  ( -80.62287095714998486, -24.51254535404255108, 9.355368623467654743 ) ) ;
#69334 = CARTESIAN_POINT ( 'NONE',  ( 2.723195454624489642, 22.67993996152103620, -1.500000000000002220 ) ) ;
#69335 = EDGE_CURVE ( 'NONE', #57212, #14292, #100374, .T. ) ;
#69336 = AXIS2_PLACEMENT_3D ( 'NONE', #11256, #42234, #3657 ) ;
#69337 = APPROVAL_STATUS ( 'not_yet_approved' ) ;
#69338 = CARTESIAN_POINT ( 'NONE',  ( -124.5228709571500616, -24.64965694238575722, 8.947790433994191162 ) ) ;
#69339 = DIRECTION ( 'NONE',  ( 0.000000000000000000, 0.9999999999976377785, 2.173523156925979975E-06 ) ) ;
#69340 = CARTESIAN_POINT ( 'NONE',  ( -6.099057486122481997, -19.05896565686126110, 11.49999999999999645 ) ) ;
#69341 = CARTESIAN_POINT ( 'NONE',  ( -79.34156256387794315, -25.26612463273757925, 4.917719406326733100 ) ) ;
#69342 = CARTESIAN_POINT ( 'NONE',  ( -111.5228709571500616, -23.47593901973090524, -1.443836447538996204 ) ) ;
#69343 = VECTOR ( 'NONE', #57377, 1000.000000000000114 ) ;
#69345 = B_SPLINE_CURVE_WITH_KNOTS ( 'NONE', 3,
 ( #36417, #43542, #13068, #51147, #35919, #44031 ),
 .UNSPECIFIED., .F., .F.,
 ( 4, 2, 4 ),
 ( 0.000000000000000000, 0.001380901958385387894, 0.002761803916770775788 ),
 .UNSPECIFIED. ) ;
#69344 = CARTESIAN_POINT ( 'NONE',  ( 4.642799911345256270, -5.876774720514408301, 18.59646607068888713 ) ) ;
#69346 = CARTESIAN_POINT ( 'NONE',  ( -108.6228709571500559, -24.64898659630368627, 1.056161002820831474 ) ) ;
#69347 = ORIENTED_EDGE ( 'NONE', *, *, #44090, .T. ) ;
#69348 = CARTESIAN_POINT ( 'NONE',  ( -83.52287095715006160, -23.48786465467241769, 11.44779295918254469 ) ) ;
#69349 = CARTESIAN_POINT ( 'NONE',  ( 14.76093561896379214, 6.475225279485574248, -26.55548769130089681 ) ) ;
#69350 = CARTESIAN_POINT ( 'NONE',  ( 21.56942612084361599, 2.798134137018522427, 11.49999999999998934 ) ) ;
#69351 = EDGE_CURVE ( 'NONE', #62329, #80499, #26433, .T. ) ;
#69352 = FACE_OUTER_BOUND ( 'NONE', #63728, .T. ) ;
#69353 = CARTESIAN_POINT ( 'NONE',  ( 0.9049686737998731134, -19.58615294826029540, -1.500000000000002220 ) ) ;
#69354 = CARTESIAN_POINT ( 'NONE',  ( 5.399550031316281640, -0.3587747205144061202, -28.54570968857217395 ) ) ;
#69355 = AXIS2_PLACEMENT_3D ( 'NONE', #53519, #84442, #7311 ) ;
#69356 = CARTESIAN_POINT ( 'NONE',  ( -40.70683750969132575, -25.18823549857387789, 3.317374228038964645 ) ) ;
#69357 = PERSON_AND_ORGANIZATION_ROLE ( 'classification_officer' ) ;
#69358 = CARTESIAN_POINT ( 'NONE',  ( -91.55173743107893358, -24.15620529776628445, 10.23563542870660292 ) ) ;
#69359 = DIRECTION ( 'NONE',  ( -3.773278334453079030E-23, 0.9999999999976377785, 2.173523156925979128E-06 ) ) ;
#69360 = CARTESIAN_POINT ( 'NONE',  ( -4.979992623568794130, 19.86841884474198494, 11.49999999999999645 ) ) ;
#69361 = PLANE ( 'NONE',  #76467 ) ;
#69362 = CARTESIAN_POINT ( 'NONE',  ( -46.52287095715004028, -24.66019654487199375, 8.947790411086122830 ) ) ;
#69363 = ORIENTED_EDGE ( 'NONE', *, *, #48646, .F. ) ;
#69364 = CARTESIAN_POINT ( 'NONE',  ( -100.0631793594960044, -25.31296428244992569, 4.632688900756619432 ) ) ;
#69365 = CARTESIAN_POINT ( 'NONE',  ( 8.749999999999769074, 18.74999999999999645, 0.000000000000000000 ) ) ;
#69366 = CARTESIAN_POINT ( 'NONE',  ( -125.5562614031464932, -23.85049219812686871, 10.88485053497526778 ) ) ;
#69367 = CARTESIAN_POINT ( 'NONE',  ( 14.98902733942698617, -3.496957042870280752, -27.33343847194423404 ) ) ;
#69368 = ADVANCED_FACE ( 'NONE', ( #7213 ), #38162, .T. ) ;
#69369 = EDGE_CURVE ( 'NONE', #8388, #56523, #92448, .T. ) ;
#69370 = CARTESIAN_POINT ( 'NONE',  ( -38.52287095715006870, -24.64965694238406613, 8.947790433994205372 ) ) ;
#69371 = CARTESIAN_POINT ( 'NONE',  ( 31.29611288755342002, 5.755914996345237178, -2.011851919325042370 ) ) ;
#69372 = CARTESIAN_POINT ( 'NONE',  ( 3.314627170985911420, 22.80399709308638023, 11.49999999999999645 ) ) ;
#69373 = CARTESIAN_POINT ( 'NONE',  ( -6.082769120682566921, -21.99330073093985405, 11.49999999999998934 ) ) ;
#69374 = CARTESIAN_POINT ( 'NONE',  ( -104.5228709571501184, -24.33832256527049154, 0.1851278514138610942 ) ) ;
#69375 = B_SPLINE_SURFACE_WITH_KNOTS ( 'NONE', 3, 3, ( 
 ( #87181, #24285, #1961, #25781 ),
 ( #10057, #63874, #17669, #56256 ),
 ( #40007, #39004, #70967, #48642 ),
 ( #71973, #1458, #41019, #78049 ),
 ( #24771, #2454, #8563, #56757 ),
 ( #69957, #55753, #442, #86680 ),
 ( #48133, #34899, #72468, #72969 ) ),
 .UNSPECIFIED., .F., .F., .F.,
 ( 4, 3, 4 ),
 ( 4, 4 ),
 ( 0.0004766839783817961962, 0.1029713700210893035, 0.2054660560637968092 ),
 ( 0.7896948821346888581, 0.7910719704583279999 ),
 .UNSPECIFIED. ) ;
#69376 = CARTESIAN_POINT ( 'NONE',  ( -75.52287095715007581, -23.84081130425355965, 10.88220057483160907 ) ) ;
#69377 = CARTESIAN_POINT ( 'NONE',  ( 6.499999999999992895, 2.573529411764703845, 1.544117647058822929 ) ) ;
#69378 = CARTESIAN_POINT ( 'NONE',  ( -17.93832129671990572, 13.47109510200611560, 11.49999999999999645 ) ) ;
#69379 = VERTEX_POINT ( 'NONE', #22916 ) ;
#69380 = FACE_OUTER_BOUND ( 'NONE', #93714, .T. ) ;
#69381 = CARTESIAN_POINT ( 'NONE',  ( -43.56913326832147959, -23.48783264082478084, -1.443836473390076369 ) ) ;
#69382 = CARTESIAN_POINT ( 'NONE',  ( -20.07106029494397248, -8.819774368769808248, -1.500000000000002220 ) ) ;
#69383 = ADVANCED_FACE ( 'NONE', ( #94962 ), #48300, .T. ) ;
#69384 = CARTESIAN_POINT ( 'NONE',  ( -113.5228709571500616, -23.96127896941632685, -0.6493128931037960294 ) ) ;
#69385 = CARTESIAN_POINT ( 'NONE',  ( -87.54530861272236564, -24.51419770103156281, 9.386484678747175181 ) ) ;
#69386 = CARTESIAN_POINT ( 'NONE',  ( -114.6228709571500559, -23.47593901973091235, -1.443836447538999312 ) ) ;
#69387 = ADVANCED_FACE ( 'NONE', ( #70125 ), #40181, .F. ) ;
#69388 = CARTESIAN_POINT ( 'NONE',  ( -49.21454750704995007, -25.12863070112381791, 7.069183623698430452 ) ) ;
#69389 = CARTESIAN_POINT ( 'NONE',  ( 0.000000000000000000, -4.056774720514426669, 6.000000000000000888 ) ) ;
#69390 = VERTEX_POINT ( 'NONE', #25451 ) ;
#69391 = CARTESIAN_POINT ( 'NONE',  ( -0.3173379506236611580, 20.48240526196808631, -1.500000000000002220 ) ) ;
#69392 = ORIENTED_EDGE ( 'NONE', *, *, #62222, .T. ) ;
#69393 = ORIENTED_EDGE ( 'NONE', *, *, #96172, .F. ) ;
#69394 = VERTEX_POINT ( 'NONE', #31558 ) ;
#69395 = EDGE_LOOP ( 'NONE', ( #29596, #36233 ) ) ;
#69396 = CARTESIAN_POINT ( 'NONE',  ( -21.10450430117995424, 9.351148110661185342, -1.500000000000002220 ) ) ;
#69398 = EDGE_CURVE ( 'NONE', #82785, #74711, #16707, .T. ) ;
#69397 = CARTESIAN_POINT ( 'NONE',  ( -102.5562042904833930, -24.66019654487199730, 8.947790411086122830 ) ) ;
#69399 = CARTESIAN_POINT ( 'NONE',  ( -15.58492919356500650, -12.95507736684500699, -1.500000000000002220 ) ) ;
#69400 = ORIENTED_EDGE ( 'NONE', *, *, #95147, .F. ) ;
#69401 = DIRECTION ( 'NONE',  ( 1.000000000000000000, -0.000000000000000000, -0.000000000000000000 ) ) ;
#69402 = AXIS2_PLACEMENT_3D ( 'NONE', #18194, #16305, #85823 ) ;
#69403 = DIRECTION ( 'NONE',  ( -1.000000000000000000, -0.000000000000000000, -0.000000000000000000 ) ) ;
#69404 = EDGE_CURVE ( 'NONE', #3899, #50986, #71170, .T. ) ;
#69405 = B_SPLINE_CURVE_WITH_KNOTS ( 'NONE', 3,
 ( #99390, #37500, #28888, #7547, #44120, #75048, #15155, #83163, #5544, #69450, #52729, #91286, #21756, #92277, #23258, #45619 ),
 .UNSPECIFIED., .F., .F.,
 ( 4, 2, 2, 2, 2, 2, 2, 4 ),
 ( 0.000000000000000000, 0.0004662014769087530121, 0.0009324029538175060243, 0.001398604430726259036, 0.001864805907635012049, 0.002331007384543765278, 0.002797208861452518073, 0.003729611815270027567 ),
 .UNSPECIFIED. ) ;
#69406 = CARTESIAN_POINT ( 'NONE',  ( -28.52287095715005449, -24.34211201941327474, 9.387659967996357935 ) ) ;
#69407 = CARTESIAN_POINT ( 'NONE',  ( -70.54094150479154735, -24.63355581998385091, 0.9682620441943861067 ) ) ;
#69409 = EDGE_LOOP ( 'NONE', ( #32993, #74637, #77594, #39182 ) ) ;
#69408 = CARTESIAN_POINT ( 'NONE',  ( 4.199879391047538491, -21.09745483596041282, 11.49999999999999645 ) ) ;
#69410 = CARTESIAN_POINT ( 'NONE',  ( -75.64173089025919694, -24.15503026093913874, -0.2815557561904522554 ) ) ;
#69411 = CARTESIAN_POINT ( 'NONE',  ( -61.49449328950704086, -24.51419770103157347, 9.386484678747178734 ) ) ;
#69412 = ORIENTED_EDGE ( 'NONE', *, *, #80061, .T. ) ;
#69413 = CARTESIAN_POINT ( 'NONE',  ( 10.87737074370964407, 17.65887017642603851, 11.49999999999998934 ) ) ;
#69414 = ORIENTED_EDGE ( 'NONE', *, *, #9691, .T. ) ;
#69416 = ORIENTED_EDGE ( 'NONE', *, *, #70022, .T. ) ;
#69415 = FACE_OUTER_BOUND ( 'NONE', #44575, .T. ) ;
#69417 = DIRECTION ( 'NONE',  ( 0.000000000000000000, 0.000000000000000000, -1.000000000000000000 ) ) ;
#69418 = EDGE_LOOP ( 'NONE', ( #83649, #24583, #7276, #32140 ) ) ;
#69419 = ORIENTED_EDGE ( 'NONE', *, *, #6710, .T. ) ;
#69420 = CARTESIAN_POINT ( 'NONE',  ( 4.959895098850171102, -5.876774720514410077, 19.67755022954121813 ) ) ;
#69421 = VECTOR ( 'NONE', #21304, 1000.000000000000114 ) ;
#69422 = CARTESIAN_POINT ( 'NONE',  ( -42.54639151317959289, -24.15620529776627734, 10.23563542870661358 ) ) ;
#69423 = CARTESIAN_POINT ( 'NONE',  ( -65.48373801871647970, -25.00158670708910691, 2.256160236439222366 ) ) ;
#69424 = CARTESIAN_POINT ( 'NONE',  ( -8.017166757594178961, 20.41873492177044724, 11.49999999999999645 ) ) ;
#69425 = LINE ( 'NONE', #62837, #13929 ) ;
#69426 = CARTESIAN_POINT ( 'NONE',  ( 8.566404662457630437, 20.85315857434707709, 11.49999999999998934 ) ) ;
#69427 = CARTESIAN_POINT ( 'NONE',  ( 8.737904895026865404, 19.08465823478955414, 11.49999999999998934 ) ) ;
#69428 = CARTESIAN_POINT ( 'NONE',  ( -89.62287095715005592, -23.72747288104470442, -1.053458166803225682 ) ) ;
#69429 = CARTESIAN_POINT ( 'NONE',  ( -100.6228709571500559, -29.50247984919015209, -1.443849546365050029 ) ) ;
#69430 = ORIENTED_EDGE ( 'NONE', *, *, #96031, .F. ) ;
#69431 = VECTOR ( 'NONE', #56027, 1000.000000000000000 ) ;
#69432 = ORIENTED_EDGE ( 'NONE', *, *, #9701, .F. ) ;
#69433 = ORIENTED_EDGE ( 'NONE', *, *, #34616, .T. ) ;
#69434 = CARTESIAN_POINT ( 'NONE',  ( -80.62287095715005592, -24.14321612903114911, -0.2833117244521584643 ) ) ;
#69435 = CARTESIAN_POINT ( 'NONE',  ( 2.564635614221720594, -21.35862533600356983, -1.500000000000002220 ) ) ;
#69436 = EDGE_CURVE ( 'NONE', #96941, #50118, #20928, .T. ) ;
#69437 = B_SPLINE_CURVE_WITH_KNOTS ( 'NONE', 3,
 ( #89500, #6253, #13860, #59560 ),
 .UNSPECIFIED., .F., .F.,
 ( 4, 4 ),
 ( 0.000000000000000000, 9.999999999998206125E-05 ),
 .UNSPECIFIED. ) ;
#69438 = CARTESIAN_POINT ( 'NONE',  ( -113.6228709571500701, -23.72773821059536559, 11.05748984161097503 ) ) ;
#69439 = ORIENTED_EDGE ( 'NONE', *, *, #54752, .F. ) ;
#69440 = CARTESIAN_POINT ( 'NONE',  ( -21.09505027744838657, -1.104435277493458045, -1.500000000000002220 ) ) ;
#69441 = DIRECTION ( 'NONE',  ( 0.000000000000000000, 0.000000000000000000, -1.000000000000000000 ) ) ;
#69442 = CARTESIAN_POINT ( 'NONE',  ( -58.86102183801504140, -25.14083923594471059, 2.947789366366678987 ) ) ;
#69443 = CARTESIAN_POINT ( 'NONE',  ( -83.59538750566655096, -23.96169478059713143, 10.65365249895718058 ) ) ;
#69444 = CARTESIAN_POINT ( 'NONE',  ( -119.5228709571500758, -29.50248528299804818, 1.056150453629045360 ) ) ;
#69445 = DIRECTION ( 'NONE',  ( -0.9872275723272646575, 0.000000000000000000, -0.1593164160933058515 ) ) ;
#69446 = CARTESIAN_POINT ( 'NONE',  ( -12.03526013704878039, -18.61824004984164560, -1.500000000000002220 ) ) ;
#69447 = CARTESIAN_POINT ( 'NONE',  ( -2.794871794871791604, -6.376774720514427841, 21.75000000000001066 ) ) ;
#69448 = VERTEX_POINT ( 'NONE', #62520 ) ;
#69449 = CARTESIAN_POINT ( 'NONE',  ( -51.85051548866884019, -25.24860163112497347, 5.725681047314564509 ) ) ;
#69450 = CARTESIAN_POINT ( 'NONE',  ( 12.36220485508518685, 4.378682769551595300, -27.78718873729292582 ) ) ;
#69451 = CARTESIAN_POINT ( 'NONE',  ( 2.021814659504407579E-13, -19.30000000000000426, 11.49999999999999645 ) ) ;
#69452 = CARTESIAN_POINT ( 'NONE',  ( -100.5838749402658294, -25.00158670708910691, 2.256160236439218369 ) ) ;
#69453 = CARTESIAN_POINT ( 'NONE',  ( -8.858824863812619910, -17.32749669425128047, 11.49999999999998934 ) ) ;
#69454 = CARTESIAN_POINT ( 'NONE',  ( -21.34312709018487553, 1.176582458498846462, 11.49999999999998934 ) ) ;
#69455 = CARTESIAN_POINT ( 'NONE',  ( -4.621320343559618848, 12.50000000000004974, 2.100000000000000089 ) ) ;
#69456 = CARTESIAN_POINT ( 'NONE',  ( 3.737436867076077363, 13.63388347648318444, 2.100000000000000089 ) ) ;
#69457 = DIRECTION ( 'NONE',  ( -0.000000000000000000, 1.000000000000000000, -0.000000000000000000 ) ) ;
#69458 = CARTESIAN_POINT ( 'NONE',  ( -101.3738023147422780, -25.18440161649941800, 3.986250810164079450 ) ) ;
#69459 = CARTESIAN_POINT ( 'NONE',  ( 21.55457256799317278, 7.124301260279622738, -1.500000000000002220 ) ) ;
#69460 = EDGE_CURVE ( 'NONE', #27239, #26914, #89041, .T. ) ;
#69461 = B_SPLINE_SURFACE_WITH_KNOTS ( 'NONE', 3, 3, ( 
 ( #42312, #10840, #64656, #26057 ),
 ( #87965, #18446, #41804, #34180 ),
 ( #65156, #76211, #68123, #29544 ),
 ( #21919, #91945, #7201, #52395 ),
 ( #5714, #6705, #38150, #83834 ),
 ( #13313, #44292, #52898, #82338 ),
 ( #74716, #99044, #69104, #60521 ),
 ( #5218, #14809, #75709, #45285 ),
 ( #45776, #30544, #36174, #91436 ),
 ( #22415, #67140, #75221, #14311 ) ),
 .UNSPECIFIED., .F., .F., .F.,
 ( 4, 3, 3, 4 ),
 ( 4, 4 ),
 ( 0.7022005934544806038, 0.7765311282028795059, 0.8508616629512784080, 0.9995227324480763231 ),
 ( 0.4995542859879725239, 0.5008647382424362693 ),
 .UNSPECIFIED. ) ;
#69462 = CARTESIAN_POINT ( 'NONE',  ( -98.62287095715007013, -23.47596703998600631, 11.44779298504227860 ) ) ;
#69463 = CARTESIAN_POINT ( 'NONE',  ( -115.6228709571500559, -29.50248528299804818, 1.056150453629045360 ) ) ;
#69464 = CARTESIAN_POINT ( 'NONE',  ( 14.04693994163893578, -13.95676237773968609, 11.49999999999999645 ) ) ;
#69465 = VECTOR ( 'NONE', #49947, 1000.000000000000114 ) ;
#69466 = CARTESIAN_POINT ( 'NONE',  ( -68.93918693012690824, -25.24795196732124936, 6.184868460502651821 ) ) ;
#69467 = ORIENTED_EDGE ( 'NONE', *, *, #11334, .F. ) ;
#69468 = DIRECTION ( 'NONE',  ( 0.000000000000000000, 2.173523156925980399E-06, -0.9999999999976378895 ) ) ;
#69469 = CARTESIAN_POINT ( 'NONE',  ( -5.912814555383966386, -5.876774720514418071, 20.28973052848695602 ) ) ;
#69471 = EDGE_CURVE ( 'NONE', #47313, #86012, #17847, .T. ) ;
#69470 = CARTESIAN_POINT ( 'NONE',  ( 3.252401863874215593, -0.3587747205143964613, -29.35688408629929214 ) ) ;
#69472 = CARTESIAN_POINT ( 'NONE',  ( 18.46943957830784555, -11.30625484363265265, -1.500000000000002220 ) ) ;
#69473 = EDGE_CURVE ( 'NONE', #95938, #17861, #53025, .T. ) ;
#69474 = CARTESIAN_POINT ( 'NONE',  ( -66.62287095715005592, -24.65952944569304606, 1.056160979905696573 ) ) ;
#69475 = AXIS2_PLACEMENT_3D ( 'NONE', #22709, #13609, #98344 ) ;
#69476 = CARTESIAN_POINT ( 'NONE',  ( -15.52061920455031618, -11.66286593722069931, -1.500000000000002220 ) ) ;
#69477 = ADVANCED_FACE ( 'NONE', ( #8731 ), #85851, .F. ) ;
#69478 = CARTESIAN_POINT ( 'NONE',  ( -114.5228709571500616, -24.64965694238408034, 8.947790433994192938 ) ) ;
#69479 = CARTESIAN_POINT ( 'NONE',  ( -55.64120953861098684, -24.40133493613049964, 9.663955038902800609 ) ) ;
#69480 = CARTESIAN_POINT ( 'NONE',  ( 16.46483878678964174, 11.07114234313464252, -1.500000000000002220 ) ) ;
#69481 = ORIENTED_EDGE ( 'NONE', *, *, #89659, .F. ) ;
#69482 = EDGE_CURVE ( 'NONE', #96543, #97326, #56673, .T. ) ;
#69483 = AXIS2_PLACEMENT_3D ( 'NONE', #50161, #81098, #42557 ) ;
#69484 = B_SPLINE_CURVE_WITH_KNOTS ( 'NONE', 3,
 ( #11234, #42702, #81744, #66555, #73637, #80246, #10739, #65054, #18841, #20323, #50307, #26469, #57433, #42211, #65551 ),
 .UNSPECIFIED., .F., .F.,
 ( 4, 2, 2, 2, 1, 2, 2, 4 ),
 ( 0.000000000000000000, 0.2500000000000124900, 0.3750000000000185962, 0.4375000000000195954, 0.4687500000000199285, 0.4843750000000200950, 0.5000000000000202061, 1.000000000000000000 ),
 .UNSPECIFIED. ) ;
#69485 = CARTESIAN_POINT ( 'NONE',  ( -3.780122020211411193, 19.97858748211865532, 11.49999999999999645 ) ) ;
#69486 = CARTESIAN_POINT ( 'NONE',  ( -80.53777470234541624, -24.92564183028979130, 1.928384488918253536 ) ) ;
#69487 = CARTESIAN_POINT ( 'NONE',  ( -3.749999999999999112, 25.69999999999999574, 2.100000000000000089 ) ) ;
#69488 = ORIENTED_EDGE ( 'NONE', *, *, #26671, .T. ) ;
#69489 = B_SPLINE_CURVE_WITH_KNOTS ( 'NONE', 3,
 ( #74065, #42134, #43615, #81170 ),
 .UNSPECIFIED., .F., .F.,
 ( 4, 4 ),
 ( 0.3307361706037946214, 0.3397426018759102107 ),
 .UNSPECIFIED. ) ;
#69490 = CARTESIAN_POINT ( 'NONE',  ( -102.6251301713998458, -24.51419770103155926, 9.386484678747178734 ) ) ;
#69491 = CARTESIAN_POINT ( 'NONE',  ( -116.4728709571500502, -25.40675428744130926, 5.000950440044785061 ) ) ;
#69492 = CARTESIAN_POINT ( 'NONE',  ( -58.87764846857956513, -25.14083923594470704, 2.947789366366647901 ) ) ;
#69493 = VECTOR ( 'NONE', #27700, 1000.000000000000114 ) ;
#69494 = CARTESIAN_POINT ( 'NONE',  ( -40.59314885895794589, -24.40133493613049609, 9.663955038902802386 ) ) ;
#69495 = CARTESIAN_POINT ( 'NONE',  ( -0.9078848932494473223, -5.876774720514411854, 19.67454710845354171 ) ) ;
#69496 = CARTESIAN_POINT ( 'NONE',  ( 18.99975792849237877, 6.539580213093530325, -1.500000000000002220 ) ) ;
#69497 = ADVANCED_FACE ( 'NONE', ( #70626 ), #47295, .F. ) ;
#69498 = CARTESIAN_POINT ( 'NONE',  ( -95.62287095715005592, -24.99132157543084531, 2.256160258750667502 ) ) ;
#69499 = ORIENTED_EDGE ( 'NONE', *, *, #14760, .F. ) ;
#69500 = CARTESIAN_POINT ( 'NONE',  ( -36.52287095715007581, -23.94994826722564696, -0.6494450866342753592 ) ) ;
#69501 = CARTESIAN_POINT ( 'NONE',  ( 12.66508800429495629, 19.07499079241581086, 11.49999999999999645 ) ) ;
#69502 = CARTESIAN_POINT ( 'NONE',  ( -22.67762270672801250, 1.536325718666671225, -1.500000000000002220 ) ) ;
#69503 = ORIENTED_EDGE ( 'NONE', *, *, #41772, .T. ) ;
#69504 = CARTESIAN_POINT ( 'NONE',  ( -109.6228709571500275, -23.96127896941632685, -0.6493128931037813745 ) ) ;
#69505 = CARTESIAN_POINT ( 'NONE',  ( -126.5228709571500616, -23.96177878511310055, 10.65340807706329507 ) ) ;
#69506 = CARTESIAN_POINT ( 'NONE',  ( -38.53898738578955374, -24.35071581493542325, 9.817618358456030592 ) ) ;
#69507 = CARTESIAN_POINT ( 'NONE',  ( -2.499999999999986677, 22.00000000000000000, 2.100000000000000089 ) ) ;
#69508 = ADVANCED_FACE ( 'NONE', ( #15825 ), #27150, .T. ) ;
#69509 = CARTESIAN_POINT ( 'NONE',  ( -84.62287095715007013, -23.48786465467241769, 11.44779295918254469 ) ) ;
#69510 = AXIS2_PLACEMENT_3D ( 'NONE', #44402, #52010, #99649 ) ;
#69511 = EDGE_CURVE ( 'NONE', #41503, #55229, #37164, .T. ) ;
#69512 = LINE ( 'NONE', #7602, #79317 ) ;
#69513 = VERTEX_POINT ( 'NONE', #66047 ) ;
#69514 = CARTESIAN_POINT ( 'NONE',  ( 19.80222353126469415, -4.898785079568316547, -1.500000000000002220 ) ) ;
#69515 = ORIENTED_EDGE ( 'NONE', *, *, #66468, .T. ) ;
#69516 = CARTESIAN_POINT ( 'NONE',  ( 16.94363762160741516, 15.55198921429254533, 11.49999999999998934 ) ) ;
#69517 = ADVANCED_FACE ( 'NONE', ( #72642 ), #96828, .T. ) ;
#69518 = CARTESIAN_POINT ( 'NONE',  ( -45.52287095715004739, -24.51163499207175889, 0.6490370598554249248 ) ) ;
#69519 = ORIENTED_EDGE ( 'NONE', *, *, #83955, .F. ) ;
#69520 = CARTESIAN_POINT ( 'NONE',  ( -108.6294922829741267, -23.96169478059714208, 10.65365249895716993 ) ) ;
#69521 = EDGE_CURVE ( 'NONE', #60463, #30073, #90571, .T. ) ;
#69522 = FACE_OUTER_BOUND ( 'NONE', #35942, .T. ) ;
#69523 = EDGE_CURVE ( 'NONE', #31069, #63463, #90351, .T. ) ;
#69524 = B_SPLINE_CURVE_WITH_KNOTS ( 'NONE', 3,
 ( #45614, #7041, #36993, #13143 ),
 .UNSPECIFIED., .F., .F.,
 ( 4, 4 ),
 ( 0.000000000000000000, 9.999999999996123101E-05 ),
 .UNSPECIFIED. ) ;
#69525 = CARTESIAN_POINT ( 'NONE',  ( -51.49047045075048601, -24.51419770103156637, 9.386484678747175181 ) ) ;
#69527 = EDGE_LOOP ( 'NONE', ( #23959, #31707, #86159, #31354 ) ) ;
#69526 = CARTESIAN_POINT ( 'NONE',  ( 14.70648301983428397, -15.34743991077593250, 11.49999999999999645 ) ) ;
#69528 = ORIENTED_EDGE ( 'NONE', *, *, #55521, .F. ) ;
#69529 = CARTESIAN_POINT ( 'NONE',  ( -0.8134642310582372859, 22.17477653155656725, 11.49999999999998934 ) ) ;
#69530 = CARTESIAN_POINT ( 'NONE',  ( 1.582324178664715975, -20.54890914157308401, 11.49999999999998934 ) ) ;
#69531 = ORIENTED_EDGE ( 'NONE', *, *, #71496, .F. ) ;
#69532 = ORIENTED_EDGE ( 'NONE', *, *, #42162, .F. ) ;
#69533 = FACE_OUTER_BOUND ( 'NONE', #61607, .T. ) ;
#69534 = EDGE_CURVE ( 'NONE', #56694, #1020, #20823, .T. ) ;
#69535 = CARTESIAN_POINT ( 'NONE',  ( 3.398286024651508530, -5.876774720514429617, 21.76255057507181334 ) ) ;
#69536 = VERTEX_POINT ( 'NONE', #43679 ) ;
#69537 = VECTOR ( 'NONE', #3387, 1000.000000000000000 ) ;
#69538 = CARTESIAN_POINT ( 'NONE',  ( -91.59442398169517219, -23.96119346886881019, -0.6495511937832073590 ) ) ;
#69539 = AXIS2_PLACEMENT_3D ( 'NONE', #13150, #53237, #44121 ) ;
#69540 = ORIENTED_EDGE ( 'NONE', *, *, #61396, .T. ) ;
#69541 = CARTESIAN_POINT ( 'NONE',  ( -39.52287095715006870, -23.72773821059535848, 11.05748984161097681 ) ) ;
#69542 = B_SPLINE_CURVE_WITH_KNOTS ( 'NONE', 3,
 ( #83438, #44903, #75825, #6324, #37280, #16928 ),
 .UNSPECIFIED., .F., .F.,
 ( 4, 2, 4 ),
 ( 0.000000000000000000, 0.001380901958385386376, 0.002761803916770772752 ),
 .UNSPECIFIED. ) ;
#69543 = DIRECTION ( 'NONE',  ( 0.000000000000000000, 0.9999999999976377785, 2.173523156925979975E-06 ) ) ;
#69544 = CARTESIAN_POINT ( 'NONE',  ( 8.324980675869593227, 19.10421180063631752, -1.500000000000002220 ) ) ;
#69545 = CARTESIAN_POINT ( 'NONE',  ( -20.93004649427559016, -6.003493321846349318, 11.49999999999999645 ) ) ;
#69546 = CARTESIAN_POINT ( 'NONE',  ( 25.98063551284147721, -4.258790553513050803, -11.44815252197057021 ) ) ;
#69547 = CARTESIAN_POINT ( 'NONE',  ( -99.67810188082559364, -25.06709179204377591, 7.399672078504718975 ) ) ;
#69548 = CARTESIAN_POINT ( 'NONE',  ( 11.54466316424315231, -19.26756404802103972, 11.49999999999998934 ) ) ;
#69549 = AXIS2_PLACEMENT_3D ( 'NONE', #61564, #16363, #69156 ) ;
#69550 = FACE_OUTER_BOUND ( 'NONE', #9004, .T. ) ;
#69551 = ORIENTED_EDGE ( 'NONE', *, *, #5950, .F. ) ;
#69552 = PLANE ( 'NONE',  #76049 ) ;
#69553 = CARTESIAN_POINT ( 'NONE',  ( -51.61997180002916963, -25.22394202344478131, 3.594056534852918983 ) ) ;
#69554 = ORIENTED_EDGE ( 'NONE', *, *, #51155, .F. ) ;
#69555 = AXIS2_PLACEMENT_3D ( 'NONE', #89351, #19818, #59397 ) ;
#69556 = VERTEX_POINT ( 'NONE', #5611 ) ;
#69557 = ORIENTED_EDGE ( 'NONE', *, *, #20905, .T. ) ;
#69558 = B_SPLINE_CURVE_WITH_KNOTS ( 'NONE', 3,
 ( #74022, #90241, #66433, #28336, #59296, #4516 ),
 .UNSPECIFIED., .F., .F.,
 ( 4, 2, 4 ),
 ( 0.000000000000000000, 0.001380901958385388545, 0.002761803916770777089 ),
 .UNSPECIFIED. ) ;
#69559 = CARTESIAN_POINT ( 'NONE',  ( 15.73328655151706101, -14.44092690703295467, -1.500000000000002220 ) ) ;
#69560 = ORIENTED_EDGE ( 'NONE', *, *, #61307, .T. ) ;
#69561 = CARTESIAN_POINT ( 'NONE',  ( 11.68726034403320746, 17.49698133428071145, -1.500000000000002220 ) ) ;
#69562 = CARTESIAN_POINT ( 'NONE',  ( -30.45988033841292975, -25.30656340722048014, 3.857144010898052588 ) ) ;
#69563 = VECTOR ( 'NONE', #27076, 1000.000000000000000 ) ;
#69564 = CARTESIAN_POINT ( 'NONE',  ( -111.3419982013945173, -25.27993372741254063, 4.063003188440275082 ) ) ;
#69565 = CARTESIAN_POINT ( 'NONE',  ( -49.85473837878901548, -25.05837338253707713, 7.491380643917580073 ) ) ;
#69566 = CARTESIAN_POINT ( 'NONE',  ( -21.26704322615652032, -5.532269525099344776, -1.500000000000002220 ) ) ;
#69567 = CARTESIAN_POINT ( 'NONE',  ( -52.62287095715004881, -23.72747288104442021, -1.053458166803663110 ) ) ;
#69568 = EDGE_LOOP ( 'NONE', ( #80805, #75912, #67826, #24232 ) ) ;
#69569 = DIRECTION ( 'NONE',  ( -0.7071067811865507924, 0.000000000000000000, 0.7071067811865442421 ) ) ;
#69570 = B_SPLINE_CURVE_WITH_KNOTS ( 'NONE', 3,
 ( #97023, #57485, #19887, #66606 ),
 .UNSPECIFIED., .F., .F.,
 ( 4, 4 ),
 ( 1.785902608152995868E-11, 0.002468655811832971662 ),
 .UNSPECIFIED. ) ;
#69571 = CARTESIAN_POINT ( 'NONE',  ( -127.5895376238167245, -23.47596703998600631, 11.44779298504227683 ) ) ;
#69572 = CARTESIAN_POINT ( 'NONE',  ( 7.204507412156021751, -19.57454612608841771, 11.49999999999999645 ) ) ;
#69573 = CARTESIAN_POINT ( 'NONE',  ( 31.66639312903740944, -5.493490882720638346, 28.57493973316426406 ) ) ;
#69574 = CARTESIAN_POINT ( 'NONE',  ( -111.6228709571500701, -23.48786465467241769, 11.44779295918254114 ) ) ;
#69575 = DIRECTION ( 'NONE',  ( -3.773278334453079030E-23, 0.9999999999976377785, 2.173523156925979128E-06 ) ) ;
#69576 = CARTESIAN_POINT ( 'NONE',  ( 9.569808575145499319, 19.01914523534739132, -1.500000000000002220 ) ) ;
#69577 = CARTESIAN_POINT ( 'NONE',  ( -2.499999999999993339, 19.99999999999999645, 2.100000000000000089 ) ) ;
#69578 = DIRECTION ( 'NONE',  ( 0.6599726524652353987, 0.000000000000000000, -0.7512896232465889890 ) ) ;
#69579 = CARTESIAN_POINT ( 'NONE',  ( 14.43441820105630136, -3.540887625665272598, -28.36222020492957796 ) ) ;
#69580 = CARTESIAN_POINT ( 'NONE',  ( -3.302878749216429544, 14.80319218833827044, 8.673617379884035472E-16 ) ) ;
#69581 = CARTESIAN_POINT ( 'NONE',  ( -21.69688529672534827, 6.072505851105969299, -1.500000000000002220 ) ) ;
#69582 = VECTOR ( 'NONE', #34052, 1000.000000000000000 ) ;
#69583 = EDGE_CURVE ( 'NONE', #82244, #12412, #46877, .T. ) ;
#69584 = DIRECTION ( 'NONE',  ( 0.9890158633619158257, 0.1478094111296165136, 0.000000000000000000 ) ) ;
#69585 = ORIENTED_EDGE ( 'NONE', *, *, #95849, .T. ) ;
#69586 = ADVANCED_FACE ( 'NONE', ( #52794 ), #67523, .F. ) ;
#69587 = CARTESIAN_POINT ( 'NONE',  ( -80.35919894935767616, -25.29542306156489673, 4.505481338088394239 ) ) ;
#69588 = CARTESIAN_POINT ( 'NONE',  ( 17.63768857353127828, -8.544740250177758512, 11.49999999999999645 ) ) ;
#69589 = DIRECTION ( 'NONE',  ( 1.046287966022745640E-14, 0.000000000000000000, -1.000000000000000000 ) ) ;
#69590 = CARTESIAN_POINT ( 'NONE',  ( 7.160000000000000142, -9.123836073446797812, -2.666350264951732552 ) ) ;
#69591 = VERTEX_POINT ( 'NONE', #14714 ) ;
#69592 = EDGE_CURVE ( 'NONE', #44878, #37372, #90849, .T. ) ;
#69593 = CARTESIAN_POINT ( 'NONE',  ( -50.58953762381671027, -23.48783264082478084, -1.443836473390070596 ) ) ;
#69594 = CARTESIAN_POINT ( 'NONE',  ( -108.5895376238167245, -24.66019654487199730, 8.947790411086135265 ) ) ;
#69595 = CARTESIAN_POINT ( 'NONE',  ( -91.96486695379628884, -25.25787539255926362, 3.590294762828090125 ) ) ;
#69596 = EDGE_CURVE ( 'NONE', #63904, #65522, #37397, .T. ) ;
#69597 = ADVANCED_FACE ( 'NONE', ( #76109 ), #6611, .T. ) ;
#69598 = CARTESIAN_POINT ( 'NONE',  ( 17.76913753361954562, 8.601950719843506121, -1.500000000000002220 ) ) ;
#69599 = EDGE_LOOP ( 'NONE', ( #44587, #21326, #4534, #62273 ) ) ;
#69600 = EDGE_CURVE ( 'NONE', #44562, #51996, #96687, .T. ) ;
#69601 = CARTESIAN_POINT ( 'NONE',  ( -109.8525198310536126, -25.20967124336913301, 3.399964862456664072 ) ) ;
#69602 = DATE_AND_TIME ( #21896, #50643 ) ;
#69603 = ORIENTED_EDGE ( 'NONE', *, *, #38903, .F. ) ;
#69604 = CARTESIAN_POINT ( 'NONE',  ( -46.52287095715007581, -23.47593901973090524, -1.443836447538997314 ) ) ;
#69605 = CARTESIAN_POINT ( 'NONE',  ( -107.6228709571500701, -23.48783264082479150, -1.443836473390060382 ) ) ;
#69606 = DIRECTION ( 'NONE',  ( -0.03244919754393515293, 0.000000000000000000, 0.9994733861282923959 ) ) ;
#69607 = LINE ( 'NONE', #15301, #94694 ) ;
#69608 = CARTESIAN_POINT ( 'NONE',  ( -2.196420576317535289, -5.876774720514410077, 19.14926908420044782 ) ) ;
#69609 = VECTOR ( 'NONE', #5875, 1000.000000000000000 ) ;
#69610 = CARTESIAN_POINT ( 'NONE',  ( -56.62287095715005592, -24.65952944569304250, 1.056160979905693464 ) ) ;
#69611 = DIRECTION ( 'NONE',  ( 0.000000000000000000, 0.000000000000000000, -1.000000000000000000 ) ) ;
#69612 = CARTESIAN_POINT ( 'NONE',  ( -19.95465934538571062, -0.7993260556091378310, 11.49999999999998934 ) ) ;
#69613 = EDGE_CURVE ( 'NONE', #20446, #55815, #63115, .T. ) ;
#69614 = CYLINDRICAL_SURFACE ( 'NONE', #15877, 1.306876713926001798 ) ;
#69615 = CARTESIAN_POINT ( 'NONE',  ( -45.63952611995537723, -24.52399227489127043, 9.353111116836528183 ) ) ;
#69616 = VERTEX_POINT ( 'NONE', #44685 ) ;
#69617 = AXIS2_PLACEMENT_3D ( 'NONE', #42732, #58945, #35110 ) ;
#69618 = ADVANCED_FACE ( 'NONE', ( #92339 ), #6108, .F. ) ;
#69619 = CIRCLE ( 'NONE', #9648, 1.699999999999999289 ) ;
#69620 = FACE_OUTER_BOUND ( 'NONE', #67912, .T. ) ;
#69621 = CARTESIAN_POINT ( 'NONE',  ( -109.3592350823140720, -25.18430345422392236, 4.175498078355194487 ) ) ;
#69622 = CARTESIAN_POINT ( 'NONE',  ( -6.499999999999992895, 1.999999999999999112, 2.499999999999999112 ) ) ;
#69623 = CARTESIAN_POINT ( 'NONE',  ( -100.5228709571500616, -23.48786465467242479, 11.44779295918254114 ) ) ;
#69624 = AXIS2_PLACEMENT_3D ( 'NONE', #73618, #80734, #96951 ) ;
#69625 = CARTESIAN_POINT ( 'NONE',  ( -97.52287095715006160, -24.65952944569304606, 1.056160979905702346 ) ) ;
#69626 = CARTESIAN_POINT ( 'NONE',  ( -83.54166051555876038, -24.65952944569304606, 1.056160979905700126 ) ) ;
#69627 = VECTOR ( 'NONE', #36360, 1000.000000000000000 ) ;
#69628 = CARTESIAN_POINT ( 'NONE',  ( 4.784292611718075072, -6.376774720514426953, -25.54547254883186014 ) ) ;
#69629 = CARTESIAN_POINT ( 'NONE',  ( 5.635247460261607166, -6.376774720514424288, 21.53093896358932469 ) ) ;
#69630 = ORIENTED_EDGE ( 'NONE', *, *, #86216, .T. ) ;
#69631 = B_SPLINE_CURVE_WITH_KNOTS ( 'NONE', 3,
 ( #100000, #92404, #29012, #59982 ),
 .UNSPECIFIED., .F., .F.,
 ( 4, 4 ),
 ( 1.387778780781445521E-17, 9.999999999997510880E-05 ),
 .UNSPECIFIED. ) ;
#69632 = CARTESIAN_POINT ( 'NONE',  ( -14.64122064730360862, 14.02963135428074004, -1.500000000000002220 ) ) ;
#69633 = CARTESIAN_POINT ( 'NONE',  ( 31.63505726983280297, 3.634951944882593988, 27.30823744647568674 ) ) ;
#69634 = CARTESIAN_POINT ( 'NONE',  ( -90.52287095715004739, -23.84047902841604838, -0.8780736468305390119 ) ) ;
#69636 = ORIENTED_EDGE ( 'NONE', *, *, #52871, .F. ) ;
#69635 = EDGE_CURVE ( 'NONE', #32857, #99058, #74470, .T. ) ;
#69637 = CARTESIAN_POINT ( 'NONE',  ( -95.52287095715006160, -23.47596703998600631, 11.44779298504228215 ) ) ;
#69638 = CARTESIAN_POINT ( 'NONE',  ( 4.282148337517553749, -19.64591042314588165, -1.500000000000002220 ) ) ;
#69639 = CARTESIAN_POINT ( 'NONE',  ( -4.359323203648655998, -20.60729432550360585, 11.49999999999999645 ) ) ;
#69640 = CARTESIAN_POINT ( 'NONE',  ( 12.17348956504948987, -18.45705692928949659, 11.49999999999998934 ) ) ;
#69641 = EDGE_CURVE ( 'NONE', #97595, #51586, #69619, .T. ) ;
#69642 = CARTESIAN_POINT ( 'NONE',  ( -19.38928925021375349, 6.733644070511561885, -1.500000000000002220 ) ) ;
#69643 = FACE_OUTER_BOUND ( 'NONE', #97809, .T. ) ;
#69644 = CARTESIAN_POINT ( 'NONE',  ( -53.62287095715004881, -24.65952944569303895, 1.056160979905692576 ) ) ;
#69645 = EDGE_LOOP ( 'NONE', ( #100117, #14343, #92139, #62082, #80767, #40328, #4445, #68131 ) ) ;
#69646 = PLANE ( 'NONE',  #8737 ) ;
#69647 = ORIENTED_EDGE ( 'NONE', *, *, #63162, .T. ) ;
#69648 = LINE ( 'NONE', #1641, #13862 ) ;
#69649 = B_SPLINE_SURFACE_WITH_KNOTS ( 'NONE', 3, 3, ( 
 ( #9105, #25831, #31947, #63419 ),
 ( #17216, #95344, #48182, #2507 ),
 ( #71521, #2007, #56806, #49193 ),
 ( #59280, #88241, #4002, #42076 ),
 ( #43064, #44055, #65427, #57310 ),
 ( #26336, #18707, #4505, #5488 ),
 ( #90229, #57796, #20702, #49687 ) ),
 .UNSPECIFIED., .F., .F., .F.,
 ( 4, 3, 4 ),
 ( 4, 4 ),
 ( 0.0004766839783818023761, 0.1029713700210893174, 0.2054660560637968370 ),
 ( 0.7196770707996874572, 0.7210218530338301512 ),
 .UNSPECIFIED. ) ;
#69650 = CARTESIAN_POINT ( 'NONE',  ( -20.27875734969026311, -4.776774720514394446, 22.60402280011863496 ) ) ;
#69651 = EDGE_LOOP ( 'NONE', ( #10285, #26483, #44455, #84303, #46972 ) ) ;
#69652 = ORIENTED_EDGE ( 'NONE', *, *, #78456, .F. ) ;
#69653 = ORIENTED_EDGE ( 'NONE', *, *, #34187, .T. ) ;
#69654 = CARTESIAN_POINT ( 'NONE',  ( -118.6228709571500417, -23.72747288104441665, -1.053458166803660667 ) ) ;
#69655 = CARTESIAN_POINT ( 'NONE',  ( -63.62287095715003460, -23.48783264082478084, -1.443836473390069042 ) ) ;
#69656 = CARTESIAN_POINT ( 'NONE',  ( -68.64046488457991302, -23.96169478059712787, 10.65365249895718414 ) ) ;
#69657 = CARTESIAN_POINT ( 'NONE',  ( 9.220172233967117492, 18.46515239161685784, -1.500000000000002220 ) ) ;
#69658 = CARTESIAN_POINT ( 'NONE',  ( 20.63042821663210091, 6.393326493806346100, 11.49999999999999645 ) ) ;
#69659 = ORIENTED_EDGE ( 'NONE', *, *, #16430, .T. ) ;
#69660 = CARTESIAN_POINT ( 'NONE',  ( -83.62287095715009855, -24.50216790748099527, 0.6166512839513712541 ) ) ;
#69661 = DIRECTION ( 'NONE',  ( 0.9921023176230514551, 0.000000000000000000, -0.1254312216594016816 ) ) ;
#69662 = CARTESIAN_POINT ( 'NONE',  ( -6.430504157862594994, -21.42354456762059201, 11.49999999999998934 ) ) ;
#69663 = CARTESIAN_POINT ( 'NONE',  ( -71.52287095715007581, -23.96127896941631619, -0.6493128931038050222 ) ) ;
#69664 = CARTESIAN_POINT ( 'NONE',  ( -84.54457827582588436, -24.51314013834316441, 0.6176544820404183955 ) ) ;
#69665 = ORIENTED_EDGE ( 'NONE', *, *, #33976, .F. ) ;
#69666 = CARTESIAN_POINT ( 'NONE',  ( 32.95642386911166710, -3.601225610321291182, -13.01540364303327380 ) ) ;
#69667 = CARTESIAN_POINT ( 'NONE',  ( -62.52287095715006160, -24.65952944569304606, 1.056160979905695463 ) ) ;
#69668 = CARTESIAN_POINT ( 'NONE',  ( -115.5228709571500474, -23.47593901973090524, -1.443836447538996204 ) ) ;
#69669 = CARTESIAN_POINT ( 'NONE',  ( -16.13976855045889636, 13.32451261336467496, 11.49999999999998934 ) ) ;
#69670 = ORIENTED_EDGE ( 'NONE', *, *, #81277, .F. ) ;
#69671 = AXIS2_PLACEMENT_3D ( 'NONE', #35680, #10844, #66657 ) ;
#69672 = CARTESIAN_POINT ( 'NONE',  ( -98.62287095715007013, -24.33832256526968862, 0.1851278514119928387 ) ) ;
#69673 = ORIENTED_EDGE ( 'NONE', *, *, #91901, .F. ) ;
#69674 = CARTESIAN_POINT ( 'NONE',  ( -50.62287095715005592, -23.47596703998600631, 11.44779298504227505 ) ) ;
#69675 = CARTESIAN_POINT ( 'NONE',  ( 10.98566517548414012, -18.08203305749968592, -1.500000000000002220 ) ) ;
#69676 = ORIENTED_EDGE ( 'NONE', *, *, #13464, .F. ) ;
#69677 = CARTESIAN_POINT ( 'NONE',  ( -3.108974358974359475, -6.376774720514417183, 20.36458333333334281 ) ) ;
#69678 = CARTESIAN_POINT ( 'NONE',  ( 18.19902423439809525, 11.99547645517801442, 11.49999999999998934 ) ) ;
#69679 = CARTESIAN_POINT ( 'NONE',  ( -7.640476926272304681, -6.376774720514415407, 20.25188360057253689 ) ) ;
#69680 = CARTESIAN_POINT ( 'NONE',  ( 26.37445894957760828, 2.682774720514426559, -11.69480419648520986 ) ) ;
#69681 = LINE ( 'NONE', #37724, #69230 ) ;
#69682 = CARTESIAN_POINT ( 'NONE',  ( 8.287826148123016878, -20.17477452812186201, -1.500000000000002220 ) ) ;
#69683 = FACE_OUTER_BOUND ( 'NONE', #57847, .T. ) ;
#69684 = VERTEX_POINT ( 'NONE', #67037 ) ;
#69685 = CARTESIAN_POINT ( 'NONE',  ( 21.57151214508649772, 3.625915217019311583E-15, 0.000000000000000000 ) ) ;
#69686 = CARTESIAN_POINT ( 'NONE',  ( -117.5228709571500758, -24.33832256527049509, 0.1851278514138643139 ) ) ;
#69687 = ORIENTED_EDGE ( 'NONE', *, *, #94900, .F. ) ;
#69688 = VECTOR ( 'NONE', #62458, 1000.000000000000114 ) ;
#69689 = B_SPLINE_CURVE_WITH_KNOTS ( 'NONE', 3,
 ( #99220, #7373, #69284, #6388 ),
 .UNSPECIFIED., .F., .F.,
 ( 4, 4 ),
 ( 0.000000000000000000, 0.0001002978978731668673 ),
 .UNSPECIFIED. ) ;
#69690 = ORIENTED_EDGE ( 'NONE', *, *, #56244, .T. ) ;
#69691 = VECTOR ( 'NONE', #9016, 1000.000000000000000 ) ;
#69692 = VERTEX_POINT ( 'NONE', #28439 ) ;
#69693 = CIRCLE ( 'NONE', #12894, 28.45799999999999486 ) ;
#69694 = CARTESIAN_POINT ( 'NONE',  ( -125.6228709571500559, -23.47596703998600631, 11.44779298504227860 ) ) ;
#69695 = CARTESIAN_POINT ( 'NONE',  ( 16.91677535067316995, -12.78530099663392505, -1.500000000000002220 ) ) ;
#69696 = CARTESIAN_POINT ( 'NONE',  ( -94.51007522493627278, -24.34968618360933945, 0.1864209137778860548 ) ) ;
#69697 = CARTESIAN_POINT ( 'NONE',  ( -79.25918010276897974, -25.27791844016729073, 6.969965416359520383 ) ) ;
#69698 = CARTESIAN_POINT ( 'NONE',  ( -20.77875734969026311, -3.316774720514426456, 27.45402280011862572 ) ) ;
#69699 = CARTESIAN_POINT ( 'NONE',  ( 33.25738712673413033, 4.772289986317655774, -12.75102155484566424 ) ) ;
#69700 = AXIS2_PLACEMENT_3D ( 'NONE', #93891, #33496, #8160 ) ;
#69701 = CARTESIAN_POINT ( 'NONE',  ( 17.07123823605233781, 9.195568589125342029, 11.49999999999998934 ) ) ;
#69702 = EDGE_CURVE ( 'NONE', #46879, #42461, #76006, .T. ) ;
#69703 = CARTESIAN_POINT ( 'NONE',  ( -70.35895856474229504, -25.31161946917133321, 5.313173610579343453 ) ) ;
#69704 = ORIENTED_EDGE ( 'NONE', *, *, #5458, .T. ) ;
#69705 = ADVANCED_FACE ( 'NONE', ( #98951 ), #75117, .F. ) ;
#69706 = CARTESIAN_POINT ( 'NONE',  ( -16.21482014894483470, 10.69450053600103345, 11.49999999999999645 ) ) ;
#69707 = CARTESIAN_POINT ( 'NONE',  ( -108.5228709571500616, -23.47596703998600631, 11.44779298504228038 ) ) ;
#69708 = CARTESIAN_POINT ( 'NONE',  ( -111.6228709571500559, -24.65952944569304606, 1.056160979905703901 ) ) ;
#69709 = VERTEX_POINT ( 'NONE', #56691 ) ;
#69710 = ADVANCED_FACE ( 'NONE', ( #62925 ), #93847, .F. ) ;
#69711 = CARTESIAN_POINT ( 'NONE',  ( 3.325015365150250535, -6.376774720514402972, 18.26971317031913955 ) ) ;
#69712 = FACE_OUTER_BOUND ( 'NONE', #4722, .T. ) ;
#69713 = EDGE_CURVE ( 'NONE', #98447, #7140, #9531, .T. ) ;
#69714 = DIRECTION ( 'NONE',  ( -3.773278334453079030E-23, 0.9999999999976377785, 2.173523156925979128E-06 ) ) ;
#69715 = CARTESIAN_POINT ( 'NONE',  ( -55.62287095715007013, -24.52232992886360563, 0.6492154411906059241 ) ) ;
#69716 = CARTESIAN_POINT ( 'NONE',  ( -6.723608784814384620, 18.44229941887336821, 11.49999999999998934 ) ) ;
#69717 = B_SPLINE_CURVE_WITH_KNOTS ( 'NONE', 3,
 ( #13728, #91858, #30465, #7629, #90364, #53311, #22827, #38578, #99953, #28961, #84243, #18, #5626, #98966, #52811, #45696, #69027, #59420 ),
 .UNSPECIFIED., .F., .F.,
 ( 4, 2, 2, 2, 2, 2, 2, 2, 4 ),
 ( 0.000000000000000000, 0.0002722776847237221888, 0.0005445553694474455702, 0.0008168330541711689517, 0.001089110738894892442, 0.001361388423618615715, 0.001633666108342339204, 0.001905943793066062477, 0.002178221477789786184 ),
 .UNSPECIFIED. ) ;
#69718 = CARTESIAN_POINT ( 'NONE',  ( 4.621320343559255583, 11.49999999999999467, 2.100000000000000089 ) ) ;
#69719 = EDGE_LOOP ( 'NONE', ( #28365, #55483, #72045, #54208 ) ) ;
#69720 = CARTESIAN_POINT ( 'NONE',  ( -21.57561264457377348, 0.06291308125064201673, -1.500000000000002220 ) ) ;
#69721 = CARTESIAN_POINT ( 'NONE',  ( -95.52287095715009002, -24.15516710230293995, 10.28746687063726029 ) ) ;
#69722 = EDGE_CURVE ( 'NONE', #54541, #18086, #31953, .T. ) ;
#69723 = CARTESIAN_POINT ( 'NONE',  ( -74.52287095715007581, -29.50250243563736774, 8.947779886222143375 ) ) ;
#69724 = CARTESIAN_POINT ( 'NONE',  ( -90.52287095715009002, -24.92604778743017846, 8.074972756849364330 ) ) ;
#69725 = CARTESIAN_POINT ( 'NONE',  ( -10.12245940999746985, -20.73198382670940987, -1.500000000000002220 ) ) ;
#69726 = PERSON_AND_ORGANIZATION ( #70597, #27821 ) ;
#69727 = CARTESIAN_POINT ( 'NONE',  ( -93.55798330475117552, -23.73766607897670511, -1.055555164236453569 ) ) ;
#69728 = CARTESIAN_POINT ( 'NONE',  ( 4.612744205187371271, -6.376774720514418959, 20.61169588237105188 ) ) ;
#69729 = CARTESIAN_POINT ( 'NONE',  ( -41.26959558397307148, -25.08918874615346439, 7.338714959427068862 ) ) ;
#69730 = FACE_OUTER_BOUND ( 'NONE', #85612, .T. ) ;
#69731 = CARTESIAN_POINT ( 'NONE',  ( -109.8541577975467192, -25.19951037986027131, 3.399436371649390498 ) ) ;
#69732 = CARTESIAN_POINT ( 'NONE',  ( -4.621320343559254695, 11.49999999999999645, 2.100000000000000089 ) ) ;
#69733 = CARTESIAN_POINT ( 'NONE',  ( -114.5168350146848155, -24.35071581493544457, 9.817618358456016381 ) ) ;
#69734 = CARTESIAN_POINT ( 'NONE',  ( 11.24879072547334324, 16.40116332625411033, 11.49999999999998934 ) ) ;
#69735 = CARTESIAN_POINT ( 'NONE',  ( 29.80070917940689412, -6.376774720514426953, 27.39560796525321607 ) ) ;
#69736 = CARTESIAN_POINT ( 'NONE',  ( -7.013475202606065828, -18.52788797337992222, -1.500000000000002220 ) ) ;
#69737 = CARTESIAN_POINT ( 'NONE',  ( 0.2428503871269292180, -5.876774720514414518, 19.85590024959437017 ) ) ;
#69738 = LINE ( 'NONE', #219, #88962 ) ;
#69739 = CARTESIAN_POINT ( 'NONE',  ( -42.52287095715005449, -23.72747288104469732, -1.053458166803227902 ) ) ;
#69740 = CARTESIAN_POINT ( 'NONE',  ( 16.28047541435887879, -12.87082401369967677, 11.49999999999999645 ) ) ;
#69741 = FACE_OUTER_BOUND ( 'NONE', #27014, .T. ) ;
#69742 = VECTOR ( 'NONE', #96730, 1000.000000000000114 ) ;
#69743 = CARTESIAN_POINT ( 'NONE',  ( -106.6235367472416868, -24.65952944569304250, 1.056160979905701902 ) ) ;
#69744 = CARTESIAN_POINT ( 'NONE',  ( 22.47986593085892437, -3.190245585651162230, 11.49999999999999645 ) ) ;
#69745 = ORIENTED_EDGE ( 'NONE', *, *, #84953, .T. ) ;
#69746 = CARTESIAN_POINT ( 'NONE',  ( -69.60238025275721441, -23.73766607897669445, -1.055555164236460008 ) ) ;
#69747 = CARTESIAN_POINT ( 'NONE',  ( -69.69245707645603716, -25.15756568742650856, 6.894249041125955380 ) ) ;
#69748 = ORIENTED_EDGE ( 'NONE', *, *, #10027, .T. ) ;
#69749 = CARTESIAN_POINT ( 'NONE',  ( -4.116507902937485142, 19.75820112358731251, 11.49999999999998934 ) ) ;
#69750 = CARTESIAN_POINT ( 'NONE',  ( -108.6228709571500559, -23.95044443724992078, 10.65354141964649592 ) ) ;
#69751 = CARTESIAN_POINT ( 'NONE',  ( -84.62287095715005592, -29.50250786944525672, 11.44777988621623521 ) ) ;
#69752 = ORIENTED_EDGE ( 'NONE', *, *, #67379, .T. ) ;
#69753 = ORIENTED_EDGE ( 'NONE', *, *, #31967, .F. ) ;
#69754 = CARTESIAN_POINT ( 'NONE',  ( 0.2428503871269292180, -5.876774720514413630, 19.85590024959437017 ) ) ;
#69755 = CARTESIAN_POINT ( 'NONE',  ( 6.305670413343573699, 22.00876638805999974, -1.500000000000002220 ) ) ;
#69756 = CARTESIAN_POINT ( 'NONE',  ( -79.34687923781920915, -25.26778825442007559, 5.960409282772108241 ) ) ;
#69757 = AXIS2_PLACEMENT_3D ( 'NONE', #32114, #63087, #34006 ) ;
#69758 = CARTESIAN_POINT ( 'NONE',  ( 2.319523670979641849, -21.48760272935114557, -1.500000000000002220 ) ) ;
#69759 = DIRECTION ( 'NONE',  ( 0.000000000000000000, 1.000000000000000000, 0.000000000000000000 ) ) ;
#69760 = CARTESIAN_POINT ( 'NONE',  ( 19.40856703110355852, -7.758221025823637262, 11.49999999999999645 ) ) ;
#69761 = ORIENTED_EDGE ( 'NONE', *, *, #20727, .F. ) ;
#69762 = AXIS2_PLACEMENT_3D ( 'NONE', #84475, #85974, #45434 ) ;
#69763 = CARTESIAN_POINT ( 'NONE',  ( -124.5553389390244945, -24.15543982623907482, -0.2315651400026562945 ) ) ;
#69764 = CARTESIAN_POINT ( 'NONE',  ( -14.32918165687622825, -16.72005635474405949, 11.49999999999998934 ) ) ;
#69765 = EDGE_CURVE ( 'NONE', #11670, #90247, #25143, .T. ) ;
#69766 = B_SPLINE_CURVE_WITH_KNOTS ( 'NONE', 3,
 ( #46201, #56839, #95377, #57341, #71552, #9641 ),
 .UNSPECIFIED., .F., .F.,
 ( 4, 2, 4 ),
 ( 1.570755371634072366E-05, 0.001396183895866090355, 0.002776660238015839915 ),
 .UNSPECIFIED. ) ;
#69768 = CARTESIAN_POINT ( 'NONE',  ( -124.4728709571500360, -25.40674640480650126, 5.000950440061919799 ) ) ;
#69767 = VECTOR ( 'NONE', #35525, 1000.000000000000000 ) ;
#69769 = CARTESIAN_POINT ( 'NONE',  ( 25.61870917940689196, 0.3587747205144265483, 28.79814474876424768 ) ) ;
#69770 = ORIENTED_EDGE ( 'NONE', *, *, #51535, .T. ) ;
#69771 = DIRECTION ( 'NONE',  ( -0.6599726524652346216, 0.000000000000000000, 0.7512896232465895441 ) ) ;
#69772 = EDGE_CURVE ( 'NONE', #21913, #30992, #44577, .T. ) ;
#69773 = DIRECTION ( 'NONE',  ( 0.000000000000000000, 0.000000000000000000, -1.000000000000000000 ) ) ;
#69774 = ORIENTED_EDGE ( 'NONE', *, *, #1793, .T. ) ;
#69775 = DIRECTION ( 'NONE',  ( -3.773278334444166432E-23, 1.000000000000000000, 0.000000000000000000 ) ) ;
#69776 = EDGE_LOOP ( 'NONE', ( #44242, #32446, #73569, #38104 ) ) ;
#69777 = ORIENTED_EDGE ( 'NONE', *, *, #59491, .T. ) ;
#69778 = DIRECTION ( 'NONE',  ( 0.000000000000000000, 1.000000000000000000, 0.000000000000000000 ) ) ;
#69779 = CARTESIAN_POINT ( 'NONE',  ( -68.52287095715006160, -23.48783264082476308, -1.443836473390092356 ) ) ;
#69780 = CARTESIAN_POINT ( 'NONE',  ( -4.358143420448500116, -5.876774720514413630, 19.75705121608222115 ) ) ;
#69781 = CARTESIAN_POINT ( 'NONE',  ( -12.04554601739387998, 16.56303510970703385, -1.500000000000002220 ) ) ;
#69782 = ORIENTED_EDGE ( 'NONE', *, *, #49844, .T. ) ;
#69783 = DIRECTION ( 'NONE',  ( 0.000000000000000000, 0.9999999999976377785, 2.173523156925979975E-06 ) ) ;
#69784 = CARTESIAN_POINT ( 'NONE',  ( -44.52203594336852888, -23.48783264082476663, -1.443836473390095021 ) ) ;
#69785 = CARTESIAN_POINT ( 'NONE',  ( 2.899999999999999467, 31.80000000000000071, 2.100000000000000089 ) ) ;
#69786 = CARTESIAN_POINT ( 'NONE',  ( 1.165341552704713513, 22.26021350444069213, -1.500000000000002220 ) ) ;
#69787 = FACE_OUTER_BOUND ( 'NONE', #43924, .T. ) ;
#69788 = CARTESIAN_POINT ( 'NONE',  ( -1.359786310227693251, -5.876774720514417183, 20.62654306927474579 ) ) ;
#69789 = EDGE_LOOP ( 'NONE', ( #69025, #28642, #31948 ) ) ;
#69790 = CARTESIAN_POINT ( 'NONE',  ( -29.49875734969025842, 0.3587747205144265483, 25.61802280011862720 ) ) ;
#69791 = CARTESIAN_POINT ( 'NONE',  ( -28.66728577581702808, -25.26248019189677763, 7.986659555697134039 ) ) ;
#69792 = CARTESIAN_POINT ( 'NONE',  ( -1.025521031027718299, 20.81036885881322362, -1.500000000000002220 ) ) ;
#69793 = ORIENTED_EDGE ( 'NONE', *, *, #31459, .F. ) ;
#69795 = ORIENTED_EDGE ( 'NONE', *, *, #23077, .T. ) ;
#69794 = CARTESIAN_POINT ( 'NONE',  ( -56.62287095715005592, -29.50248528299804818, 1.056150453629034924 ) ) ;
#69796 = CARTESIAN_POINT ( 'NONE',  ( -31.62287095715005236, -24.65952944569304250, 1.056160979905689690 ) ) ;
#69797 = CARTESIAN_POINT ( 'NONE',  ( 14.09988904737591575, 15.55221489148801872, -1.500000000000002220 ) ) ;
#69798 = ORIENTED_EDGE ( 'NONE', *, *, #93305, .F. ) ;
#69799 = DIRECTION ( 'NONE',  ( 0.000000000000000000, 0.000000000000000000, -1.000000000000000000 ) ) ;
#69800 = FACE_OUTER_BOUND ( 'NONE', #63068, .T. ) ;
#69801 = CARTESIAN_POINT ( 'NONE',  ( 5.109298100551870725, -5.356774720514426491, -27.55941679637891895 ) ) ;
#69802 = CARTESIAN_POINT ( 'NONE',  ( 30.09341516180546350, -1.682774720514426114, -13.89311774897855933 ) ) ;
#69803 = DIRECTION ( 'NONE',  ( 0.000000000000000000, 0.000000000000000000, 1.000000000000000000 ) ) ;
#69804 = DIRECTION ( 'NONE',  ( -1.000000000000000000, -3.773278334444166432E-23, -8.201307841325785021E-29 ) ) ;
#69806 = ORIENTED_EDGE ( 'NONE', *, *, #2249, .T. ) ;
#69805 = CARTESIAN_POINT ( 'NONE',  ( -2.516727866726558460, 22.04588476715296963, 11.49999999999999645 ) ) ;
#69807 = DIRECTION ( 'NONE',  ( 0.000000000000000000, -2.173523156925979552E-06, 0.9999999999976378895 ) ) ;
#69808 = CARTESIAN_POINT ( 'NONE',  ( -44.62287095715004170, -23.96177878511307568, 10.65340807706330573 ) ) ;
#69809 = ORIENTED_EDGE ( 'NONE', *, *, #58645, .T. ) ;
#69810 = CARTESIAN_POINT ( 'NONE',  ( 13.37577147909557773, 18.27418014603220442, -1.500000000000002220 ) ) ;
#69812 = ORIENTED_EDGE ( 'NONE', *, *, #2703, .F. ) ;
#69811 = CARTESIAN_POINT ( 'NONE',  ( -93.52287095715009002, -23.48783264082477018, -1.443836473390088360 ) ) ;
#69813 = ORIENTED_EDGE ( 'NONE', *, *, #73179, .F. ) ;
#69814 = CARTESIAN_POINT ( 'NONE',  ( -8.160000000000000142, -9.652339641703484574, -1.621096496867199033 ) ) ;
#69815 = AXIS2_PLACEMENT_3D ( 'NONE', #17499, #78881, #56584 ) ;
#69816 = CARTESIAN_POINT ( 'NONE',  ( -9.210493908506615313, -17.87979239004878451, -1.500000000000002220 ) ) ;
#69817 = CARTESIAN_POINT ( 'NONE',  ( -34.62287095715005592, -29.50250243563736774, 8.947779886222150481 ) ) ;
#69818 = ORIENTED_EDGE ( 'NONE', *, *, #51852, .T. ) ;
#69819 = EDGE_CURVE ( 'NONE', #20487, #36206, #7610, .T. ) ;
#69820 = B_SPLINE_CURVE_WITH_KNOTS ( 'NONE', 3,
 ( #4087, #49776, #19296, #35039, #49278, #65511 ),
 .UNSPECIFIED., .F., .F.,
 ( 4, 2, 4 ),
 ( 0.000000000000000000, 0.001380901958385393315, 0.002761803916770786630 ),
 .UNSPECIFIED. ) ;
#69821 = CARTESIAN_POINT ( 'NONE',  ( 14.43441819135929194, -3.316774720514426456, -28.36222020317710957 ) ) ;
#69822 = CARTESIAN_POINT ( 'NONE',  ( 3.003370282714790562, 22.13870467353671856, -1.500000000000002220 ) ) ;
#69823 = ORIENTED_EDGE ( 'NONE', *, *, #57831, .T. ) ;
#69824 = ORIENTED_EDGE ( 'NONE', *, *, #94097, .F. ) ;
#69825 = DIRECTION ( 'NONE',  ( 7.960204194457801640E-17, 1.000000000000000000, 0.000000000000000000 ) ) ;
#69826 = CARTESIAN_POINT ( 'NONE',  ( -89.62287095715004170, -24.64965695001468404, 8.947790433994180503 ) ) ;
#69827 = ADVANCED_FACE ( 'NONE', ( #39059 ), #81450, .T. ) ;
#69828 = FACE_OUTER_BOUND ( 'NONE', #92967, .T. ) ;
#69829 = CARTESIAN_POINT ( 'NONE',  ( -116.5228709571499763, -23.95044443724992789, 10.65354141964649237 ) ) ;
#69830 = EDGE_CURVE ( 'NONE', #99331, #27910, #48174, .T. ) ;
#69831 = DIRECTION ( 'NONE',  ( 0.000000000000000000, 0.000000000000000000, 1.000000000000000000 ) ) ;
#69832 = VECTOR ( 'NONE', #22005, 1000.000000000000000 ) ;
#69833 = CARTESIAN_POINT ( 'NONE',  ( 3.994393897313025743, -19.14333888664780048, -1.500000000000002220 ) ) ;
#69834 = EDGE_CURVE ( 'NONE', #60943, #77342, #98208, .T. ) ;
#69835 = PLANE ( 'NONE',  #83028 ) ;
#69836 = VECTOR ( 'NONE', #42836, 1000.000000000000000 ) ;
#69837 = CARTESIAN_POINT ( 'NONE',  ( 4.199879391047538491, -21.09745483596041282, -1.500000000000002220 ) ) ;
#69838 = CARTESIAN_POINT ( 'NONE',  ( -62.52287095715011844, -23.96177878511310055, 10.65340807706330217 ) ) ;
#69839 = EDGE_CURVE ( 'NONE', #56219, #61101, #5377, .T. ) ;
#69840 = FACE_OUTER_BOUND ( 'NONE', #48610, .T. ) ;
#69841 = DIRECTION ( 'NONE',  ( 0.7512896232465891000, 0.000000000000000000, 0.6599726524652351767 ) ) ;
#69842 = CARTESIAN_POINT ( 'NONE',  ( -107.5895376238167529, -23.47596703998600631, 11.44779298504227683 ) ) ;
#69843 = CARTESIAN_POINT ( 'NONE',  ( 22.85402955525884394, -0.1436109537974766814, -1.500000000000002220 ) ) ;
#69844 = APPROVAL_DATE_TIME ( #100256, #65024 ) ;
#69845 = DIRECTION ( 'NONE',  ( 0.000000000000000000, 0.000000000000000000, -1.000000000000000000 ) ) ;
#69846 = CARTESIAN_POINT ( 'NONE',  ( -42.52287095715004739, -23.48783264083366973, -1.443836473376261642 ) ) ;
#69847 = CARTESIAN_POINT ( 'NONE',  ( 7.329891291799937925, -18.66831812819665970, 11.49999999999999645 ) ) ;
#69848 = DIRECTION ( 'NONE',  ( 0.000000000000000000, -2.173523156925979552E-06, 0.9999999999976378895 ) ) ;
#69849 = CARTESIAN_POINT ( 'NONE',  ( -100.6228709571500559, -29.50248789122583659, 2.256150453626215580 ) ) ;
#69850 = CARTESIAN_POINT ( 'NONE',  ( 3.825381322105384285, -5.876774720514401196, 18.16071977647550995 ) ) ;
#69851 = DIRECTION ( 'NONE',  ( -0.000000000000000000, -1.000000000000000000, -0.000000000000000000 ) ) ;
#69852 = VERTEX_POINT ( 'NONE', #89616 ) ;
#69853 = EDGE_CURVE ( 'NONE', #69195, #57364, #66344, .T. ) ;
#69854 = CARTESIAN_POINT ( 'NONE',  ( 5.202077965628057576, -2.038091937962834166, -2.869745073849994963E-16 ) ) ;
#69855 = CARTESIAN_POINT ( 'NONE',  ( -109.0206074541901415, -25.23913850168018769, 3.730511194984860612 ) ) ;
#69856 = CARTESIAN_POINT ( 'NONE',  ( -12.31242093702619123, -17.95196869449987531, -1.500000000000002220 ) ) ;
#69857 = CARTESIAN_POINT ( 'NONE',  ( -68.93918693012690824, -29.50249643036528369, 6.184859213151739254 ) ) ;
#69858 = CARTESIAN_POINT ( 'NONE',  ( 13.10555085358618221, -14.64361678476065087, -1.500000000000002220 ) ) ;
#69859 = CARTESIAN_POINT ( 'NONE',  ( -122.6228709571500559, -24.51283580621365132, 0.6167428607019886933 ) ) ;
#69860 = CARTESIAN_POINT ( 'NONE',  ( -109.7735670026218173, -25.27925862195693796, 5.109898703217436555 ) ) ;
#69861 = CARTESIAN_POINT ( 'NONE',  ( -91.59442375792446001, -23.96169478059713498, 10.65365249895717881 ) ) ;
#69862 = CARTESIAN_POINT ( 'NONE',  ( 3.181132013147180970, -5.876774720514426065, 21.64201922499777808 ) ) ;
#69863 = CARTESIAN_POINT ( 'NONE',  ( -1.637206367458305500, 20.51943892441452633, 11.49999999999999645 ) ) ;
#69864 = DIRECTION ( 'NONE',  ( 0.000000000000000000, 0.000000000000000000, -1.000000000000000000 ) ) ;
#69865 = CARTESIAN_POINT ( 'NONE',  ( -120.6245372636320639, -24.73486907724918638, 1.287355809206965684 ) ) ;
#69866 = VERTEX_POINT ( 'NONE', #96722 ) ;
#69867 = CARTESIAN_POINT ( 'NONE',  ( -46.62287095715004881, -24.65952944569304250, 1.056160979905693020 ) ) ;
#69868 = FACE_OUTER_BOUND ( 'NONE', #70731, .T. ) ;
#69869 = CARTESIAN_POINT ( 'NONE',  ( -74.52287095715009002, -23.72773821059536914, 11.05748984161097148 ) ) ;
#69870 = CARTESIAN_POINT ( 'NONE',  ( 8.971512145086499856, -1.028487854913500810, 6.500000000000000000 ) ) ;
#69871 = CARTESIAN_POINT ( 'NONE',  ( -25.88669879221086134, -24.61459842209443494, 7.002165747688067654 ) ) ;
#69872 = CARTESIAN_POINT ( 'NONE',  ( 30.79432203307449711, 6.272817126675294119, 0.6151397435758989563 ) ) ;
#69873 = EDGE_CURVE ( 'NONE', #23809, #84257, #81006, .T. ) ;
#69874 = CARTESIAN_POINT ( 'NONE',  ( 13.09964176094197441, 18.96253433080681106, 11.49999999999999645 ) ) ;
#69875 = CARTESIAN_POINT ( 'NONE',  ( 10.87194125936840194, 20.03610521102953257, 11.49999999999998934 ) ) ;
#69876 = CARTESIAN_POINT ( 'NONE',  ( -74.50754834148092698, -24.15543982623906771, -0.2315651400026650653 ) ) ;
#69877 = CARTESIAN_POINT ( 'NONE',  ( -88.52287095715003318, -24.51283580621364777, 0.6167428607019784792 ) ) ;
#69878 = CARTESIAN_POINT ( 'NONE',  ( -123.5228709571500474, -24.34917612406837151, 0.1852690917426585981 ) ) ;
#69879 = CARTESIAN_POINT ( 'NONE',  ( -22.41777205227948855, 0.6913007675000180097, 11.49999999999999645 ) ) ;
#69880 = ORIENTED_EDGE ( 'NONE', *, *, #98794, .F. ) ;
#69881 = CARTESIAN_POINT ( 'NONE',  ( 27.53860345374808105, 1.682774720514426114, -1.352392034746782823 ) ) ;
#69882 = CARTESIAN_POINT ( 'NONE',  ( -43.52287095715006160, -24.64965694238406613, 8.947790433994205372 ) ) ;
#69883 = CARTESIAN_POINT ( 'NONE',  ( 15.37660858059359725, 15.65766701038582021, 11.49999999999998934 ) ) ;
#69884 = ADVANCED_FACE ( 'NONE', ( #4391 ), #98714, .F. ) ;
#69885 = CARTESIAN_POINT ( 'NONE',  ( -5.530932042872791499, -5.876774720514408301, 19.30497968945844534 ) ) ;
#69886 = DIRECTION ( 'NONE',  ( -0.000000000000000000, 1.000000000000000000, -0.000000000000000000 ) ) ;
#69887 = CARTESIAN_POINT ( 'NONE',  ( 2.903846153846159517, -6.376774720514415407, 19.99999999999999289 ) ) ;
#69888 = LINE ( 'NONE', #54674, #88144 ) ;
#69889 = LINE ( 'NONE', #880, #1489 ) ;
#69890 = ORIENTED_EDGE ( 'NONE', *, *, #57088, .F. ) ;
#69891 = CARTESIAN_POINT ( 'NONE',  ( -13.28352777634190396, 15.58691228024164310, 11.49999999999998934 ) ) ;
#69892 = ORIENTED_EDGE ( 'NONE', *, *, #20780, .F. ) ;
#69893 = EDGE_LOOP ( 'NONE', ( #29829, #48699, #30576, #60357 ) ) ;
#69894 = ORIENTED_EDGE ( 'NONE', *, *, #77885, .T. ) ;
#69895 = ORIENTED_EDGE ( 'NONE', *, *, #12024, .F. ) ;
#69896 = CARTESIAN_POINT ( 'NONE',  ( -20.32320236877023589, 10.94715076914730290, 11.49999999999998934 ) ) ;
#69897 = CARTESIAN_POINT ( 'NONE',  ( -82.52287095715003318, -24.50216790748205042, 0.6166512839542531710 ) ) ;
#69898 = CARTESIAN_POINT ( 'NONE',  ( 13.48481281434462531, 15.16087405922196041, -1.500000000000002220 ) ) ;
#69899 = ORIENTED_EDGE ( 'NONE', *, *, #7325, .F. ) ;
#69900 = DIRECTION ( 'NONE',  ( -0.06283980576413537855, 0.000000000000000000, -0.9980236263794188822 ) ) ;
#69901 = CARTESIAN_POINT ( 'NONE',  ( -92.60130187865181028, -23.48783264082478084, -1.443836473390064157 ) ) ;
#69903 = CARTESIAN_POINT ( 'NONE',  ( -127.6228709571500559, -29.50250243563736774, 8.947779886222132717 ) ) ;
#69902 = VECTOR ( 'NONE', #23015, 1000.000000000000000 ) ;
#69904 = CARTESIAN_POINT ( 'NONE',  ( -70.63225065262203373, -24.63355581998385091, 0.9682620441943861067 ) ) ;
#69906 = ORIENTED_EDGE ( 'NONE', *, *, #88724, .T. ) ;
#69905 = CARTESIAN_POINT ( 'NONE',  ( 12.90647603486358364, 17.18646895862681134, 11.49999999999999645 ) ) ;
#69907 = PLANE ( 'NONE',  #72743 ) ;
#69908 = CARTESIAN_POINT ( 'NONE',  ( -61.56642141492948639, -23.48786465467240703, 11.44779295918255002 ) ) ;
#69909 =( GEOMETRIC_REPRESENTATION_CONTEXT ( 3 ) GLOBAL_UNCERTAINTY_ASSIGNED_CONTEXT ( ( #54023 ) ) GLOBAL_UNIT_ASSIGNED_CONTEXT ( ( #16563, #66149, #25687 ) ) REPRESENTATION_CONTEXT ( 'NONE', 'WORKASPACE' ) );
#69910 = ORIENTED_EDGE ( 'NONE', *, *, #28634, .F. ) ;
#69911 = CARTESIAN_POINT ( 'NONE',  ( 12.20387445076365296, 16.77033177596414504, 11.49999999999998934 ) ) ;
#69912 = VERTEX_POINT ( 'NONE', #82003 ) ;
#69913 = PRODUCT_DEFINITION ( 'UNKNOWN', '', #87801, #52020 ) ;
#69915 = ORIENTED_EDGE ( 'NONE', *, *, #99072, .T. ) ;
#69914 = CARTESIAN_POINT ( 'NONE',  ( -70.75516858542015086, -25.30843098343074971, 4.197529876663087300 ) ) ;
#69916 = CARTESIAN_POINT ( 'NONE',  ( -111.5187044900002746, -23.96169478059714564, 10.65365249895717348 ) ) ;
#69917 = LINE ( 'NONE', #38466, #69691 ) ;
#69918 = ORIENTED_EDGE ( 'NONE', *, *, #71297, .T. ) ;
#69919 = ORIENTED_EDGE ( 'NONE', *, *, #2950, .F. ) ;
#69920 = CARTESIAN_POINT ( 'NONE',  ( 4.966983519792414370, -5.876774720514413630, 19.83633487160803099 ) ) ;
#69921 = CARTESIAN_POINT ( 'NONE',  ( -65.58911965655261156, -24.52300882791528380, 0.6510814631126250474 ) ) ;
#69922 = CARTESIAN_POINT ( 'NONE',  ( -21.70078857174656761, -3.768841730229552045, 11.49999999999999645 ) ) ;
#69923 = CARTESIAN_POINT ( 'NONE',  ( -89.50575723802535322, -24.51419770103157703, 9.386484678747176957 ) ) ;
#69924 = CARTESIAN_POINT ( 'NONE',  ( 22.42242567092132433, 2.420433022335332751, 11.49999999999998934 ) ) ;
#69925 = CARTESIAN_POINT ( 'NONE',  ( 6.892386425805808514, -19.84609432511738447, -1.500000000000002220 ) ) ;
#69926 = CARTESIAN_POINT ( 'NONE',  ( -10.24059822343757986, -5.876774720514426953, 22.82308057603840368 ) ) ;
#69927 = ORIENTED_EDGE ( 'NONE', *, *, #23422, .T. ) ;
#69928 = VERTEX_POINT ( 'NONE', #11486 ) ;
#69929 = CARTESIAN_POINT ( 'NONE',  ( -59.62287095715004881, -24.64965695001468404, 8.947790433994185832 ) ) ;
#69930 = AXIS2_PLACEMENT_3D ( 'NONE', #48229, #68692, #7271 ) ;
#69931 = FACE_OUTER_BOUND ( 'NONE', #15766, .T. ) ;
#69932 = ORIENTED_EDGE ( 'NONE', *, *, #21166, .F. ) ;
#69933 = CARTESIAN_POINT ( 'NONE',  ( 19.82261944725993175, 7.364942908566579405, 11.49999999999998934 ) ) ;
#69934 = CARTESIAN_POINT ( 'NONE',  ( -67.58953762381671027, -23.47593901973091235, -1.443836447539006196 ) ) ;
#69935 = CARTESIAN_POINT ( 'NONE',  ( -51.71530383401179876, -25.26040974995711608, 6.909342197498395066 ) ) ;
#69936 = CARTESIAN_POINT ( 'NONE',  ( -49.56659911537192897, -25.28200315853347035, 4.244126846616177673 ) ) ;
#69937 = CARTESIAN_POINT ( 'NONE',  ( -79.55620429048339304, -24.64898659630528854, 1.056161002820828143 ) ) ;
#69938 = DIRECTION ( 'NONE',  ( -3.773278334453079030E-23, 0.9999999999976377785, 2.173523156925979128E-06 ) ) ;
#69939 = CARTESIAN_POINT ( 'NONE',  ( 21.88104185797606505, 3.448541436957560880, -1.500000000000002220 ) ) ;
#69940 = CARTESIAN_POINT ( 'NONE',  ( -71.64476510811557830, -23.73766607897669800, -1.055555164236456012 ) ) ;
#69941 = EDGE_CURVE ( 'NONE', #2526, #88549, #20290, .T. ) ;
#69942 = B_SPLINE_CURVE_WITH_KNOTS ( 'NONE', 3,
 ( #38894, #95056, #64642, #334, #87442, #86938, #79324, #49403, #48896, #9818, #46513, #77442, #61755, #69855, #87951, #34167, #62249, #72228 ),
 .UNSPECIFIED., .F., .F.,
 ( 4, 2, 2, 2, 2, 2, 2, 2, 4 ),
 ( 1.411962612463446054E-17, 0.0002633899507887005873, 0.0005267799015773870800, 0.0007901698523660736270, 0.001053559803154760065, 0.001316949753943446504, 0.001580339704732133159, 0.001843729655520819598, 0.002107119606309506253 ),
 .UNSPECIFIED. ) ;
#69943 = VERTEX_POINT ( 'NONE', #20592 ) ;
#69944 = CARTESIAN_POINT ( 'NONE',  ( -51.81420417462592809, -25.24860145185455806, 5.643201866869797634 ) ) ;
#69945 = CARTESIAN_POINT ( 'NONE',  ( 8.071512145086522594, -7.528487854913505473, 4.500000000000000888 ) ) ;
#69946 = CARTESIAN_POINT ( 'NONE',  ( -43.62287095715006302, -23.96127896941632685, -0.6493128931037891460 ) ) ;
#69947 = CARTESIAN_POINT ( 'NONE',  ( -41.86208256938783023, -25.26663232696201433, 4.025867116275735569 ) ) ;
#69948 = CARTESIAN_POINT ( 'NONE',  ( -39.62287095715005592, -24.64965695001468404, 8.947790433994187609 ) ) ;
#69949 = CARTESIAN_POINT ( 'NONE',  ( 9.746180923669104601, -16.83516941858706417, 11.49999999999998934 ) ) ;
#69950 = ADVANCED_FACE ( 'NONE', ( #36331 ), #3896, .T. ) ;
#69951 = CARTESIAN_POINT ( 'NONE',  ( -9.924231251898440576, -18.97836718215353713, 11.49999999999998934 ) ) ;
#69952 = CARTESIAN_POINT ( 'NONE',  ( -38.52287095715006870, -24.66019654487199730, 8.947790411086121054 ) ) ;
#69953 = CARTESIAN_POINT ( 'NONE',  ( -60.54140983439796742, -24.52399227489757649, 9.353111116819363247 ) ) ;
#69954 = B_SPLINE_CURVE_WITH_KNOTS ( 'NONE', 3,
 ( #73501, #94331, #3993, #52655 ),
 .UNSPECIFIED., .F., .F.,
 ( 4, 4 ),
 ( 0.6702645439819958639, 0.6792709752541115087 ),
 .UNSPECIFIED. ) ;
#69955 = VECTOR ( 'NONE', #29282, 1000.000000000000000 ) ;
#69956 = EDGE_CURVE ( 'NONE', #19418, #81354, #45828, .T. ) ;
#69957 = CARTESIAN_POINT ( 'NONE',  ( -51.62816867347140715, -24.51314013834315730, 0.6176544820404110681 ) ) ;
#69958 = CARTESIAN_POINT ( 'NONE',  ( -101.2905359165590227, -25.18440123917106277, 3.812648632975031315 ) ) ;
#69959 = CARTESIAN_POINT ( 'NONE',  ( 13.97002500213282516, -17.90638934399130733, -1.500000000000002220 ) ) ;
#69960 = CARTESIAN_POINT ( 'NONE',  ( -98.51906589821315663, -23.73766607897669800, -1.055555164236454013 ) ) ;
#69961 = CARTESIAN_POINT ( 'NONE',  ( -62.62287095715002039, -24.35013146730203815, 9.818937971375111928 ) ) ;
#69962 = CARTESIAN_POINT ( 'NONE',  ( -4.880483578727112359, 19.22116399702514045, 11.49999999999999645 ) ) ;
#69963 = CARTESIAN_POINT ( 'NONE',  ( -123.6266590520278186, -23.48786465467241769, 11.44779295918253759 ) ) ;
#69964 = CARTESIAN_POINT ( 'NONE',  ( 8.071512145086501278, -0.8690767389352472838, 3.741933809627420171 ) ) ;
#69965 = VERTEX_POINT ( 'NONE', #65804 ) ;
#69966 = EDGE_CURVE ( 'NONE', #34234, #53182, #14362, .T. ) ;
#69967 = FACE_OUTER_BOUND ( 'NONE', #93607, .T. ) ;
#69968 = CARTESIAN_POINT ( 'NONE',  ( -66.52287095715006160, -29.50250243563736774, 8.947779886222143375 ) ) ;
#69969 = FACE_OUTER_BOUND ( 'NONE', #23745, .T. ) ;
#69970 = CARTESIAN_POINT ( 'NONE',  ( 20.17453868081960167, 7.849935799312063089, 11.49999999999998934 ) ) ;
#69971 = CARTESIAN_POINT ( 'NONE',  ( -67.52287095715006160, -29.50250243563736774, 8.947779886222143375 ) ) ;
#69972 = CARTESIAN_POINT ( 'NONE',  ( -5.977879402576776968, -18.46583800616800630, -1.500000000000002220 ) ) ;
#69973 = CARTESIAN_POINT ( 'NONE',  ( -61.62287095715004170, -23.72773821059536559, 11.05748984161097503 ) ) ;
#69974 = CARTESIAN_POINT ( 'NONE',  ( -18.24533751216517885, 7.751685665592884078, 11.49999999999998934 ) ) ;
#69975 = CIRCLE ( 'NONE', #26232, 3.549999999999999378 ) ;
#69976 = ORIENTED_EDGE ( 'NONE', *, *, #8486, .F. ) ;
#69977 = LOCAL_TIME ( 0, 54, 15.00000000000000000, #98776 ) ;
#69978 = CARTESIAN_POINT ( 'NONE',  ( 12.54693703879240196, 16.07252283493236433, 11.49999999999999645 ) ) ;
#69979 = DIRECTION ( 'NONE',  ( 1.000000000000000000, 3.773278334444167608E-23, 8.201307833595939069E-29 ) ) ;
#69980 = CARTESIAN_POINT ( 'NONE',  ( -104.5228709571501184, -23.48783264082477373, -1.443836473390087027 ) ) ;
#69981 = EDGE_LOOP ( 'NONE', ( #85705, #76417, #58446, #20147 ) ) ;
#69982 = CARTESIAN_POINT ( 'NONE',  ( -80.40673297319085577, -25.03305104182449270, 7.562216455819397609 ) ) ;
#69983 = DIRECTION ( 'NONE',  ( 0.000000000000000000, 0.000000000000000000, -1.000000000000000000 ) ) ;
#69984 = CARTESIAN_POINT ( 'NONE',  ( -49.35191700208513765, -25.25214480681022522, 5.185240423550362188 ) ) ;
#69985 = CARTESIAN_POINT ( 'NONE',  ( -128.6228709571500417, -23.96127896941633750, -0.6493128931037734919 ) ) ;
#69986 = FACE_OUTER_BOUND ( 'NONE', #40583, .T. ) ;
#69987 = CARTESIAN_POINT ( 'NONE',  ( 4.282148337517553749, -19.64591042314588165, 11.49999999999998934 ) ) ;
#69988 = EDGE_CURVE ( 'NONE', #20487, #17929, #17764, .T. ) ;
#69989 = FACE_OUTER_BOUND ( 'NONE', #81241, .T. ) ;
#69990 = EDGE_LOOP ( 'NONE', ( #81534, #92870 ) ) ;
#69991 = DIRECTION ( 'NONE',  ( -0.8264557562326033668, 0.000000000000000000, -0.5630016722799281448 ) ) ;
#69992 = EDGE_CURVE ( 'NONE', #94825, #63151, #51563, .T. ) ;
#69993 = CARTESIAN_POINT ( 'NONE',  ( -9.675568039816649701, -20.77828039667204862, 11.49999999999999645 ) ) ;
#69994 = CARTESIAN_POINT ( 'NONE',  ( 13.97002500213282516, -17.90638934399130733, 11.49999999999998934 ) ) ;
#69995 = ORIENTED_EDGE ( 'NONE', *, *, #26630, .T. ) ;
#69996 = CARTESIAN_POINT ( 'NONE',  ( 5.271800844963591359, -5.356774720514425603, -28.56638892015329034 ) ) ;
#69997 = LINE ( 'NONE', #62397, #23463 ) ;
#69998 = CARTESIAN_POINT ( 'NONE',  ( -38.53313680577858236, -24.51419770103157347, 9.386484678747176957 ) ) ;
#69999 = DIRECTION ( 'NONE',  ( 0.000000000000000000, 2.173523156925980399E-06, -0.9999999999976378895 ) ) ;
#70000 = CARTESIAN_POINT ( 'NONE',  ( -128.5899664246173302, -23.96169478059714919, 10.65365249895716993 ) ) ;
#70001 = EDGE_CURVE ( 'NONE', #99053, #11386, #29044, .T. ) ;
#70002 = AXIS2_PLACEMENT_3D ( 'NONE', #75916, #84038, #6423 ) ;
#70003 = B_SPLINE_CURVE_WITH_KNOTS ( 'NONE', 3,
 ( #82093, #66393, #56780, #43042 ),
 .UNSPECIFIED., .F., .F.,
 ( 4, 4 ),
 ( 0.000000000000000000, 9.999999999998898659E-05 ),
 .UNSPECIFIED. ) ;
#70004 = DIRECTION ( 'NONE',  ( 0.000000000000000000, 1.000000000000000000, -0.000000000000000000 ) ) ;
#70005 = ORIENTED_EDGE ( 'NONE', *, *, #71638, .T. ) ;
#70006 = CARTESIAN_POINT ( 'NONE',  ( -16.54958403137900191, 11.88860064210666856, -1.500000000000002220 ) ) ;
#70007 = B_SPLINE_CURVE_WITH_KNOTS ( 'NONE', 3,
 ( #68146, #22439, #20455, #84352, #14835, #75247 ),
 .UNSPECIFIED., .F., .F.,
 ( 4, 2, 4 ),
 ( 0.000000000000000000, 0.001380764517854766050, 0.002761529035709532100 ),
 .UNSPECIFIED. ) ;
#70008 = ORIENTED_EDGE ( 'NONE', *, *, #65735, .F. ) ;
#70009 = CARTESIAN_POINT ( 'NONE',  ( -19.49525799874905729, 12.17417675796824561, 11.49999999999998934 ) ) ;
#70010 = CARTESIAN_POINT ( 'NONE',  ( -54.62367911701477396, -24.66019654487199375, 8.947790411086119278 ) ) ;
#70011 = VERTEX_POINT ( 'NONE', #21090 ) ;
#70012 = CARTESIAN_POINT ( 'NONE',  ( -108.5505251014125321, -24.51419770103157347, 9.386484678747168076 ) ) ;
#70013 = CARTESIAN_POINT ( 'NONE',  ( 2.976770017179964700, -6.376774720514420736, 20.68690469677381927 ) ) ;
#70014 = CARTESIAN_POINT ( 'NONE',  ( -111.5228709571500332, -23.95044443724993144, 10.65354141964649237 ) ) ;
#70016 = ORIENTED_EDGE ( 'NONE', *, *, #75936, .T. ) ;
#70015 = CARTESIAN_POINT ( 'NONE',  ( 8.224165413489119558, 19.69228431130148493, 11.49999999999999645 ) ) ;
#70017 = AXIS2_PLACEMENT_3D ( 'NONE', #1345, #15048, #53638 ) ;
#70018 = EDGE_LOOP ( 'NONE', ( #29634, #48576, #80280, #82966 ) ) ;
#70019 = CARTESIAN_POINT ( 'NONE',  ( 21.63176498729014341, 4.993826359924048219, 11.49999999999998934 ) ) ;
#70020 = AXIS2_PLACEMENT_3D ( 'NONE', #66139, #27054, #11327 ) ;
#70021 = CARTESIAN_POINT ( 'NONE',  ( 7.614520588612671226, -19.20288753073135268, -1.500000000000002220 ) ) ;
#70022 = EDGE_CURVE ( 'NONE', #49913, #98343, #4683, .T. ) ;
#70023 = ORIENTED_EDGE ( 'NONE', *, *, #57088, .T. ) ;
#70024 = EDGE_LOOP ( 'NONE', ( #11267, #49207 ) ) ;
#70025 = CARTESIAN_POINT ( 'NONE',  ( -112.6228709571500701, -23.95044443724992433, 10.65354141964649948 ) ) ;
#70026 = CARTESIAN_POINT ( 'NONE',  ( -95.51719868888432075, -23.85049219812686161, 10.88485053497527133 ) ) ;
#70027 = VERTEX_POINT ( 'NONE', #52056 ) ;
#70028 = CARTESIAN_POINT ( 'NONE',  ( -91.59781571226605479, -23.73766607897670156, -1.055555164236454235 ) ) ;
#70029 = ADVANCED_FACE ( 'NONE', ( #57680 ), #99692, .F. ) ;
#70030 = B_SPLINE_CURVE_WITH_KNOTS ( 'NONE', 3,
 ( #77477, #31824, #78982, #62793, #54668, #55175, #93708, #24694 ),
 .UNSPECIFIED., .F., .F.,
 ( 4, 2, 2, 4 ),
 ( -0.001224554619866349532, -0.0002241820295893679187, 0.0007761905606876136950, 0.002776935741241577139 ),
 .UNSPECIFIED. ) ;
#70031 = ORIENTED_EDGE ( 'NONE', *, *, #52617, .T. ) ;
#70032 = CARTESIAN_POINT ( 'NONE',  ( -58.63776154008928643, -24.15620529776628089, 10.23563542870660470 ) ) ;
#70033 = PLANE ( 'NONE',  #90838 ) ;
#70034 = CARTESIAN_POINT ( 'NONE',  ( -5.744250498300313090, 20.02623800365557472, -1.500000000000002220 ) ) ;
#70035 = CARTESIAN_POINT ( 'NONE',  ( 8.107222467604051630, 20.28165043084963060, 11.49999999999999645 ) ) ;
#70036 = CARTESIAN_POINT ( 'NONE',  ( -91.23534077628075067, -25.22391154813774605, 6.409327647370976599 ) ) ;
#70037 = CARTESIAN_POINT ( 'NONE',  ( -78.55031912633015168, -24.15620529776628445, 10.23563542870660292 ) ) ;
#70038 = CARTESIAN_POINT ( 'NONE',  ( -22.07377061809603092, 4.253497373390751513, -1.500000000000002220 ) ) ;
#70039 = ADVANCED_FACE ( 'NONE', ( #68775 ), #83991, .T. ) ;
#70040 = ADVANCED_FACE ( 'NONE', ( #39311 ), #84985, .F. ) ;
#70041 = CARTESIAN_POINT ( 'NONE',  ( -85.62287095715005592, -29.50250786944525672, 11.44777988621623344 ) ) ;
#70042 = DIRECTION ( 'NONE',  ( -0.000000000000000000, 1.000000000000000000, -0.000000000000000000 ) ) ;
#70043 = CIRCLE ( 'NONE', #37595, 28.96799999999999287 ) ;
#70044 = DIRECTION ( 'NONE',  ( 0.000000000000000000, 1.000000000000000000, 0.000000000000000000 ) ) ;
#70046 = EDGE_CURVE ( 'NONE', #74266, #32974, #85482, .T. ) ;
#70045 = CC_DESIGN_SECURITY_CLASSIFICATION ( #34420, ( #78135 ) ) ;
#70047 = ORIENTED_EDGE ( 'NONE', *, *, #31209, .F. ) ;
#70048 = EDGE_LOOP ( 'NONE', ( #89155, #76738, #51489, #29081 ) ) ;
#70049 = ORIENTED_EDGE ( 'NONE', *, *, #23760, .T. ) ;
#70050 = CARTESIAN_POINT ( 'NONE',  ( -5.188002292566340934, -20.72503599944539587, -1.500000000000002220 ) ) ;
#70051 = ORIENTED_EDGE ( 'NONE', *, *, #28443, .T. ) ;
#70052 = CARTESIAN_POINT ( 'NONE',  ( -13.06023916655064276, -16.53025015627232719, -1.500000000000002220 ) ) ;
#70053 = CARTESIAN_POINT ( 'NONE',  ( -30.55377735246407411, -24.38452336476660065, 0.3015907515355735202 ) ) ;
#70054 = CARTESIAN_POINT ( 'NONE',  ( 15.91301918423788919, -12.03417825965012433, -1.500000000000002220 ) ) ;
#70055 = CARTESIAN_POINT ( 'NONE',  ( -114.5228709571500616, -23.48786465467241769, 11.44779295918253936 ) ) ;
#70056 = CARTESIAN_POINT ( 'NONE',  ( 3.004381791450704942, -6.376774720514420736, 20.78526834885430219 ) ) ;
#70057 = CARTESIAN_POINT ( 'NONE',  ( 10.07166557822571207, 19.55152498600455857, -1.500000000000002220 ) ) ;
#70058 = DIRECTION ( 'NONE',  ( 0.000000000000000000, 0.000000000000000000, 1.000000000000000000 ) ) ;
#70059 = VERTEX_POINT ( 'NONE', #30197 ) ;
#70060 = CARTESIAN_POINT ( 'NONE',  ( -74.58953762381672448, -24.64965694238407679, 8.947790433994656567 ) ) ;
#70061 = ADVANCED_FACE ( 'NONE', ( #62168 ), #38310, .F. ) ;
#70062 = DIRECTION ( 'NONE',  ( 0.6599726524652352877, -0.000000000000000000, -0.7512896232465891000 ) ) ;
#70063 = CARTESIAN_POINT ( 'NONE',  ( -9.832896139050584239, -18.40278743011522877, 11.49999999999999645 ) ) ;
#70064 = CARTESIAN_POINT ( 'NONE',  ( 31.63910543787568130, -6.180494461685818841, 27.51903215948834358 ) ) ;
#70065 = DIRECTION ( 'NONE',  ( -3.773278334444166432E-23, 1.000000000000000000, 0.000000000000000000 ) ) ;
#70066 = CARTESIAN_POINT ( 'NONE',  ( -20.48352523709943185, -22.69084714409266823, 11.44779298504228215 ) ) ;
#70067 = CARTESIAN_POINT ( 'NONE',  ( 11.00477826368897283, 18.22718707545001138, -1.500000000000002220 ) ) ;
#70068 = FACE_OUTER_BOUND ( 'NONE', #17096, .T. ) ;
#70069 = CARTESIAN_POINT ( 'NONE',  ( -107.5116926678866207, -24.66019654487199730, 8.947790411086115725 ) ) ;
#70070 = ADVANCED_FACE ( 'NONE', ( #75873 ), #4496, .T. ) ;
#70071 = DIRECTION ( 'NONE',  ( -2.327730190238738523E-16, 1.000000000000000000, 8.064610422320909082E-16 ) ) ;
#70072 = CARTESIAN_POINT ( 'NONE',  ( -70.65754726777662142, -25.12112739299269037, 7.112216829152949948 ) ) ;
#70073 = CARTESIAN_POINT ( 'NONE',  ( 14.32739804834607256, 17.34395043298086847, -1.500000000000002220 ) ) ;
#70074 = AXIS2_PLACEMENT_3D ( 'NONE', #98135, #28148, #21506 ) ;
#70075 = B_SPLINE_SURFACE_WITH_KNOTS ( 'NONE', 3, 3, ( 
 ( #94754, #18626, #86145, #16627 ),
 ( #47599, #70935, #94253, #55718 ),
 ( #17130, #97258, #34866, #49604 ),
 ( #27750, #42988, #51092, #26750 ),
 ( #19627, #74422, #57714, #58700 ),
 ( #59206, #50099, #11517, #50589 ),
 ( #4915, #89153, #73926, #90148 ) ),
 .UNSPECIFIED., .F., .F., .F.,
 ( 4, 3, 4 ),
 ( 4, 4 ),
 ( 0.7945040050992245861, 0.8970133687736507877, 0.9995227324480768782 ),
 ( 0.8697150038779488668, 0.8711292465922757522 ),
 .UNSPECIFIED. ) ;
#70076 = ADVANCED_FACE ( 'NONE', ( #92101 ), #60677, .F. ) ;
#70077 = CARTESIAN_POINT ( 'NONE',  ( -129.5562042904833788, -24.66019654487200441, 8.947790411086121054 ) ) ;
#70078 = VERTEX_POINT ( 'NONE', #46933 ) ;
#70079 = CARTESIAN_POINT ( 'NONE',  ( 8.499999999999989342, 18.99999999999977973, 2.100000000000000089 ) ) ;
#70080 = DIRECTION ( 'NONE',  ( 0.09824042138329590335, -0.9951627101165079203, -3.519298150595267883E-15 ) ) ;
#70081 = CARTESIAN_POINT ( 'NONE',  ( -8.027368788987615744, 17.96763083595211441, 11.49999999999999645 ) ) ;
#70082 = DIRECTION ( 'NONE',  ( 0.000000000000000000, -2.173523156925980399E-06, 0.9999999999976378895 ) ) ;
#70083 = DIRECTION ( 'NONE',  ( 3.773278334444167608E-23, -1.000000000000000000, 0.000000000000000000 ) ) ;
#70084 = ORIENTED_EDGE ( 'NONE', *, *, #8558, .T. ) ;
#70085 = EDGE_CURVE ( 'NONE', #69320, #71901, #77858, .T. ) ;
#70086 = CARTESIAN_POINT ( 'NONE',  ( -89.52287095715001897, -23.95044443724991723, 10.65354141964648882 ) ) ;
#70087 = CARTESIAN_POINT ( 'NONE',  ( -115.5228709571500616, -29.50248789122583659, 2.256150453626215580 ) ) ;
#70088 = CARTESIAN_POINT ( 'NONE',  ( -100.2069791292054504, -25.31439543413117477, 5.245324408949481487 ) ) ;
#70089 = B_SPLINE_CURVE_WITH_KNOTS ( 'NONE', 3,
 ( #67031, #73627, #43185, #88861 ),
 .UNSPECIFIED., .F., .F.,
 ( 4, 4 ),
 ( 0.000000000000000000, 9.999999999998897304E-05 ),
 .UNSPECIFIED. ) ;
#70090 = EDGE_CURVE ( 'NONE', #95766, #15382, #36124, .T. ) ;
#70091 = DIRECTION ( 'NONE',  ( -3.773278334444166432E-23, 1.000000000000000000, 0.000000000000000000 ) ) ;
#70092 = CARTESIAN_POINT ( 'NONE',  ( 18.24634267693259559, -7.554628487255452107, 11.49999999999998934 ) ) ;
#70093 = ADVANCED_FACE ( 'NONE', ( #6374 ), #55051, .T. ) ;
#70094 = ORIENTED_EDGE ( 'NONE', *, *, #60912, .T. ) ;
#70095 = B_SPLINE_CURVE_WITH_KNOTS ( 'NONE', 3,
 ( #14576, #75967, #85088, #46538, #84589, #37428 ),
 .UNSPECIFIED., .F., .F.,
 ( 4, 2, 4 ),
 ( 1.570887131794333942E-05, 0.001396322306279759555, 0.002776935741241575838 ),
 .UNSPECIFIED. ) ;
#70096 = AXIS2_PLACEMENT_3D ( 'NONE', #19049, #3355, #18551 ) ;
#70097 = CARTESIAN_POINT ( 'NONE',  ( -110.2723855490748122, -25.19526345475334850, 3.295595324081435074 ) ) ;
#70098 = APPROVAL_DATE_TIME ( #46765, #82835 ) ;
#70099 = ORIENTED_EDGE ( 'NONE', *, *, #23050, .F. ) ;
#70100 = CARTESIAN_POINT ( 'NONE',  ( 9.552245033349362461E-16, 23.99999999999999645, 0.000000000000000000 ) ) ;
#70101 = CARTESIAN_POINT ( 'NONE',  ( 17.47419131657910185, 0.3587747205144265483, 28.31804950686278843 ) ) ;
#70102 = CARTESIAN_POINT ( 'NONE',  ( -29.49875734969026198, -5.965225279485572685, 2.362022800118626531 ) ) ;
#70103 = DIRECTION ( 'NONE',  ( -3.773278334453080206E-23, 0.9999999999976377785, 2.173523156925979975E-06 ) ) ;
#70104 = FACE_OUTER_BOUND ( 'NONE', #58790, .T. ) ;
#70105 = CARTESIAN_POINT ( 'NONE',  ( -123.6228709571500559, -23.47593901973091235, -1.443836447538997536 ) ) ;
#70106 = CARTESIAN_POINT ( 'NONE',  ( -107.5875604241846730, -24.51314013834315730, 0.6176544820404215042 ) ) ;
#70107 = CARTESIAN_POINT ( 'NONE',  ( -16.75416981316412190, 10.96944243606782443, -1.500000000000002220 ) ) ;
#70108 = CARTESIAN_POINT ( 'NONE',  ( -99.49608100277511369, -25.10935113139711206, 3.179641471686016629 ) ) ;
#70109 = CARTESIAN_POINT ( 'NONE',  ( -45.62377148096768309, -25.00182538069146787, 7.747789668545045139 ) ) ;
#70110 = VERTEX_POINT ( 'NONE', #9359 ) ;
#70111 = AXIS2_PLACEMENT_3D ( 'NONE', #68713, #38243, #29140 ) ;
#70113 = PLANE ( 'NONE',  #16160 ) ;
#70112 = APPROVAL_PERSON_ORGANIZATION ( #88213, #22686, #35426 ) ;
#70114 = CARTESIAN_POINT ( 'NONE',  ( -110.0449441895338509, -25.29012733315208195, 3.330200468167525685 ) ) ;
#70115 = CARTESIAN_POINT ( 'NONE',  ( -74.62287095715005592, -23.48786465467241058, 11.44779295918254469 ) ) ;
#70116 = DIRECTION ( 'NONE',  ( 0.000000000000000000, 0.9999999999976377785, 2.173523156925979128E-06 ) ) ;
#70117 = DIRECTION ( 'NONE',  ( 0.000000000000000000, 1.000000000000000000, 0.000000000000000000 ) ) ;
#70118 = DIRECTION ( 'NONE',  ( 1.000000000000000000, -0.000000000000000000, 0.000000000000000000 ) ) ;
#70119 = CARTESIAN_POINT ( 'NONE',  ( -2.711489738547795625, -5.876774720514410966, 19.27798293355755632 ) ) ;
#70120 = VECTOR ( 'NONE', #79078, 1000.000000000000000 ) ;
#70121 = CARTESIAN_POINT ( 'NONE',  ( -40.52287095715006870, -24.51254535375849031, 9.355368624242066389 ) ) ;
#70122 = ORIENTED_EDGE ( 'NONE', *, *, #73868, .F. ) ;
#70123 = CARTESIAN_POINT ( 'NONE',  ( -2.359408512905806443, -20.17289352931189583, 11.49999999999998934 ) ) ;
#70124 = VECTOR ( 'NONE', #97123, 1000.000000000000000 ) ;
#70125 = FACE_OUTER_BOUND ( 'NONE', #6217, .T. ) ;
#70126 = DIRECTION ( 'NONE',  ( -0.000000000000000000, -0.000000000000000000, -1.000000000000000000 ) ) ;
#70127 = ORIENTED_EDGE ( 'NONE', *, *, #46621, .F. ) ;
#70128 = PLANE ( 'NONE',  #6447 ) ;
#70129 = CARTESIAN_POINT ( 'NONE',  ( -13.04681709000290013, -15.30929823114697541, -1.500000000000002220 ) ) ;
#70130 = CARTESIAN_POINT ( 'NONE',  ( -16.61111445048470614, -13.04167290785011701, 11.49999999999999645 ) ) ;
#70131 = CARTESIAN_POINT ( 'NONE',  ( -4.051365815588555463, -21.74199345402511696, 11.49999999999998934 ) ) ;
#70132 = CARTESIAN_POINT ( 'NONE',  ( -6.092534927433182368, -19.63929903328317295, 11.49999999999998934 ) ) ;
#70133 = AXIS2_PLACEMENT_3D ( 'NONE', #41387, #48507, #34279 ) ;
#70134 = EDGE_CURVE ( 'NONE', #39828, #26090, #35929, .T. ) ;
#70135 = LINE ( 'NONE', #83858, #98716 ) ;
#70136 = VERTEX_POINT ( 'NONE', #1761 ) ;
#70137 = DIRECTION ( 'NONE',  ( 0.000000000000000000, 0.9999999999976377785, 2.173523156925979975E-06 ) ) ;
#70138 = VERTEX_POINT ( 'NONE', #24580 ) ;
#70139 = CARTESIAN_POINT ( 'NONE',  ( -6.369015873774380943, -6.376774720514413630, 19.23384392940399934 ) ) ;
#70140 = CARTESIAN_POINT ( 'NONE',  ( -109.5228709571500616, -24.33927499327855415, 9.819080762295811837 ) ) ;
#70141 = ORIENTED_EDGE ( 'NONE', *, *, #78721, .F. ) ;
#70142 = ORIENTED_EDGE ( 'NONE', *, *, #53511, .F. ) ;
#70143 = ORIENTED_EDGE ( 'NONE', *, *, #32964, .F. ) ;
#70144 = DIRECTION ( 'NONE',  ( 1.334402673828313339E-16, 0.000000000000000000, -1.000000000000000000 ) ) ;
#70145 = CARTESIAN_POINT ( 'NONE',  ( -49.21454750704995007, -25.12863070112381791, 7.069183623698430452 ) ) ;
#70146 = CARTESIAN_POINT ( 'NONE',  ( -68.54922812267722065, -24.15620529776627734, 10.23563542870660825 ) ) ;
#70147 = CARTESIAN_POINT ( 'NONE',  ( -3.285303218690974525, -20.39892020120133154, -1.500000000000002220 ) ) ;
#70148 = CARTESIAN_POINT ( 'NONE',  ( 7.158504886898216846, -20.39052948596947346, 11.49999999999999645 ) ) ;
#70149 = ORIENTED_EDGE ( 'NONE', *, *, #7158, .F. ) ;
#70150 = CIRCLE ( 'NONE', #8597, 0.2999999999999981570 ) ;
#70151 = ADVANCED_FACE ( 'NONE', ( #79370 ), #72279, .F. ) ;
#70152 = CYLINDRICAL_SURFACE ( 'NONE', #9352, 3.349999999999998757 ) ;
#70153 = CARTESIAN_POINT ( 'NONE',  ( 2.884397429187188333, -5.876774720514406525, 18.67943752795919110 ) ) ;
#70154 = CARTESIAN_POINT ( 'NONE',  ( -16.90645664988545249, 14.66980924573920397, -1.500000000000002220 ) ) ;
#70155 = EDGE_CURVE ( 'NONE', #98626, #6678, #78362, .T. ) ;
#70156 = EDGE_CURVE ( 'NONE', #94109, #63282, #72242, .T. ) ;
#70157 = CARTESIAN_POINT ( 'NONE',  ( -47.62369827702862324, -24.66019654487199730, 8.947790411086117501 ) ) ;
#70158 = DIRECTION ( 'NONE',  ( 0.000000000000000000, 1.000000000000000000, 0.000000000000000000 ) ) ;
#70159 = ORIENTED_EDGE ( 'NONE', *, *, #22832, .F. ) ;
#70160 = CARTESIAN_POINT ( 'NONE',  ( -117.5798424949460923, -25.31863975941917388, 6.461805294873899541 ) ) ;
#70161 = CARTESIAN_POINT ( 'NONE',  ( -120.6228709571500559, -25.00182538069145721, 7.747789668545100206 ) ) ;
#70162 = EDGE_CURVE ( 'NONE', #65127, #93325, #32392, .T. ) ;
#70163 = CARTESIAN_POINT ( 'NONE',  ( 13.94627346685978075, -15.57361473980792255, 11.49999999999998934 ) ) ;
#70164 = ORIENTED_EDGE ( 'NONE', *, *, #92769, .T. ) ;
#70165 = DIRECTION ( 'NONE',  ( 0.000000000000000000, -0.000000000000000000, -1.000000000000000000 ) ) ;
#70166 = EDGE_LOOP ( 'NONE', ( #6343, #64803, #62598, #62822 ) ) ;
#70167 = FACE_OUTER_BOUND ( 'NONE', #25857, .T. ) ;
#70168 = CARTESIAN_POINT ( 'NONE',  ( 16.91677535067316995, -12.78530099663392505, -1.500000000000002220 ) ) ;
#70169 = ORIENTED_EDGE ( 'NONE', *, *, #88650, .F. ) ;
#70170 = CARTESIAN_POINT ( 'NONE',  ( -79.52287095715006160, -24.64965694238575011, 8.947790433994198267 ) ) ;
#70171 = CARTESIAN_POINT ( 'NONE',  ( 19.81658424304261246, 9.080307684375437560, 11.49999999999998934 ) ) ;
#70172 = LINE ( 'NONE', #22476, #56265 ) ;
#70173 = PLANE ( 'NONE',  #72897 ) ;
#70174 = CARTESIAN_POINT ( 'NONE',  ( -35.52287095715006160, -24.91570333825474037, 8.075032458260901436 ) ) ;
#70175 = CARTESIAN_POINT ( 'NONE',  ( 20.57308398666954119, -7.222494929537193187, -1.500000000000002220 ) ) ;
#70176 = CARTESIAN_POINT ( 'NONE',  ( -30.57287095715005876, -25.25639193976267194, 6.126332763130458936 ) ) ;
#70177 = ORIENTED_EDGE ( 'NONE', *, *, #76107, .F. ) ;
#70178 = CARTESIAN_POINT ( 'NONE',  ( 11.13529270535513760, -4.132774720514426292, -26.87372982997969117 ) ) ;
#70179 = FACE_OUTER_BOUND ( 'NONE', #54678, .T. ) ;
#70180 = ADVANCED_FACE ( 'NONE', ( #63169 ), #94094, .T. ) ;
#70181 = ORIENTED_EDGE ( 'NONE', *, *, #3964, .F. ) ;
#70182 = VERTEX_POINT ( 'NONE', #63680 ) ;
#70183 = AXIS2_PLACEMENT_3D ( 'NONE', #61995, #77689, #21901 ) ;
#70184 = ADVANCED_FACE ( 'NONE', ( #10363 ), #64687, .T. ) ;
#70185 = ORIENTED_EDGE ( 'NONE', *, *, #17580, .T. ) ;
#70186 = ORGANIZATION ( 'NAUO-ORG7', 'UNSPECIFIED', 'UNSPECIFIED' ) ;
#70187 = CARTESIAN_POINT ( 'NONE',  ( -28.24811442358726410, -24.84257439951912616, 2.397443450879609639 ) ) ;
#70188 = DIRECTION ( 'NONE',  ( 0.000000000000000000, 0.000000000000000000, -1.000000000000000000 ) ) ;
#70189 = CARTESIAN_POINT ( 'NONE',  ( 4.903939382885006637, -20.63555827282145572, -1.500000000000002220 ) ) ;
#70190 = CARTESIAN_POINT ( 'NONE',  ( -79.52287095715006160, -24.65952944569304961, 1.056160979905698794 ) ) ;
#70191 = FACE_OUTER_BOUND ( 'NONE', #12749, .T. ) ;
#70192 = EDGE_CURVE ( 'NONE', #1913, #4586, #90385, .T. ) ;
#70193 = CARTESIAN_POINT ( 'NONE',  ( 20.98059139286874242, -4.383336229084510371, -17.13711341628515328 ) ) ;
#70194 = CARTESIAN_POINT ( 'NONE',  ( -128.5228709571500758, -23.47593901973090524, -1.443836447538996204 ) ) ;
#70196 = CARTESIAN_POINT ( 'NONE',  ( 17.66168439605153395, -8.020940556088177686, 11.49999999999998934 ) ) ;
#70195 = CIRCLE ( 'NONE', #83150, 6.594667762285749468 ) ;
#70197 = CARTESIAN_POINT ( 'NONE',  ( -41.89292675774235875, -25.11539320593059443, 2.804431443241629740 ) ) ;
#70198 = ORIENTED_EDGE ( 'NONE', *, *, #39000, .F. ) ;
#70199 = CARTESIAN_POINT ( 'NONE',  ( -7.634514033349506512, -17.95459398628807435, 11.49999999999999645 ) ) ;
#70200 = CARTESIAN_POINT ( 'NONE',  ( -34.58953762381671737, -23.48783264082478084, -1.443836473390074149 ) ) ;
#70201 = AXIS2_PLACEMENT_3D ( 'NONE', #43962, #57703, #96749 ) ;
#70202 = B_SPLINE_CURVE_WITH_KNOTS ( 'NONE', 3,
 ( #65963, #26873, #42117, #80659 ),
 .UNSPECIFIED., .F., .F.,
 ( 4, 4 ),
 ( 0.000000000000000000, 9.999999999998897304E-05 ),
 .UNSPECIFIED. ) ;
#70203 = CARTESIAN_POINT ( 'NONE',  ( 1.754398552524170762, 17.92127466780477718, -9.000000000000000000 ) ) ;
#70204 = ORIENTED_EDGE ( 'NONE', *, *, #37682, .T. ) ;
#70205 = EDGE_CURVE ( 'NONE', #51748, #82017, #6458, .T. ) ;
#70206 = CARTESIAN_POINT ( 'NONE',  ( -103.6228709571500417, -23.47596703998600631, 11.44779298504227860 ) ) ;
#70207 = CARTESIAN_POINT ( 'NONE',  ( 8.978253834636468866, -5.876774720514426953, 0.000000000000000000 ) ) ;
#70209 = EDGE_CURVE ( 'NONE', #96384, #125, #58947, .T. ) ;
#70208 = DIRECTION ( 'NONE',  ( 1.000000000000000000, 3.773278334444167608E-23, 8.201307833595939069E-29 ) ) ;
#70210 = CARTESIAN_POINT ( 'NONE',  ( -93.54679903806243146, -24.51419770103157703, 9.386484678747164523 ) ) ;
#70211 = CARTESIAN_POINT ( 'NONE',  ( 19.59260286812380514, -1.442238090573773501, 11.49999999999998934 ) ) ;
#70212 = B_SPLINE_SURFACE_WITH_KNOTS ( 'NONE', 3, 3, ( 
 ( #47468, #2804, #70807, #87020 ),
 ( #33741, #48476, #64722, #18506 ),
 ( #47969, #78894, #49480, #63715 ),
 ( #41353, #1296, #40844, #32229 ),
 ( #80410, #10395, #56087, #72307 ),
 ( #79403, #63203, #71811, #33232 ),
 ( #94126, #64212, #25624, #56596 ) ),
 .UNSPECIFIED., .F., .F., .F.,
 ( 4, 3, 4 ),
 ( 4, 4 ),
 ( 0.7945040050992243641, 0.8970133687736502326, 0.9995227324480761011 ),
 ( 0.4396057071469119393, 0.4408213828681695756 ),
 .UNSPECIFIED. ) ;
#70213 = CARTESIAN_POINT ( 'NONE',  ( -41.46533095918948675, -25.31583583508971813, 4.218578428352230070 ) ) ;
#70214 = EDGE_LOOP ( 'NONE', ( #36063, #40473, #87541, #82516 ) ) ;
#70215 = CARTESIAN_POINT ( 'NONE',  ( -21.50746323947805649, 1.722430922125298247, 11.49999999999998934 ) ) ;
#70216 = CARTESIAN_POINT ( 'NONE',  ( -40.48566607648301385, -24.52300882791530157, 0.6510814631126360386 ) ) ;
#70217 = EDGE_CURVE ( 'NONE', #14465, #41863, #58549, .T. ) ;
#70218 = DIRECTION ( 'NONE',  ( 1.000000000000000000, 0.000000000000000000, 0.000000000000000000 ) ) ;
#70219 = CARTESIAN_POINT ( 'NONE',  ( 21.63105218614105851, 7.968772182826888262, -1.500000000000002220 ) ) ;
#70220 = CALENDAR_DATE ( 2026, 9, 10 ) ;
#70221 = CARTESIAN_POINT ( 'NONE',  ( -93.62801744632055545, -24.34968618360934300, 0.1864209137778838898 ) ) ;
#70222 = CARTESIAN_POINT ( 'NONE',  ( -115.5895376238167245, -23.47593901973091235, -1.443836447538997536 ) ) ;
#70223 = CARTESIAN_POINT ( 'NONE',  ( -121.6267055903540637, -23.73791477778912196, 11.05961554403169878 ) ) ;
#70224 = CARTESIAN_POINT ( 'NONE',  ( -101.1710158166120692, -25.07377586470730790, 7.416935156559355313 ) ) ;
#70226 = B_SPLINE_CURVE_WITH_KNOTS ( 'NONE', 3,
 ( #51160, #43055, #81107, #35930 ),
 .UNSPECIFIED., .F., .F.,
 ( 4, 4 ),
 ( 0.6302359605503721207, 0.6392423918224876545 ),
 .UNSPECIFIED. ) ;
#70225 = CARTESIAN_POINT ( 'NONE',  ( 5.641653616409716854, -6.376774720514420736, 20.81030773351227481 ) ) ;
#70227 = CARTESIAN_POINT ( 'NONE',  ( -129.5561477353246005, -23.48783264082477729, -1.443836473390078590 ) ) ;
#70228 = CARTESIAN_POINT ( 'NONE',  ( -99.52609871227460303, -25.31566080173880451, 4.842596112347664850 ) ) ;
#70229 = CARTESIAN_POINT ( 'NONE',  ( -16.62890364678930410, -10.96057169749504645, -1.500000000000002220 ) ) ;
#70230 = CARTESIAN_POINT ( 'NONE',  ( 25.83488407601164383, 2.682774720514426559, -11.31196583263649558 ) ) ;
#70231 = CARTESIAN_POINT ( 'NONE',  ( 15.56394622224390645, 12.30447529683395125, -1.500000000000002220 ) ) ;
#70232 = CARTESIAN_POINT ( 'NONE',  ( 0.1739078616027790736, -5.876774720514415407, 19.75705121608222115 ) ) ;
#70233 = VECTOR ( 'NONE', #76699, 1000.000000000000000 ) ;
#70234 = LINE ( 'NONE', #7827, #100291 ) ;
#70235 = CARTESIAN_POINT ( 'NONE',  ( -92.52287095715009002, -24.66019654487200086, 8.947790411086115725 ) ) ;
#70236 = CARTESIAN_POINT ( 'NONE',  ( 14.12806351585482112, -15.20395780304818523, 11.49999999999999645 ) ) ;
#70237 = LINE ( 'NONE', #39773, #3025 ) ;
#70238 = B_SPLINE_CURVE_WITH_KNOTS ( 'NONE', 3,
 ( #38018, #75568, #46646, #98909 ),
 .UNSPECIFIED., .F., .F.,
 ( 4, 4 ),
 ( 0.5691783989504385355, 0.5701791459912038951 ),
 .UNSPECIFIED. ) ;
#70239 = CARTESIAN_POINT ( 'NONE',  ( -40.52287095715005449, -24.99132157543166244, 2.256160258750667502 ) ) ;
#70240 = CARTESIAN_POINT ( 'NONE',  ( 15.15630024635751383, 17.02982414992789018, 11.49999999999999645 ) ) ;
#70241 = ORIENTED_EDGE ( 'NONE', *, *, #32854, .T. ) ;
#70242 = CARTESIAN_POINT ( 'NONE',  ( -69.59707441095807212, -23.96119346886880308, -0.6495511937832122440 ) ) ;
#70243 = DIRECTION ( 'NONE',  ( 0.000000000000000000, -1.000000000000000000, 0.000000000000000000 ) ) ;
#70244 = ORIENTED_EDGE ( 'NONE', *, *, #4063, .F. ) ;
#70245 = CARTESIAN_POINT ( 'NONE',  ( 15.73562052650688514, -12.66937975264744587, -1.500000000000002220 ) ) ;
#70246 = CARTESIAN_POINT ( 'NONE',  ( 27.53860345374808105, -4.772774720514425972, -8.321925749325261634 ) ) ;
#70247 = CARTESIAN_POINT ( 'NONE',  ( -2.701720430790311767, -5.965225279485594001, -28.90526747363640681 ) ) ;
#70248 = EDGE_LOOP ( 'NONE', ( #53873, #87424, #74360, #56227 ) ) ;
#70249 = ORIENTED_EDGE ( 'NONE', *, *, #2249, .F. ) ;
#70250 = VECTOR ( 'NONE', #61272, 1000.000000000000114 ) ;
#70251 = LINE ( 'NONE', #31687, #66301 ) ;
#70252 = CARTESIAN_POINT ( 'NONE',  ( 7.980177114813061579, 21.45908683785374649, -1.500000000000002220 ) ) ;
#70253 = CARTESIAN_POINT ( 'NONE',  ( -51.29636648399702636, -25.27420710014245131, 3.969959656738967446 ) ) ;
#70254 = CARTESIAN_POINT ( 'NONE',  ( 15.40532884848888884, -15.22192433072940609, -1.500000000000002220 ) ) ;
#70255 = CARTESIAN_POINT ( 'NONE',  ( -99.64934318012689118, -25.31535474791540707, 4.927356294767410105 ) ) ;
#70256 = CARTESIAN_POINT ( 'NONE',  ( 17.12911088700535700, -11.98135219954639830, 11.49999999999999645 ) ) ;
#70257 = VERTEX_POINT ( 'NONE', #81377 ) ;
#70258 = CARTESIAN_POINT ( 'NONE',  ( -107.6228709571500701, -24.33927499327855415, 9.819080762295817166 ) ) ;
#70259 = CARTESIAN_POINT ( 'NONE',  ( -69.15592802969443653, -25.31612547948029146, 5.438241754530615424 ) ) ;
#70260 = CARTESIAN_POINT ( 'NONE',  ( -14.94409825380703616, 16.19114737329946507, 11.49999999999998934 ) ) ;
#70261 = LINE ( 'NONE', #78356, #62472 ) ;
#70262 = CARTESIAN_POINT ( 'NONE',  ( 32.16024265030974050, 5.965225279485572685, 14.03360796525321774 ) ) ;
#70263 = AXIS2_PLACEMENT_3D ( 'NONE', #32908, #25283, #63378 ) ;
#70264 = VERTEX_POINT ( 'NONE', #50938 ) ;
#70265 = CARTESIAN_POINT ( 'NONE',  ( -49.59807878744301490, -25.27344843023344012, 3.677862403480164133 ) ) ;
#70266 = CARTESIAN_POINT ( 'NONE',  ( -122.6228709571500701, -24.33927499327855415, 9.819080762295815390 ) ) ;
#70267 = ORIENTED_EDGE ( 'NONE', *, *, #57378, .T. ) ;
#70268 = CARTESIAN_POINT ( 'NONE',  ( -72.60176318579898691, -23.73791477778911840, 11.05961554403170943 ) ) ;
#70269 = ADVANCED_FACE ( 'NONE', ( #59547 ), #90485, .F. ) ;
#70270 = VERTEX_POINT ( 'NONE', #97102 ) ;
#70271 = VECTOR ( 'NONE', #7284, 1000.000000000000114 ) ;
#70272 = EDGE_CURVE ( 'NONE', #82699, #47065, #89987, .T. ) ;
#70273 = ORIENTED_EDGE ( 'NONE', *, *, #25480, .F. ) ;
#70274 = CARTESIAN_POINT ( 'NONE',  ( -106.6228709571500843, -24.34917612406837506, 0.1852690917426655925 ) ) ;
#70275 = B_SPLINE_CURVE_WITH_KNOTS ( 'NONE', 3,
 ( #7290, #97284, #12542, #20646, #30634, #61610 ),
 .UNSPECIFIED., .F., .F.,
 ( 4, 2, 4 ),
 ( 0.000000000000000000, 0.001380901958385381172, 0.002761803916770762344 ),
 .UNSPECIFIED. ) ;
#70276 = PLANE ( 'NONE',  #47001 ) ;
#70277 = CARTESIAN_POINT ( 'NONE',  ( -36.58683833660532514, -24.34968618360933590, 0.1864209137778783110 ) ) ;
#70278 = CARTESIAN_POINT ( 'NONE',  ( -15.50425215161893355, 13.37805140191733777, -1.500000000000002220 ) ) ;
#70279 = ADVANCED_FACE ( 'NONE', ( #42831 ), #73761, .T. ) ;
#70280 = ORIENTED_EDGE ( 'NONE', *, *, #19652, .T. ) ;
#70281 = LINE ( 'NONE', #47947, #91429 ) ;
#70282 = B_SPLINE_CURVE_WITH_KNOTS ( 'NONE', 3,
 ( #75215, #66143, #43783, #19434, #89452, #49911, #34673, #42307, #35174, #73236, #36658, #13306, #82825, #44286, #74710, #97060, #27563, #3729, #51395, #65643, #58021, #36168, #96557, #27058, #50399, #66644, #67133, #29039, #82333, #81341, #11822, #12809, #67624, #98044, #98543, #28539, #42793, #73725, #90942, #35671, #4220, #58515, #19930, #50899, #81838, #12311, #4721, #43291, #97557, #28057, #59015, #89947, #20416, #59507 ),
 .UNSPECIFIED., .F., .F.,
 ( 4, 1, 1, 1, 1, 2, 2, 1, 2, 2, 1, 1, 2, 2, 1, 2, 2, 2, 1, 2, 2, 1, 1, 1, 1, 2, 2, 2, 2, 1, 1, 1, 2, 2, 4 ),
 ( 0.000000000000000000, 0.06249999999999557299, 0.09374999999999336642, 0.1093749999999920897, 0.1171874999999916039, 0.1210937499999911876, 0.1249999999999907713, 0.1562499999999895361, 0.1718749999999889255, 0.1874999999999883149, 0.2187499999999874545, 0.2343749999999873157, 0.2421874999999875377, 0.2499999999999877875, 0.3124999999999897304, 0.3437499999999905076, 0.3749999999999912847, 0.4999999999999942268, 0.5624999999999956701, 0.5937499999999965583, 0.6249999999999974465, 0.6874999999999988898, 0.7187499999999996669, 0.7343750000000001110, 0.7421875000000003331, 0.7460937500000005551, 0.7500000000000006661, 0.7812500000000013323, 0.8125000000000018874, 0.8437500000000024425, 0.8593750000000027756, 0.8671875000000028866, 0.8710937500000027756, 0.8750000000000027756, 1.000000000000000000 ),
 .UNSPECIFIED. ) ;
#70283 = CARTESIAN_POINT ( 'NONE',  ( 0.000000000000000000, -4.056774720514426669, 6.000000000000000888 ) ) ;
#70284 = DIRECTION ( 'NONE',  ( -0.9890158633619159367, -0.1478094111296165691, -0.000000000000000000 ) ) ;
#70285 = CARTESIAN_POINT ( 'NONE',  ( 4.546662993595487201, 21.82331882591909178, 11.49999999999998934 ) ) ;
#70286 = EDGE_CURVE ( 'NONE', #25620, #48372, #12849, .T. ) ;
#70287 = CARTESIAN_POINT ( 'NONE',  ( -70.90788765031213359, -25.16125207327868196, 6.936007712053442020 ) ) ;
#70288 = CARTESIAN_POINT ( 'NONE',  ( -27.23878724382540284, -24.61900095434126712, 8.198000781698828732 ) ) ;
#70289 = ORIENTED_EDGE ( 'NONE', *, *, #22256, .T. ) ;
#70290 = CARTESIAN_POINT ( 'NONE',  ( -111.6228709571500559, -24.65952944569304606, 1.056160979905703901 ) ) ;
#70291 = CARTESIAN_POINT ( 'NONE',  ( -29.79716636085243664, -24.63645471362255890, 5.521953888132082433 ) ) ;
#70292 = CARTESIAN_POINT ( 'NONE',  ( 13.71216040526616098, 15.69570726272272232, 11.49999999999998934 ) ) ;
#70293 = ORIENTED_EDGE ( 'NONE', *, *, #11154, .T. ) ;
#70295 = ORIENTED_EDGE ( 'NONE', *, *, #52113, .T. ) ;
#70294 = CARTESIAN_POINT ( 'NONE',  ( -116.5228709571500900, -23.73907113217699560, -1.053371485780731254 ) ) ;
#70296 = ORIENTED_EDGE ( 'NONE', *, *, #94823, .T. ) ;
#70297 = B_SPLINE_SURFACE_WITH_KNOTS ( 'NONE', 3, 1, ( 
 ( #13897, #5797 ),
 ( #91527, #36256 ),
 ( #59600, #99132 ),
 ( #51983, #99623 ),
 ( #28640, #82911 ),
 ( #61605, #44875 ),
 ( #45865, #38236 ),
 ( #6296, #98632 ),
 ( #69192, #75798 ),
 ( #76293, #37256 ),
 ( #29132, #30625 ),
 ( #14397, #68204 ),
 ( #100111, #60606 ),
 ( #30124, #92522 ),
 ( #21505, #90531 ),
 ( #5298, #92026 ),
 ( #22001, #84417 ),
 ( #76781, #7285 ),
 ( #45377, #52983 ),
 ( #22995, #67220 ),
 ( #53984, #44374 ),
 ( #13399, #84911 ),
 ( #43869, #75299 ),
 ( #68705, #36753 ),
 ( #67719, #60107 ),
 ( #91031, #61099 ),
 ( #52481, #182 ),
 ( #71705, #47868 ),
 ( #679, #17409 ),
 ( #15395, #31625 ),
 ( #62591, #48368 ),
 ( #2202, #93516 ),
 ( #24512, #47362 ),
 ( #77784, #77288 ),
 ( #7789, #55991 ),
 ( #86418, #38734 ),
 ( #70694, #78788 ),
 ( #86916, #69701 ),
 ( #46357, #39238 ),
 ( #16395, #63099 ),
 ( #25523, #31124 ),
 ( #24011, #56495 ),
 ( #94027, #63606 ),
 ( #79299, #62097 ),
 ( #15897, #93017 ),
 ( #94528, #70196 ),
 ( #16905, #85921 ),
 ( #9795, #33132 ),
 ( #23495, #54474 ),
 ( #9285, #85411 ),
 ( #40747, #54978 ),
 ( #64111, #55481 ),
 ( #95032, #46860 ),
 ( #8292, #78292 ),
 ( #8799, #39738 ),
 ( #1190, #32126 ),
 ( #40251, #71201 ),
 ( #1695, #32629 ),
 ( #25011, #82674 ),
 ( #33640, #17915 ),
 ( #48873, #44124 ),
 ( #41765, #20762 ),
 ( #95533, #11297 ),
 ( #64620, #44622 ),
 ( #79800, #96035 ),
 ( #51739, #57494 ),
 ( #73208, #90794 ),
 ( #13153, #72709 ),
 ( #10297, #28384 ),
 ( #6051, #75547 ),
 ( #49882, #26529 ),
 ( #65113, #2697 ),
 ( #41254, #36498 ),
 ( #42279, #98388 ),
 ( #67463, #28891 ),
 ( #59344, #36001 ),
 ( #37004, #72208 ),
 ( #21263, #87926 ),
 ( #5551, #67969 ),
 ( #98893, #26019 ),
 ( #88428, #29387 ),
 ( #3206, #66976 ),
 ( #56989, #75051 ),
 ( #97889, #18410 ),
 ( #87416, #59857 ),
 ( #34148, #52238 ),
 ( #49378, #18901 ),
 ( #80813, #83166 ),
 ( #13650, #80309 ),
 ( #10800, #3696 ),
 ( #90292, #62352 ),
 ( #52732, #93277 ),
 ( #99877, #38504 ),
 ( #15661, #8050 ),
 ( #23770, #61856 ),
 ( #92778, #31391 ),
 ( #92282, #83672 ),
 ( #38999, #23261 ),
 ( #77548, #53742 ),
 ( #46125, #54744 ),
 ( #54244, #45623 ),
 ( #30888, #84671 ),
 ( #85680, #15158 ),
 ( #46630, #16159 ),
 ( #38004, #76053 ),
 ( #91290, #69949 ),
 ( #77050, #437 ),
 ( #22757, #76543 ),
 ( #39508, #47128 ),
 ( #68953, #7052 ),
 ( #78043, #8556 ),
 ( #70459, #943 ),
 ( #14152, #60365 ),
 ( #7553, #21759 ),
 ( #14660, #69453 ),
 ( #99394, #45130 ),
 ( #100375, #6555 ),
 ( #37503, #85172 ),
 ( #30385, #68458 ),
 ( #29889, #61358 ),
 ( #60856, #91775 ),
 ( #22258, #53239 ),
 ( #84169, #16658 ),
 ( #33891, #31894 ),
 ( #79564, #72464 ),
 ( #70963, #64876 ),
 ( #80066, #56252 ),
 ( #55248, #41509 ),
 ( #41014, #71468 ),
 ( #32899, #10052 ),
 ( #42020, #47629 ),
 ( #48129, #72965 ),
 ( #71969, #10550 ),
 ( #26278, #87177 ),
 ( #1956, #18657 ),
 ( #1454, #2957 ),
 ( #17665, #55749 ),
 ( #80562, #63870 ),
 ( #94785, #17162 ),
 ( #11056, #88186 ),
 ( #9550, #79057 ),
 ( #32393, #2450 ),
 ( #49632, #95787 ),
 ( #86175, #87682 ),
 ( #48637, #62869 ),
 ( #86674, #33384 ),
 ( #63369, #18166 ),
 ( #64372, #78547 ),
 ( #9051, #40003 ),
 ( #95293, #25777 ),
 ( #56752, #93785 ),
 ( #57255, #94283 ),
 ( #24280, #24766 ),
 ( #40517, #25272 ),
 ( #49138, #3458 ),
 ( #51117, #43995 ),
 ( #42520, #5433 ),
 ( #51618, #27775 ),
 ( #26780, #13035 ),
 ( #12544, #43013 ),
 ( #4452, #82061 ),
 ( #19155, #58725 ),
 ( #11545, #59229 ),
 ( #88685, #81066 ),
 ( #21146, #73956 ),
 ( #74927, #98266 ),
 ( #66361, #58239 ),
 ( #28773, #73458 ),
 ( #13531, #50125 ),
 ( #97287, #34393 ),
 ( #52117, #66855 ),
 ( #90668, #89677 ),
 ( #43510, #97777 ),
 ( #34896, #65371 ),
 ( #65869, #36383 ),
 ( #83040, #20152 ),
 ( #74448, #3951 ),
 ( #90174, #12043 ),
 ( #96788, #67347 ),
 ( #35885, #27284 ),
 ( #59735, #35403 ),
 ( #44503, #4940 ),
 ( #89181, #19651 ),
 ( #50616, #81569 ),
 ( #28271, #96293 ),
 ( #57745, #20648 ),
 ( #82553, #91658 ),
 ( #67848, #315 ),
 ( #7422, #62231 ),
 ( #85044, #83548 ),
 ( #14533, #37389 ),
 ( #75427, #22137 ),
 ( #52609, #99270 ),
 ( #16029, #45508 ),
 ( #23132, #69327 ),
 ( #21636, #5928 ),
 ( #36882, #30763 ),
 ( #29769, #77421 ),
 ( #76423, #76921 ),
 ( #93150, #6928 ),
 ( #60238, #54121 ),
 ( #38374, #37882 ),
 ( #61237, #7924 ),
 ( #100247, #60734 ),
 ( #98768, #15032 ),
 ( #23639, #54610 ),
 ( #68835, #99753 ),
 ( #61735, #14027 ),
 ( #15530, #30257 ),
 ( #92156, #85546 ),
 ( #22632, #53623 ),
 ( #46003, #84547 ),
 ( #29266, #91164 ),
 ( #38872, #75929 ),
 ( #92653, #31260 ),
 ( #45010, #6434 ),
 ( #46494, #68337 ),
 ( #69833, #53121 ),
 ( #84051, #8926 ),
 ( #94662, #39378 ),
 ( #62737, #1828 ),
 ( #88062, #17035 ),
 ( #95168, #40880 ),
 ( #93653, #77919 ),
 ( #8428, #2331 ),
 ( #70835, #49005 ),
 ( #48003, #48506 ),
 ( #33771, #78927 ),
 ( #31768, #25653 ),
 ( #24147, #64246 ),
 ( #79434, #9421 ),
 ( #71840, #32262 ),
 ( #70333, #87050 ),
 ( #64754, #95670 ),
 ( #40385, #86550 ),
 ( #33260, #86050 ),
 ( #56626, #71337 ),
 ( #32763, #26153 ),
 ( #63745, #25142 ),
 ( #55114, #57126 ),
 ( #46995, #24640 ),
 ( #79936, #47498 ),
 ( #87555, #2834 ),
 ( #10425, #18041 ),
 ( #56124, #815 ),
 ( #41386, #78427 ),
 ( #39877, #17540 ),
 ( #9926, #16525 ),
 ( #72342, #1327 ),
 ( #63233, #94156 ),
 ( #55621, #58609 ),
 ( #34772, #51498 ),
 ( #59116, #5309 ),
 ( #28158, #90053 ),
 ( #10932, #20525 ),
 ( #51002, #66243 ),
 ( #41899, #57621 ),
 ( #82431, #12914 ),
 ( #19533, #28653 ),
 ( #43882, #19035 ),
 ( #50010, #50495 ),
 ( #27662, #3342 ),
 ( #74815, #81937 ),
 ( #3831, #36270 ),
 ( #18539, #65742 ),
 ( #96663, #67231 ),
 ( #98145, #59613 ),
 ( #49509, #80443 ),
 ( #72842, #34278 ),
 ( #12421, #97168 ),
 ( #65250, #88562 ),
 ( #66743, #42891 ),
 ( #96174, #26660 ),
 ( #89554, #58123 ),
 ( #81449, #20039 ),
 ( #80944, #11429 ),
 ( #11927, #42406 ),
 ( #27160, #73338 ),
 ( #89060, #73827 ),
 ( #43390, #4328 ),
 ( #35278, #74329 ),
 ( #4820, #35773 ),
 ( #97658, #77303 ),
 ( #13412, #75312 ),
 ( #7804, #53505 ),
 ( #83423, #22511 ),
 ( #21025, #44889 ),
 ( #61111, #7297 ),
 ( #14411, #44386 ),
 ( #45388, #14907 ),
 ( #15409, #194 ),
 ( #61617, #100123 ),
 ( #13911, #76303 ),
 ( #29644, #6802 ),
 ( #75810, #98646 ),
 ( #46370, #38748 ),
 ( #37266, #37758 ),
 ( #30643, #92535 ),
 ( #53996, #69716 ),
 ( #31139, #92039 ),
 ( #84428, #68716 ),
 ( #90545, #68217 ),
 ( #60618, #51994 ),
 ( #29145, #23008 ),
 ( #99633, #6311 ),
 ( #82924, #91539 ),
 ( #53000, #99144 ),
 ( #5809, #36767 ),
 ( #22013, #83930 ),
 ( #67731, #84926 ),
 ( #60118, #91044 ),
 ( #21517, #52494 ),
 ( #30137, #45880 ),
 ( #76796, #38249 ),
 ( #69208, #56506 ),
 ( #54486, #70211 ),
 ( #39251, #46876 ),
 ( #25029, #1709 ),
 ( #32643, #41267 ),
 ( #47379, #62608 ),
 ( #17928, #8813 ),
 ( #33144, #77796 ),
 ( #64127, #62109 ),
 ( #9298, #2215 ),
 ( #692, #95045 ),
 ( #94541, #48885 ),
 ( #23509, #8308 ),
 ( #85934, #25537 ),
 ( #78305, #93030 ),
 ( #2713, #31637 ),
 ( #39749, #85424 ),
 ( #93529, #24023 ),
 ( #79813, #1207 ),
 ( #87430, #10311 ),
 ( #24524, #16406 ),
 ( #72220, #54993 ),
 ( #15909, #70709 ),
 ( #55493, #32138 ),
 ( #63114, #56003 ),
 ( #94040, #47881 ),
 ( #86433, #16918 ),
 ( #78800, #40264 ),
 ( #71215, #63619 ),
 ( #86929, #17422 ),
 ( #48381, #79314 ),
 ( #9809, #40760 ),
 ( #71719, #65625 ),
 ( #96542, #26031 ),
 ( #97540, #10812 ),
 ( #42776, #97044 ),
 ( #43762, #73709 ),
 ( #49894, #66625 ),
 ( #89932, #80828 ),
 ( #4202, #27038 ),
 ( #96049, #95547 ),
 ( #57004, #74212 ),
 ( #35156, #87939 ),
 ( #88939, #66127 ),
 ( #4702, #18423 ),
 ( #64633, #57507 ),
 ( #58007, #18915 ),
 ( #74695, #49393 ),
 ( #19416, #41781 ),
 ( #11311, #80321 ),
 ( #35653, #51375 ),
 ( #11804, #28037 ),
 ( #81821, #88442 ),
 ( #27543, #3710 ),
 ( #58996, #20398 ),
 ( #72721, #3222 ),
 ( #58501, #34159 ),
 ( #26543, #89435 ),
 ( #65126, #42292 ),
 ( #19909, #50883 ),
 ( #50383, #73220 ),
 ( #81322, #12293 ),
 ( #82314, #33653 ),
 ( #34656, #43270 ),
 ( #12792, #67607 ),
 ( #14787, #6686 ),
 ( #90926, #13289 ),
 ( #68594, #44762 ),
 ( #6186, #52874 ),
 ( #15288, #20903 ),
 ( #37137, #44265 ),
 ( #21393, #90428 ),
 ( #7179, #22884 ),
 ( #83809, #76674 ),
 ( #36149, #68099 ),
 ( #37635, #100009 ),
 ( #29517, #46254 ),
 ( #28524, #51878 ),
 ( #99517, #82806 ),
 ( #98524, #30017 ),
 ( #67114, #59994 ),
 ( #76185, #22392 ),
 ( #60498, #59486 ),
 ( #91414, #60988 ),
 ( #30523, #5190 ),
 ( #75195, #5688 ),
 ( #53377, #29022 ),
 ( #75687, #21892 ),
 ( #52371, #36639 ),
 ( #61489, #53872 ),
 ( #83305, #14289 ),
 ( #45753, #38129 ),
 ( #84806, #99021 ),
 ( #91921, #98025 ),
 ( #92414, #45260 ),
 ( #84301, #13789 ),
 ( #69083, #85817 ),
 ( #85306, #40655 ),
 ( #61986, #86316 ),
 ( #16801, #87315 ),
 ( #56394, #16297 ),
 ( #77681, #39134 ),
 ( #23909, #8195 ),
 ( #8700, #17813 ),
 ( #38634, #46759 ),
 ( #17303, #93414 ),
 ( #69598, #2103 ),
 ( #64017, #48268 ),
 ( #23389, #7687 ),
 ( #32027, #86816 ),
 ( #55889, #79198 ),
 ( #47766, #24412 ),
 ( #25420, #76 ),
 ( #9696, #70092 ),
 ( #94425, #33037 ),
 ( #94932, #31021 ),
 ( #92913, #63001 ),
 ( #71606, #575 ),
 ( #31522, #39637 ),
 ( #70593, #54375 ),
 ( #77181, #9187 ),
 ( #62488, #15794 ),
 ( #54877, #47262 ),
 ( #78187, #1086 ),
 ( #93921, #55379 ),
 ( #78681, #40148 ),
 ( #71103, #1593 ),
 ( #32530, #63506 ),
 ( #24911, #41158 ),
 ( #3598, #81210 ),
 ( #89324, #10199 ),
 ( #79702, #72608 ),
 ( #11199, #34041 ),
 ( #65017, #89818 ),
 ( #80714, #56893 ),
 ( #95933, #33535 ),
 ( #50768, #66515 ),
 ( #49283, #72111 ),
 ( #96935, #3107 ),
 ( #50269, #18804 ),
 ( #19795, #35545 ),
 ( #2601, #64521 ),
 ( #11685, #95433 ),
 ( #42172, #97432 ),
 ( #81711, #57895 ),
 ( #26431, #80210 ),
 ( #88833, #10703 ),
 ( #57400, #73109 ),
 ( #27919, #4092 ),
 ( #12183, #58388 ),
 ( #88328, #25920 ),
 ( #34542, #42668 ),
 ( #43160, #87826 ),
 ( #18313, #49780 ),
 ( #65516, #96435 ),
 ( #26927, #48776 ),
 ( #19301, #73602 ),
 ( #35044, #41665 ),
 ( #74102, #58879 ),
 ( #66016, #4597 ),
 ( #27429, #83189 ),
 ( #21781, #90817 ),
 ( #91807, #7075 ),
 ( #43650, #5077 ),
 ( #83696, #36029 ),
 ( #13676, #38025 ),
 ( #22280, #29408 ),
 ( #91312, #37529 ),
 ( #44646, #74587 ),
 ( #75575, #45153 ),
 ( #45645, #30411 ),
 ( #67002, #97915 ),
 ( #68482, #82698 ),
 ( #29910, #52758 ),
 ( #60877, #67490 ),
 ( #76571, #68974 ),
 ( #98412, #37029 ),
 ( #98916, #99416 ),
 ( #84191, #99900 ),
 ( #76078, #51263 ),
 ( #61380, #67991 ),
 ( #60390, #90317 ),
 ( #6576, #28916 ),
 ( #28407, #53264 ),
 ( #14176, #59374 ),
 ( #14682, #59884 ),
 ( #5577, #20288 ),
 ( #20789, #13177 ),
 ( #44148, #82202 ),
 ( #51764, #12686 ),
 ( #75079, #36523 ),
 ( #21289, #52262 ),
 ( #6074, #41921 ),
 ( #48529, #56141 ),
 ( #100398, #72862 ),
 ( #10954, #69974 ),
 ( #9947, #18558 ),
 ( #10445, #49531 ),
 ( #80462, #46147 ),
 ( #22777, #79455 ),
 ( #40900, #46653 ),
 ( #61878, #30911 ),
 ( #3363, #34297 ),
 ( #92307, #25673 ),
 ( #77572, #95689 ),
 ( #53765, #8076 ),
 ( #39023, #26174 ),
 ( #84694, #459 ),
 ( #2350, #25165 ),
 ( #54268, #15183 ),
 ( #77072, #33790 ),
 ( #64267, #7577 ),
 ( #71861, #56645 ),
 ( #64774, #38525 ),
 ( #69480, #15687 ),
 ( #87071, #31415 ),
 ( #92803, #23284 ),
 ( #63765, #85196 ),
 ( #33279, #41406 ),
 ( #57148, #94680 ),
 ( #17562, #95189 ),
 ( #72362, #87576 ),
 ( #18060, #49028 ),
 ( #88085, #79958 ),
 ( #2858, #50030 ),
 ( #28177, #80965 ),
 ( #58631, #52015 ),
 ( #96195, #19555 ),
 ( #35792, #82453 ),
 ( #27182, #82944 ),
 ( #42913, #27681 ),
 ( #13434, #20545 ),
 ( #36292, #74835 ),
 ( #89078, #75333 ),
 ( #11448, #42427 ),
 ( #12935, #58142 ),
 ( #5331, #66762 ),
 ( #50514, #73359 ),
 ( #21045, #44408 ),
 ( #11946, #81960 ),
 ( #67249, #98169 ),
 ( #5830, #97187 ),
 ( #28673, #59634 ),
 ( #65272, #12442 ),
 ( #43412, #34794 ),
 ( #51519, #89576 ),
 ( #26682, #90566 ),
 ( #3853, #74348 ),
 ( #4839, #57641 ),
 ( #88583, #73850 ),
 ( #65764, #81472 ),
 ( #4349, #96680 ),
 ( #20059, #19056 ),
 ( #35300, #66264 ),
 ( #51021, #97681 ),
 ( #59136, #90074 ),
 ( #43902, #23528 ),
 ( #83444, #67750 ),
 ( #38768, #99653 ),
 ( #36787, #53020 ),
 ( #13934, #60638 ),
 ( #77812, #6822 ),
 ( #84944, #30665 ),
 ( #44908, #98668 ),
 ( #29165, #92554 ),
 ( #91559, #69734 ),
 ( #37779, #38269 ),
 ( #75832, #93048 ),
 ( #60140, #45405 ),
 ( #100142, #68735 ),
 ( #22530, #212 ),
 ( #61634, #22035 ),
 ( #91064, #76816 ),
 ( #54506, #85440 ),
 ( #30158, #76322 ),
 ( #62126, #92059 ),
 ( #15927, #77321 ),
 ( #6330, #45899 ),
 ( #99165, #61132 ),
 ( #21537, #46894 ),
 ( #53523, #84446 ),
 ( #23026, #83950 ),
 ( #37285, #31157 ),
 ( #14926, #7315 ),
 ( #54014, #15428 ),
 ( #52514, #69227 ),
 ( #46389, #7822 ),
 ( #68236, #29664 ),
 ( #14431, #26047 ),
 ( #78817, #1222 ),
 ( #40278, #39269 ),
 ( #95563, #79330 ),
 ( #9824, #32658 ),
 ( #2729, #63636 ),
 ( #64143, #33667 ),
 ( #86448, #24040 ),
 ( #70229, #56520 ),
 ( #17941, #40775 ),
 ( #48902, #55513 ),
 ( #56017, #71736 ),
 ( #709, #31655 ),
 ( #8828, #86946 ),
 ( #64648, #72235 ),
 ( #62626, #95065 ),
 ( #94555, #57019 ),
 ( #63130, #17435 ),
 ( #47397, #25551 ),
 ( #71233, #87957 ),
 ( #85951, #93545 ),
 ( #2229, #48396 ),
 ( #33158, #18437 ),
 ( #41280, #78322 ),
 ( #49408, #32156 ),
 ( #79829, #55013 ),
 ( #10325, #8324 ),
 ( #87449, #16423 ),
 ( #39765, #70727 ),
 ( #94056, #24542 ),
 ( #9313, #16933 ),
 ( #47898, #1721 ),
 ( #25042, #11821 ),
 ( #74225, #42791 ),
 ( #4218, #57521 ),
 ( #89451, #43288 ),
 ( #90443, #19928 ),
 ( #96556, #12807 ),
 ( #20414, #67129 ),
 ( #50896, #73722 ),
 ( #42306, #41796 ),
 ( #72739, #51392 ),
 ( #81836, #3239 ),
 ( #35173, #12308 ),
 ( #82330, #34172 ),
 ( #10829, #3728 ),
 ( #66141, #65640 ),
 ( #27056, #20920 ),
 ( #34670, #58020 ),
 ( #88957, #65143 ),
 ( #43780, #26560 ),
 ( #80844, #96067 ),
 ( #28055, #19433 ),
 ( #4718, #50398 ),
 ( #74708, #98042 ),
 ( #88457, #18931 ),
 ( #35669, #49909 ),
 ( #97059, #28537 ),
 ( #5207, #66641 ),
 ( #97554, #59012 ),
 ( #27561, #11329 ),
 ( #58514, #89945 ),
 ( #36165, #80336 ),
 ( #73235, #81339 ),
 ( #59504, #76204 ),
 ( #91428, #6699 ),
 ( #37155, #60013 ),
 ( #7703, #69612 ),
 ( #99036, #68609 ),
 ( #30030, #69097 ),
 ( #14802, #94 ),
 ( #44283, #84821 ),
 ( #61004, #100026 ),
 ( #15305, #38649 ),
 ( #7193, #82822 ),
 ( #31035, #99532 ),
 ( #91938, #21411 ),
 ( #38144, #83826 ),
 ( #62000, #37653 ),
 ( #67622, #68116 ),
 ( #60515, #51895 ),
 ( #13304, #29533 ),
 ( #90939, #92432 ),
 ( #44778, #61505 ),
 ( #36656, #75211 ),
 ( #5703, #84320 ),
 ( #22899, #98540 ),
 ( #53888, #22408 ),
 ( #53392, #29036 ),
 ( #52388, #83322 ),
 ( #46267, #14305 ),
 ( #13803, #92929 ),
 ( #45768, #45277 ),
 ( #30537, #21908 ),
 ( #75703, #77196 ),
 ( #52887, #76693 ),
 ( #6202, #54389 ),
 ( #78201, #55902 ),
 ( #31536, #47780 ),
 ( #55394, #46774 ),
 ( #2115, #86827 ),
 ( #40668, #16816 ),
 ( #9200, #25432 ),
 ( #17317, #8715 ),
 ( #85318, #63517 ),
 ( #17826, #78694 ),
 ( #79211, #48793 ),
 ( #1099, #39149 ),
 ( #48283, #47276 ),
 ( #33053, #24925 ),
 ( #64030, #70607 ),
 ( #32043, #39651 ),
 ( #85831, #79715 ),
 ( #23923, #32545 ),
 ( #64535, #16314 ),
 ( #93429, #15810 ),
 ( #63014, #94439 ),
 ( #10212, #40161 ),
 ( #41169, #94945 ),
 ( #77696, #93937 ),
 ( #86331, #24427 ),
 ( #71116, #23403 ),
 ( #1606, #9711 ),
 ( #71619, #56409 ),
 ( #87328, #72125 ),
 ( #8211, #54893 ),
 ( #2613, #33549 ),
 ( #70107, #590 ),
 ( #62500, #66530 ),
 ( #51274, #57906 ),
 ( #3611, #12697 ),
 ( #65529, #88341 ),
 ( #97445, #4106 ),
 ( #80728, #26446 ),
 ( #35055, #57411 ),
 ( #82215, #73123 ),
 ( #34555, #43665 ),
 ( #27934, #74600 ),
 ( #27445, #18815 ),
 ( #4612, #96947 ),
 ( #35558, #42186 ),
 ( #42680, #58401 ),
 ( #56907, #87841 ),
 ( #95945, #73614 ),
 ( #5092, #58891 ),
 ( #49295, #50783 ),
 ( #36043, #34056 ),
 ( #49795, #25934 ),
 ( #26938, #89834 ),
 ( #95446, #20302 ),
 ( #89339, #10717 ),
 ( #18325, #96446 ),
 ( #11212, #80222 ),
 ( #41679, #3119 ),
 ( #88848, #19313 ),
 ( #66030, #72623 ),
 ( #65032, #50283 ),
 ( #81224, #81724 ),
 ( #11700, #19807 ),
 ( #12196, #43173 ),
 ( #74114, #97927 ),
 ( #21303, #99430 ),
 ( #75094, #91324 ),
 ( #13189, #22791 ),
 ( #28421, #75586 ),
 ( #29925, #37042 ),
 ( #60892, #98933 ),
 ( #52274, #53779 ),
 ( #84205, #37544 ),
 ( #84706, #15197 ),
 ( #29421, #6089 ),
 ( #22294, #38039 ),
 ( #61395, #91819 ),
 ( #21797, #76584 ),
 ( #45659, #7088 ),
 ( #68494, #14190 ),
 ( #46160, #59387 ),
 ( #99912, #67505 ),
 ( #14695, #77088 ),
 ( #30424, #68990 ),
 ( #68003, #7588 ),
 ( #92320, #98425 ),
 ( #28928, #60403 ),
 ( #53276, #52773 ),
 ( #83709, #44162 ),
 ( #76091, #67016 ),
 ( #90329, #6589 ),
 ( #83205, #20804 ),
 ( #51778, #82712 ),
 ( #5592, #45168 ),
 ( #59898, #36537 ),
 ( #90829, #13691 ),
 ( #44662, #100412 ),
 ( #39543, #55282 ),
 ( #55785, #70496 ),
 ( #78581, #86709 ),
 ( #61893, #24313 ),
 ( #63402, #71001 ),
 ( #981, #1492 ),
 ( #47163, #31428 ),
 ( #31933, #86215 ),
 ( #69496, #30923 ),
 ( #77585, #62902 ),
 ( #17199, #48165 ),
 ( #92817, #9089 ),
 ( #93825, #79091 ),
 ( #474, #16696 ),
 ( #15699, #40042 ),
 ( #9593, #40552 ),
 ( #85210, #23297 ),
 ( #47665, #32430 ),
 ( #94319, #71504 ),
 ( #62386, #8090 ),
 ( #38537, #78083 ),
 ( #54283, #93316 ),
 ( #46664, #39038 ),
 ( #24805, #69987 ),
 ( #23807, #54780 ),
 ( #85717, #16195 ),
 ( #8594, #75414 ),
 ( #52596, #30748 ),
 ( #14015, #28760 ),
 ( #69816, #5916 ),
 ( #44995, #59722 ),
 ( #6912, #76906 ),
 ( #92640, #36871 ),
 ( #29249, #90651 ),
 ( #7403, #83533 ),
 ( #23119, #67836 ),
 ( #15514, #60721 ),
 ( #13519, #38360 ),
 ( #44489, #45988 ),
 ( #46478, #14519 ),
 ( #37868, #22617 ),
 ( #60224, #21132 ),
 ( #91148, #76411 ),
 ( #77407, #52102 ),
 ( #61720, #21624 ),
 ( #69314, #85028 ),
 ( #54108, #100234 ),
 ( #29754, #38859 ),
 ( #75915, #68819 ),
 ( #98756, #84534 ),
 ( #7912, #83029 ),
 ( #6421, #61224 ),
 ( #37376, #68321 ),
 ( #99256, #91643 ),
 ( #22124, #53107 ),
 ( #84036, #45495 ),
 ( #99738, #30243 ),
 ( #92142, #53609 ),
 ( #15018, #40865 ),
 ( #71325, #93137 ),
 ( #55606, #32748 ),
 ( #71826, #62217 ),
 ( #9407, #39861 ),
 ( #1311, #47986 ),
 ( #10412, #16015 ),
 ( #32247, #8413 ),
 ( #78914, #48493 ),
 ( #64228, #46983 ),
 ( #801, #23620 ),
 ( #79418, #24131 ),
 ( #1811, #70821 ),
 ( #2319, #87543 ),
 ( #54596, #85530 ),
 ( #63731, #77906 ),
 ( #94141, #18025 ),
 ( #33248, #40370 ),
 ( #31752, #39365 ),
 ( #62721, #48992 ),
 ( #78415, #63218 ),
 ( #79920, #56107 ),
 ( #41373, #95155 ),
 ( #55100, #24627 ),
 ( #86535, #17023 ),
 ( #86036, #70320 ),
 ( #93637, #87036 ),
 ( #16513, #47482 ),
 ( #8912, #94649 ),
 ( #25639, #31246 ),
 ( #25127, #17527 ),
 ( #9912, #56613 ),
 ( #302, #62143 ),
 ( #54524, #23549 ),
 ( #76341, #99183 ),
 ( #37799, #36805 ),
 ( #93066, #76832 ),
 ( #7332, #30173 ),
 ( #85458, #83968 ),
 ( #45423, #15944 ),
 ( #77339, #46909 ),
 ( #38286, #29684 ),
 ( #5849, #6841 ),
 ( #68751, #91574 ),
 ( #67769, #98688 ),
 ( #29184, #60158 ),
 ( #6349, #84464 ),
 ( #91081, #69749 ),
 ( #7840, #15446 ),
 ( #21556, #44927 ),
 ( #37307, #52528 ),
 ( #99668, #231 ),
 ( #61153, #83462 ),
 ( #13950, #75849 ),
 ( #69244, #45918 ),
 ( #100162, #68254 ),
 ( #22055, #60654 ),
 ( #53037, #14447 ),
 ( #92076, #22546 ),
 ( #53537, #14946 ),
 ( #46407, #30679 ),
 ( #61650, #31173 ),
 ( #92568, #23044 ),
 ( #54034, #84960 ),
 ( #38788, #79849 ),
 ( #63148, #77833 ),
 ( #18456, #55028 ),
 ( #78340, #86963 ),
 ( #70245, #10345 ),
 ( #9841, #25060 ),
 ( #726, #16443 ),
 ( #56037, #25568 ),
 ( #17960, #39289 ),
 ( #8340, #1244 ),
 ( #40299, #94074 ),
 ( #24559, #31677 ),
 ( #32175, #55535 ),
 ( #47915, #17452 ),
 ( #72258, #86465 ),
 ( #48418, #48920 ),
 ( #62646, #71250 ),
 ( #40794, #2747 ),
 ( #1739, #87976 ),
 ( #2246, #33688 ),
 ( #26068, #95580 ),
 ( #78835, #70747 ),
 ( #41299, #79348 ),
 ( #16953, #8843 ),
 ( #32678, #93564 ),
 ( #63654, #33178 ),
 ( #64668, #24059 ),
 ( #71755, #64161 ),
 ( #56539, #39785 ),
 ( #87468, #95083 ),
 ( #57040, #9335 ),
 ( #85967, #47414 ),
 ( #94578, #41814 ),
 ( #49931, #27579 ),
 ( #67151, #81358 ),
 ( #4738, #80356 ),
 ( #36184, #66161 ),
 ( #58529, #18952 ),
 ( #35686, #11837 ),
 ( #98059, #43798 ),
 ( #81856, #65165 ),
 ( #51410, #58040 ),
 ( #34689, #49428 ),
 ( #82348, #88478 ),
 ( #96576, #5228 ),
 ( #12829, #96089 ),
 ( #10850, #66662 ),
 ( #73253, #74727 ),
 ( #19448, #50914 ),
 ( #26579, #74242 ),
 ( #34191, #28560 ),
 ( #12331, #50415 ),
 ( #43304, #42810 ),
 ( #3747, #59524 ),
 ( #72760, #89471 ),
 ( #90462, #3255 ),
 ( #73741, #88979 ),
 ( #97574, #20438 ),
 ( #57541, #28075 ),
 ( #4238, #80862 ),
 ( #35190, #97079 ),
 ( #11347, #42322 ),
 ( #65660, #27075 ),
 ( #19945, #59030 ),
 ( #89965, #38667 ),
 ( #53907, #92446 ),
 ( #21927, #31049 ),
 ( #84840, #21429 ),
 ( #52405, #52909 ),
 ( #14820, #83842 ),
 ( #45296, #98561 ),
 ( #30047, #84334 ),
 ( #62018, #61023 ),
 ( #29554, #6218 ),
 ( #61528, #7718 ),
 ( #30553, #22914 ),
 ( #83341, #82841 ),
 ( #13323, #15320 ),
 ( #91953, #44304 ),
 ( #76219, #53410 ),
 ( #46284, #75230 ),
 ( #51913, #44799 ),
 ( #14320, #37176 ),
 ( #68132, #20940 ),
 ( #6716, #29057 ),
 ( #99054, #5724 ),
 ( #77214, #36676 ),
 ( #69632, #45788 ),
 ( #13823, #76709 ),
 ( #67640, #75717 ),
 ( #60532, #60031 ),
 ( #91445, #110 ),
 ( #37669, #68628 ),
 ( #90959, #7210 ),
 ( #38160, #99547 ),
 ( #22425, #69115 ),
 ( #100042, #71633 ),
 ( #39667, #63534 ),
 ( #55919, #41184 ),
 ( #85338, #25449 ),
 ( #71132, #9728 ),
 ( #56424, #48806 ),
 ( #48297, #23421 ),
 ( #79730, #9216 ),
 ( #62518, #31554 ),
 ( #24442, #72140 ),
 ( #87343, #10227 ),
 ( #8228, #78220 ),
 ( #1119, #92945 ),
 ( #54404, #8730 ),
 ( #93447, #33069 ),
 ( #85850, #2133 ),
 ( #77716, #15824 ),
 ( #46791, #24941 ),
 ( #70624, #94460 ),
 ( #17844, #47795 ),
 ( #2627, #64046 ),
 ( #608, #1626 ),
 ( #54907, #93954 ),
 ( #39167, #33569 ),
 ( #78710, #55412 ),
 ( #79228, #32057 ),
 ( #86840, #70123 ),
 ( #63032, #32558 ),
 ( #40683, #94961 ),
 ( #23940, #17336 ),
 ( #16330, #47294 ),
 ( #86351, #16834 ),
 ( #40179, #58905 ),
 ( #96960, #80238 ),
 ( #66548, #73136 ),
 ( #43676, #3626 ),
 ( #65046, #26461 ),
 ( #11227, #95963 ),
 ( #49307, #56921 ),
 ( #64547, #27460 ),
 ( #4622, #87854 ),
 ( #97459, #11716 ),
 ( #88863, #18340 ),
 ( #74129, #72640 ),
 ( #34574, #57425 ),
 ( #42694, #10731 ),
 ( #41696, #19330 ),
 ( #3133, #19820 ),
 ( #58419, #89847 ),
 ( #42204, #73629 ),
 ( #20315, #95460 ),
 ( #18830, #89353 ),
 ( #34074, #50301 ),
 ( #88354, #50797 ),
 ( #49811, #12710 ),
 ( #81736, #65543 ),
 ( #12210, #96461 ),
 ( #80743, #51288 ),
 ( #25950, #4120 ),
 ( #82229, #74614 ),
 ( #26950, #57922 ),
 ( #43187, #35570 ),
 ( #27950, #5108 ),
 ( #81237, #35071 ),
 ( #66044, #76600 ),
 ( #6607, #83726 ),
 ( #84726, #97941 ),
 ( #69006, #36552 ),
 ( #13205, #53794 ),
 ( #99932, #7105 ),
 ( #37055, #46175 ),
 ( #30445, #67520 ),
 ( #98442, #68020 ),
 ( #92336, #83225 ),
 ( #45182, #98947 ),
 ( #28944, #28436 ),
 ( #14206, #38053 ),
 ( #75112, #61411 ),
 ( #68511, #22810 ),
 ( #59399, #82727 ),
 ( #59913, #15216 ),
 ( #21317, #36058 ),
 ( #77104, #44179 ),
 ( #52289, #67033 ),
 ( #76105, #84222 ),
 ( #99443, #90347 ),
 ( #90846, #20819 ),
 ( #14710, #13708 ),
 ( #51794, #5608 ),
 ( #44680, #29437 ),
 ( #75600, #6105 ),
 ( #60416, #53292 ),
 ( #91338, #21814 ),
 ( #37558, #29939 ),
 ( #52790, #60910 ),
 ( #91837, #22314 ),
 ( #45677, #70511 ),
 ( #94841, #63422 ),
 ( #1511, #79115 ),
 ( #70006, #62921 ),
 ( #9107, #86730 ),
 ( #54798, #78599 ),
 ( #71021, #56310 ),
 ( #24332, #32954 ),
 ( #48184, #85228 ),
 ( #39561, #40571 ),
 ( #17218, #8614 ),
 ( #46682, #71523 ),
 ( #77604, #8111 ),
 ( #1001, #87229 ),
 ( #2010, #63930 ),
 ( #23316, #93333 ),
 ( #16216, #7605 ),
 ( #38558, #23825 ),
 ( #39056, #55804 ),
 ( #29622, #30941 ),
 ( #15715, #16716 ),
 ( #31949, #85733 ),
 ( #17726, #54300 ),
 ( #93842, #492 ),
 ( #47182, #92833 ),
 ( #25332, #78101 ),
 ( #86234, #9610 ),
 ( #69514, #55302 ),
 ( #40066, #48694 ),
 ( #47684, #61908 ),
 ( #32448, #31443 ),
 ( #62406, #94340 ),
 ( #24827, #66422 ),
 ( #81622, #88743 ),
 ( #50180, #96843 ),
 ( #3509, #33443 ),
 ( #34453, #4004 ),
 ( #4507, #89737 ),
 ( #81119, #73512 ),
 ( #27336, #41574 ),
 ( #89235, #11600 ),
 ( #19704, #26339 ),
 ( #35454, #97345 ),
 ( #57312, #96346 ),
 ( #50677, #12096 ),
 ( #27831, #11108 ),
 ( #43066, #74012 ),
 ( #20205, #18226 ),
 ( #57799, #49195 ),
 ( #34947, #42078 ),
 ( #58786, #79617 ),
 ( #42577, #95348 ),
 ( #19212, #10109 ),
 ( #41068, #88243 ),
 ( #80120, #72522 ),
 ( #18710, #10609 ),
 ( #73023, #72025 ),
 ( #2509, #3015 ),
 ( #64432, #95846 ),
 ( #25833, #56808 ),
 ( #87740, #65429 ),
 ( #26834, #33951 ),
 ( #64930, #65923 ),
 ( #49689, #80620 ),
 ( #58297, #83605 ),
 ( #36439, #53180 ),
 ( #51173, #67405 ),
 ( #98326, #84111 ),
 ( #91715, #37938 ),
 ( #60795, #22195 ),
 ( #43564, #14595 ),
 ( #14091, #98830 ),
 ( #21697, #74500 ),
 ( #5989, #45068 ),
 ( #45567, #12602 ),
 ( #60297, #90731 ),
 ( #52171, #29325 ),
 ( #61295, #66912 ),
 ( #83101, #59284 ),
 ( #29824, #92221 ),
 ( #75988, #76484 ),
 ( #51678, #4994 ),
 ( #13592, #5490 ),
 ( #6990, #90231 ),
 ( #82118, #97833 ),
 ( #68887, #35943 ),
 ( #99812, #6495 ),
 ( #44057, #37446 ),
 ( #28328, #28833 ),
 ( #82611, #20705 ),
 ( #13090, #30319 ),
 ( #59798, #44559 ),
 ( #74990, #21204 ),
 ( #68397, #75486 ),
 ( #36939, #67910 ),
 ( #52670, #91221 ),
 ( #99329, #93718 ),
 ( #86113, #71401 ),
 ( #15099, #55685 ),
 ( #882, #39941 ),
 ( #86614, #78992 ),
 ( #78488, #70393 ),
 ( #84611, #46065 ),
 ( #23200, #31835 ),
 ( #9490, #17100 ),
 ( #76984, #8988 ),
 ( #8494, #40451 ),
 ( #77485, #62804 ),
 ( #61793, #70902 ),
 ( #1887, #32832 ),
 ( #63809, #55185 ),
 ( #7987, #24705 ),
 ( #24211, #22693 ),
 ( #38936, #54185 ),
 ( #53680, #69891 ),
 ( #16590, #54677 ),
 ( #48064, #7481 ),
 ( #47568, #63300 ),
 ( #92712, #38438 ),
 ( #1393, #47066 ),
 ( #69391, #32328 ),
 ( #94219, #62293 ),
 ( #376, #100310 ),
 ( #30828, #85109 ),
 ( #31324, #15593 ),
 ( #46557, #93217 ),
 ( #23705, #85608 ),
 ( #16096, #77980 ),
 ( #39444, #18106 ),
 ( #96237, #64817 ),
 ( #5737, #40945 ),
 ( #51926, #79501 ),
 ( #9989, #11487 ),
 ( #82855, #80502 ),
 ( #3402, #88624 ),
 ( #25713, #56187 ),
 ( #56692, #13340 ),
 ( #72406, #57193 ),
 ( #44318, #50067 ),
 ( #75246, #90478 ),
 ( #49071, #18595 ),
 ( #33829, #49570 ),
 ( #41448, #65315 ),
 ( #88127, #71905 ),
 ( #10994, #36691 ),
 ( #96723, #34338 ),
 ( #80000, #87623 ),
 ( #26720, #10487 ),
 ( #94723, #2900 ),
 ( #95731, #25209 ),
 ( #65805, #87112 ),
 ( #57681, #26220 ),
 ( #3897, #19095 ),
 ( #34836, #41961 ),
 ( #72905, #81007 ),
 ( #17605, #48577 ),
 ( #95230, #42464 ),
 ( #2390, #73402 ),
 ( #27224, #59540 ),
 ( #33320, #64309 ),
 ( #20953, #98577 ),
 ( #99560, #62031 ),
 ( #85349, #92957 ),
 ( #100053, #83354 ),
 ( #69642, #76233 ),
 ( #52924, #67658 ),
 ( #120, #6233 ),
 ( #54414, #60547 ),
 ( #38677, #52423 ),
 ( #31059, #29072 ),
 ( #14834, #7731 ),
 ( #60046, #23431 ),
 ( #91968, #90974 ),
 ( #77223, #75732 ),
 ( #6730, #29569 ),
 ( #45800, #21442 ),
 ( #13839, #22438 ),
 ( #15834, #46805 ),
 ( #77724, #61539 ),
 ( #14333, #45311 ),
 ( #8239, #44813 ),
 ( #30063, #21938 ),
 ( #37683, #69131 ),
 ( #37189, #61036 ),
 ( #30568, #46295 ),
 ( #68643, #38170 ),
 ( #92457, #68145 ),
 ( #99070, #91462 ),
 ( #76722, #84853 ),
 ( #83856, #53421 ),
 ( #22931, #84351 ),
 ( #7223, #53920 ),
 ( #15333, #70634 ),
 ( #33579, #33079 ),
 ( #87868, #63551 ),
 ( #23951, #48310 ),
 ( #79239, #49320 ),
 ( #18353, #47804 ),
 ( #78229, #79745 ),
 ( #32068, #48819 ),
 ( #54918, #31567 ),
 ( #39178, #71645 ),
 ( #55423, #9738 ),
 ( #64557, #94471 ),
 ( #25962, #10236 ),
 ( #85863, #70132 ),
 ( #41199, #1636 ),
 ( #621, #86362 ),
 ( #16339, #63043 ),
 ( #93963, #2146 ),
 ( #80253, #95476 ),
 ( #2640, #47306 ),
 ( #94969, #87358 ),
 ( #72152, #40693 ),
 ( #64058, #56934 ),
 ( #71145, #8740 ),
 ( #78723, #32570 ),
 ( #56435, #24955 ),
 ( #55929, #62528 ),
 ( #25458, #24457 ),
 ( #93458, #17855 ),
 ( #39679, #1130 ),
 ( #16846, #9227 ),
 ( #40190, #86850 ),
 ( #17348, #58919 ),
 ( #59415, #3146 ),
 ( #26961, #81751 ),
 ( #36076, #66054 ),
 ( #97954, #51303 ),
 ( #57439, #41709 ),
 ( #12722, #73642 ),
 ( #10744, #57936 ),
 ( #96974, #42708 ),
 ( #74629, #28451 ),
 ( #4634, #5124 ),
 ( #88875, #89364 ),
 ( #67046, #72650 ),
 ( #65558, #43200 ),
 ( #18845, #35083 ),
 ( #4134, #26475 ),
 ( #19346, #27474 ),
 ( #27964, #58431 ),
 ( #19832, #34087 ),
 ( #90360, #12223 ),
 ( #74141, #50810 ),
 ( #20833, #35587 ),
 ( #66561, #51810 ),
 ( #65060, #97473 ),
 ( #82243, #89862 ),
 ( #20332, #43691 ),
 ( #95976, #88367 ),
 ( #49826, #80759 ),
 ( #11240, #42216 ),
 ( #73150, #3640 ),
 ( #34586, #96473 ),
 ( #50312, #81248 ),
 ( #11730, #69530 ),
 ( #37072, #60924 ),
 ( #21330, #38066 ),
 ( #61922, #13 ),
 ( #38573, #14725 ),
 ( #68036, #84742 ),
 ( #22327, #92851 ),
 ( #98961, #83241 ),
 ( #30955, #29450 ),
 ( #91853, #14219 ),
 ( #15230, #82740 ),
 ( #28957, #13223 ),
 ( #46188, #45195 ),
 ( #44195, #60430 ),
 ( #59930, #6120 ),
 ( #75614, #45691 ),
 ( #76614, #77117 ),
 ( #91354, #53305 ),
 ( #7624, #75130 ),
 ( #21829, #7118 ),
 ( #90858, #6621 ),
 ( #52306, #69023 ),
 ( #67536, #23329 ),
 ( #99947, #52806 ),
 ( #68526, #5622 ),
 ( #30460, #83739 ),
 ( #84238, #37575 ),
 ( #36566, #99456 ),
 ( #61425, #98457 ),
 ( #13724, #92351 ),
 ( #53810, #22823 ),
 ( #29957, #44695 ),
 ( #76123, #94857 ),
 ( #24844, #1524 ),
 ( #2528, #15729 ),
 ( #87247, #54811 ),
 ( #31460, #72042 ),
 ( #8131, #9625 ),
 ( #40080, #41088 ),
 ( #8628, #32463 ),
 ( #93347, #40587 ),
 ( #33458, #64448 ),
 ( #10124, #86746 ),
 ( #39575, #56325 ),
 ( #54314, #70528 ),
 ( #1016, #17741 ),
 ( #95363, #31962 ),
 ( #63438, #86250 ),
 ( #16233, #46698 ),
 ( #77618, #25347 ),
 ( #55818, #39069 ),
 ( #2032, #78615 ),
 ( #70021, #17234 ),
 ( #48710, #507 ),
 ( #79631, #94358 ),
 ( #9123, #62423 ),
 ( #23839, #85240 ),
 ( #85749, #16729 ),
 ( #47197, #62935 ),
 ( #78116, #93855 ),
 ( #24349, #48201 ),
 ( #55316, #47696 ),
 ( #71034, #79131 ),
 ( #71537, #32971 ),
 ( #63948, #27849 ),
 ( #33965, #50198 ),
 ( #57823, #41592 ),
 ( #34472, #88763 ),
 ( #43089, #19234 ),
 ( #11619, #58806 ),
 ( #19722, #11126 ),
 ( #87756, #65943 ),
 ( #43582, #12623 ),
 ( #81140, #65446 ),
 ( #81644, #97368 ),
 ( #20227, #58317 ),
 ( #42598, #35475 ),
 ( #4526, #66443 ),
 ( #5014, #82138 ),
 ( #3528, #73042 ),
 ( #51196, #89755 ),
 ( #3030, #74523 ),
 ( #35963, #66933 ),
 ( #26854, #25849 ),
 ( #56825, #26354 ),
 ( #57328, #73532 ),
 ( #18241, #49210 ),
 ( #80139, #89255 ),
 ( #42095, #10630 ),
 ( #72536, #96365 ),
 ( #4023, #64948 ),
 ( #95861, #88258 ),
 ( #34969, #96865 ),
 ( #18732, #49710 ),
 ( #80642, #27356 ),
 ( #50696, #12115 ),
 ( #74033, #77003 ),
 ( #92239, #53703 ),
 ( #13114, #83122 ),
 ( #6009, #97851 ),
 ( #28345, #13612 ),
 ( #36457, #37958 ),
 ( #90749, #7011 ),
 ( #82629, #90252 ),
 ( #59309, #29847 ),
 ( #68910, #20726 ),
 ( #45087, #45587 ),
 ( #51696, #44078 ),
 ( #5508, #6515 ),
 ( #59816, #98849 ),
 ( #75011, #7507 ),
 ( #52690, #29345 ),
 ( #61315, #15120 ),
 ( #91738, #22712 ),
 ( #75508, #76011 ),
 ( #84629, #67425 ),
 ( #99835, #99349 ),
 ( #60814, #30342 ),
 ( #60315, #98349 ),
 ( #46084, #38459 ),
 ( #67930, #21223 ),
 ( #91245, #28853 ),
 ( #52194, #68415 ),
 ( #22217, #21716 ),
 ( #44580, #83629 ),
 ( #53199, #36962 ),
 ( #14112, #37467 ),
 ( #84129, #14618 ),
 ( #76503, #8513 ),
 ( #31855, #54697 ),
 ( #48597, #25229 ),
 ( #47086, #16115 ),
 ( #94743, #9510 ),
 ( #56207, #32853 ),
 ( #23220, #24725 ),
 ( #55204, #79013 ),
 ( #62824, #85632 ),
 ( #79520, #87135 ),
 ( #78002, #39465 ),
 ( #17625, #40470 ),
 ( #46581, #10010 ),
 ( #1912, #71420 ),
 ( #70417, #69413 ),
 ( #63831, #69911 ),
 ( #395, #900 ),
 ( #63323, #93738 ),
 ( #77505, #54204 ),
 ( #32346, #9010 ),
 ( #39961, #100330 ),
 ( #24233, #31348 ),
 ( #30846, #86135 ),
 ( #78506, #16610 ),
 ( #62312, #61813 ),
 ( #92734, #85128 ),
 ( #70923, #15614 ),
 ( #47588, #1412 ),
 ( #8007, #38955 ),
 ( #94241, #55707 ),
 ( #86634, #17118 ),
 ( #93237, #23726 ),
 ( #48088, #33851 ),
 ( #19614, #82021 ),
 ( #73420, #4408 ),
 ( #41467, #2412 ),
 ( #89141, #64839 ),
 ( #42487, #11014 ),
 ( #51081, #87642 ),
 ( #97247, #25740 ),
 ( #58688, #3917 ),
 ( #95748, #34854 ),
 ( #71928, #26240 ),
 ( #11505, #58199 ),
 ( #65334, #95249 ),
 ( #96255, #65822 ),
 ( #27738, #96747 ),
 ( #89635, #35360 ),
 ( #2919, #26739 ),
 ( #81533, #33340 ),
 ( #42975, #88645 ),
 ( #57701, #64332 ),
 ( #50577, #49091 ),
 ( #80522, #57213 ),
 ( #19115, #56710 ),
 ( #18126, #50088 ),
 ( #20119, #66321 ),
 ( #40968, #27243 ),
 ( #80023, #10507 ),
 ( #72426, #88146 ),
 ( #18616, #12007 ),
 ( #49589, #81028 ),
 ( #41982, #73910 ),
 ( #72923, #3423 ),
 ( #34357, #83003 ),
 ( #44967, #44466 ),
 ( #67305, #99712 ),
 ( #29727, #83506 ),
 ( #30216, #61199 ),
 ( #75391, #52076 ),
 ( #68294, #84007 ),
 ( #6887, #75892 ),
 ( #36850, #92118 ),
 ( #91617, #53080 ),
 ( #13990, #60196 ),
 ( #22589, #74409 ),
 ( #45469, #12995 ),
 ( #60695, #68795 ),
 ( #76385, #14494 ),
 ( #13494, #53584 ),
 ( #37839, #43958 ),
 ( #74893, #5888 ),
 ( #6396, #67813 ),
 ( #98735, #90134 ),
 ( #21598, #37353 ),
 ( #12505, #52572 ),
 ( #21105, #98228 ),
 ( #43470, #4901 ),
 ( #99225, #29228 ),
 ( #5394, #35847 ),
 ( #66821, #28736 ),
 ( #82513, #51578 ),
 ( #91125, #97741 ),
 ( #28233, #59195 ),
 ( #20611, #59696 ),
 ( #22096, #36348 ),
 ( #90629, #270 ),
 ( #23092, #24599 ),
 ( #85003, #93606 ),
 ( #25100, #46451 ),
 ( #16483, #31726 ),
 ( #76874, #54081 ),
 ( #62691, #32214 ),
 ( #7378, #38332 ),
 ( #92611, #24102 ),
 ( #77381, #85503 ),
 ( #69289, #94619 ),
 ( #39330, #15984 ),
 ( #47455, #63191 ),
 ( #40339, #78381 ),
 ( #30725, #15487 ),
 ( #39832, #94114 ),
 ( #86506, #86008 ),
 ( #8887, #55576 ),
 ( #70792, #71293 ),
 ( #32718, #1780 ),
 ( #54563, #7881 ),
 ( #46956, #14994 ),
 ( #69792, #38832 ),
 ( #55073, #31218 ),
 ( #63702, #62188 ),
 ( #23593, #84509 ),
 ( #16990, #45962 ),
 ( #1285, #93113 ),
 ( #100205, #77878 ),
 ( #8383, #70292 ),
 ( #61692, #773 ),
 ( #47958, #78879 ),
 ( #9380, #96614 ),
 ( #73781, #88017 ),
 ( #27113, #65700 ),
 ( #66201, #95123 ),
 ( #41342, #87516 ),
 ( #96130, #17999 ),
 ( #42852, #33728 ),
 ( #95626, #4280 ),
 ( #58082, #35230 ),
 ( #88516, #79890 ),
 ( #89015, #57580 ),
 ( #19491, #2789 ),
 ( #3301, #18992 ),
 ( #64709, #72795 ),
 ( #50452, #81401 ),
 ( #97121, #18495 ),
 ( #11881, #56074 ),
 ( #87006, #25613 ),
 ( #56581, #17497 ),
 ( #49468, #48462 ),
 ( #79392, #9881 ),
 ( #49970, #71797 ),
 ( #40832, #26112 ),
 ( #72295, #2290 ),
 ( #33220, #48959 ),
 ( #64201, #10383 ),
 ( #57082, #80399 ),
 ( #10889, #41856 ),
 ( #34233, #65207 ),
 ( #26617, #80898 ),
 ( #11385, #42363 ),
 ( #73294, #3789 ),
 ( #34726, #90010 ),
 ( #75270, #19992 ),
 ( #43345, #82880 ),
 ( #14364, #91489 ),
 ( #21968, #21470 ),
 ( #74769, #5266 ),
 ( #99096, #52951 ),
 ( #90502, #82388 ),
 ( #35730, #51952 ),
 ( #74284, #52448 ),
 ( #12372, #76262 ),
 ( #90997, #98103 ),
 ( #60072, #59570 ),
 ( #12867, #28113 ),
 ( #20978, #68669 ),
 ( #89507, #97613 ),
 ( #68170, #43838 ),
 ( #50959, #83881 ),
 ( #13367, #81898 ),
 ( #37219, #66701 ),
 ( #67187, #20483 ),
 ( #5764, #4775 ),
 ( #59073, #51452 ),
 ( #36224, #83379 ),
 ( #27619, #45338 ),
 ( #6755, #28608 ),
 ( #44343, #13868 ),
 ( #36721, #29595 ),
 ( #67685, #98606 ),
 ( #29096, #44839 ),
 ( #75763, #37710 ),
 ( #6261, #60572 ),
 ( #58567, #31091 ),
 ( #53952, #87773 ),
 ( #17758, #70163 ),
 ( #53454, #95379 ),
 ( #62061, #38705 ),
 ( #54948, #72060 ),
 ( #2542, #48727 ),
 ( #54443, #10143 ),
 ( #79645, #41105 ),
 ( #646, #46833 ),
 ( #49229, #61065 ),
 ( #33475, #100080 ),
 ( #64467, #56841 ),
 ( #18255, #84383 ),
 ( #30093, #85377 ),
 ( #15864, #84880 ),
 ( #30595, #92986 ),
 ( #80157, #10646 ),
 ( #41609, #31594 ),
 ( #15361, #25868 ),
 ( #99588, #46326 ),
 ( #77256, #91993 ),
 ( #22464, #14863 ),
 ( #45831, #76749 ),
 ( #7250, #22959 ),
 ( #23461, #7759 ),
 ( #38204, #69160 ),
 ( #77749, #61567 ),
 ( #92491, #69669 ),
 ( #148, #8265 ),
 ( #39203, #62560 ),
 ( #93484, #23976 ),
 ( #87262, #42610 ),
 ( #43597, #59320 ),
 ( #88276, #11632 ),
 ( #34981, #57343 ),
 ( #65461, #4543 ),
 ( #3046, #26869 ),
 ( #43101, #89768 ),
 ( #96879, #26370 ),
 ( #27370, #97379 ),
 ( #97863, #82645 ),
 ( #74045, #66461 ),
 ( #20240, #34484 ),
 ( #82150, #35488 ),
 ( #57836, #80656 ),
 ( #27863, #20739 ),
 ( #64965, #5027 ),
 ( #50708, #51208 ),
 ( #35975, #28359 ),
 ( #58820, #33983 ),
 ( #90264, #89267 ),
 ( #81658, #42114 ),
 ( #12635, #4039 ),
 ( #51707, #66945 ),
 ( #74537, #18745 ),
 ( #12129, #13125 ),
 ( #72552, #81155 ),
 ( #11141, #95876 ),
 ( #96378, #49724 ),
 ( #73057, #3542 ),
 ( #88778, #19245 ),
 ( #50213, #73546 ),
 ( #65959, #19736 ),
 ( #58331, #61827 ),
 ( #100345, #76517 ),
 ( #7023, #84140 ),
 ( #14630, #23233 ),
 ( #29357, #44594 ),
 ( #30861, #91257 ),
 ( #53213, #76023 ),
 ( #6021, #5520 ),
 ( #91750, #84644 ),
 ( #83135, #46096 ),
 ( #92255, #68428 ),
 ( #67436, #53716 ),
 ( #67940, #77023 ),
 ( #60334, #44093 ),
 ( #85145, #21237 ),
 ( #21731, #36976 ),
 ( #22726, #75021 ),
 ( #37974, #7522 ),
 ( #75522, #36473 ),
 ( #15133, #98864 ),
 ( #45597, #14125 ),
 ( #38477, #92749 ),
 ( #83643, #52705 ),
 ( #28866, #61330 ),
 ( #54219, #29858 ),
 ( #68925, #99851 ),
 ( #45102, #98362 ),
 ( #6527, #59828 ),
 ( #37478, #99364 ),
 ( #90762, #30357 ),
 ( #52207, #69427 ),
 ( #60831, #22229 ),
 ( #13622, #79031 ),
 ( #70432, #1427 ),
 ( #63340, #56224 ),
 ( #78520, #63846 ),
 ( #9528, #31363 ),
 ( #24249, #1929 ),
 ( #40485, #93758 ),
 ( #93256, #71439 ),
 ( #46599, #85652 ),
 ( #32874, #94258 ),
 ( #17641, #38972 ),
 ( #24742, #94759 ),
 ( #16132, #16631 ),
 ( #32364, #25250 ),
 ( #919, #55723 ),
 ( #86650, #87153 ),
 ( #77523, #48613 ),
 ( #15634, #23743 ),
 ( #47603, #8022 ),
 ( #69925, #9028 ),
 ( #17138, #62840 ),
 ( #8529, #78017 ),
 ( #39977, #411 ),
 ( #62327, #54718 ),
 ( #31871, #70940 ),
 ( #48105, #47101 ),
 ( #39480, #55222 ),
 ( #86150, #76151 ),
 ( #59961, #37606 ),
 ( #85267, #6151 ),
 ( #36602, #84771 ),
 ( #14753, #67571 ),
 ( #99489, #76644 ),
 ( #15259, #5652 ),
 ( #75162, #68066 ),
 ( #6650, #29480 ),
 ( #60465, #44231 ),
 ( #98990, #91383 ),
 ( #7145, #22853 ),
 ( #40, #38097 ),
 ( #22354, #46215 ),
 ( #98488, #68555 ),
 ( #69051, #38602 ),
 ( #29984, #54342 ),
 ( #90889, #83770 ),
 ( #60955, #28989 ),
 ( #91881, #30985 ),
 ( #77149, #53341 ),
 ( #21860, #75650 ),
 ( #84270, #37102 ),
 ( #45721, #99977 ),
 ( #21364, #52834 ),
 ( #13753, #52338 ),
 ( #14252, #30486 ),
 ( #69561, #61454 ),
 ( #61953, #7653 ),
 ( #83275, #44725 ),
 ( #92879, #92381 ),
 ( #45227, #53840 ),
 ( #23358, #47727 ),
 ( #48230, #94887 ),
 ( #72076, #79161 ),
 ( #62449, #16264 ),
 ( #71570, #63977 ),
 ( #17776, #17267 ),
 ( #9660, #87275 ),
 ( #78643, #31486 ),
 ( #24376, #9149 ),
 ( #33002, #40110 ),
 ( #1555, #48740 ),
 ( #2556, #86776 ),
 ( #55848, #78144 ),
 ( #33493, #93888 ),
 ( #55345, #64480 ),
 ( #79660, #95394 ),
 ( #40615, #39601 ),
 ( #25884, #86277 ),
 ( #71066, #1049 ),
 ( #56856, #15759 ),
 ( #16757, #62960 ),
 ( #47222, #94390 ),
 ( #46724, #10160 ),
 ( #70052, #2063 ),
 ( #32496, #77650 ),
 ( #70553, #24872 ),
 ( #63468, #41119 ),
 ( #25379, #8157 ),
 ( #93377, #538 ),
 ( #56356, #39095 ),
 ( #23864, #54841 ),
 ( #85782, #8659 ),
 ( #31991, #97874 ),
 ( #58836, #66479 ),
 ( #34501, #58348 ),
 ( #50726, #35988 ),
 ( #80171, #20253 ),
 ( #65975, #4557 ),
 ( #51221, #43610 ),
 ( #43114, #18271 ),
 ( #26386, #82164 ),
 ( #57356, #88289 ),
 ( #19258, #66961 ),
 ( #12647, #74553 ),
 ( #3059, #73071 ),
 ( #96392, #87788 ),
 ( #49243, #3555 ),
 ( #18760, #88794 ),
 ( #28372, #95891 ),
 ( #72566, #10662 ),
 ( #41623, #19750 ),
 ( #65474, #89283 ),
 ( #5041, #42624 ),
 ( #34001, #64977 ),
 ( #49741, #96894 ),
 ( #80668, #50229 ),
 ( #11155, #42131 ),
 ( #73562, #81167 ),
 ( #26883, #57854 ),
 ( #81671, #11647 ),
 ( #4052, #27387 ),
 ( #74061, #35503 ),
 ( #89783, #12144 ),
 ( #97393, #34995 ),
 ( #27878, #75038 ),
 ( #67953, #21745 ),
 ( #76529, #52719 ),
 ( #91274, #90279 ),
 ( #46107, #29872 ),
 ( #60843, #83655 ),
 ( #53726, #14137 ),
 ( #98880, #77035 ),
 ( #30370, #7536 ),
 ( #91761, #83153 ),
 ( #38490, #29370 ),
 ( #45116, #22241 ),
 ( #76034, #6542 ),
 ( #21249, #20751 ),
 ( #51720, #99863 ),
 ( #53225, #82660 ),
 ( #37489, #84153 ),
 ( #68938, #67449 ),
 ( #60348, #52223 ),
 ( #68440, #13138 ),
 ( #5533, #99377 ),
 ( #69440, #22742 ),
 ( #84657, #14644 ),
 ( #6036, #36988 ),
 ( #61342, #15144 ),
 ( #45609, #13637 ),
 ( #100357, #98374 ),
 ( #59331, #7035 ),
 ( #37988, #92265 ),
 ( #44109, #36484 ),
 ( #28878, #59840 ),
 ( #44606, #90778 ),
 ( #75533, #1436 ),
 ( #85154, #25257 ),
 ( #55732, #86658 ),
 ( #40997, #15644 ),
 ( #24751, #1939 ),
 ( #55234, #79546 ),
 ( #86160, #93769 ),
 ( #38983, #10037 ),
 ( #48621, #8539 ),
 ( #47612, #56236 ),
 ( #71451, #8032 ),
 ( #62850, #63855 ),
 ( #61840, #16641 ),
 ( #78531, #85662 ),
 ( #421, #69933 ),
 ( #17147, #24259 ),
 ( #9035, #31373 ),
 ( #39988, #94267 ),
 ( #71954, #70948 ),
 ( #39492, #16142 ),
 ( #93263, #32883 ),
 ( #929, #32374 ),
 ( #17651, #63350 ),
 ( #70442, #31879 ),
 ( #46612, #48113 ),
 ( #79041, #94769 ),
 ( #9536, #47114 ),
 ( #40495, #87161 ),
 ( #30874, #92761 ),
 ( #23247, #54229 ),
 ( #77534, #62337 ),
 ( #23750, #54727 ),
 ( #78027, #12033 ),
 ( #81558, #43000 ),
 ( #73447, #50113 ),
 ( #80549, #49619 ),
 ( #27764, #73941 ),
 ( #80049, #20143 ),
 ( #35388, #4439 ),
 ( #88673, #89665 ),
 ( #57238, #81051 ),
 ( #41496, #58229 ),
 ( #82049, #51106 ),
 ( #58714, #34879 ),
 ( #88172, #66351 ),
 ( #42509, #12530 ),
 ( #18641, #2944 ),
 ( #34382, #65856 ),
 ( #96278, #65360 ),
 ( #64862, #64357 ),
 ( #95278, #97276 ),
 ( #3940, #25764 ),
 ( #57731, #96774 ),
 ( #44869, #2435 ),
 ( #11534, #42008 ),
 ( #11043, #33369 ),
 ( #56735, #10535 ),
 ( #72950, #95776 ),
 ( #87668, #18148 ),
 ( #27272, #49122 ),
 ( #33879, #72449 ),
 ( #50605, #26266 ),
 ( #3447, #26766 ),
 ( #89167, #19144 ),
 ( #19640, #21996 ),
 ( #14890, #37739 ),
 ( #75792, #92021 ),
 ( #52977, #99618 ),
 ( #68698, #7784 ),
 ( #16390, #31620 ),
 ( #39232, #83913 ),
 ( #37249, #31117 ),
 ( #30119, #77777 ),
 ( #45858, #77282 ),
 ( #62585, #7279 ),
 ( #60601, #24005 ),
 ( #38729, #76776 ),
 ( #69695, #38231 ),
 ( #61092, #29625 ),
 ( #54973, #84905 ),
 ( #93511, #85914 ),
 ( #69186, #100106 ),
 ( #62091, #46855 ),
 ( #70189, #177 ),
 ( #30619, #6291 ),
 ( #54469, #15892 ),
 ( #46351, #22989 ),
 ( #93011, #22494 ),
 ( #673, #8287 ),
 ( #14391, #68197 ),
 ( #99126, #91522 ),
 ( #61600, #45371 ),
 ( #76288, #6781 ),
 ( #53486, #92516 ),
 ( #84412, #53978 ),
 ( #15389, #23488 ),
 ( #85404, #87411 ),
 ( #17907, #26523 ),
 ( #32624, #47862 ),
 ( #79292, #79794 ),
 ( #40741, #9789 ),
 ( #9279, #8792 ),
 ( #39733, #87921 ),
 ( #3199, #1183 ),
 ( #78285, #33126 ),
 ( #80303, #78783 ),
 ( #40244, #71699 ),
 ( #57487, #65108 ),
 ( #34141, #10291 ),
 ( #63599, #49372 ),
 ( #47356, #94522 ),
 ( #25004, #10795 ),
 ( #48363, #96028 ),
 ( #55475, #18403 ),
 ( #70689, #41759 ),
 ( #32121, #72704 ),
 ( #48867, #63093 ),
 ( #2195, #41247 ),
 ( #26013, #56490 ),
 ( #94021, #71196 ),
 ( #64106, #55986 ),
 ( #88423, #24506 ),
 ( #95027, #86412 ),
 ( #16899, #1688 ),
 ( #86910, #17403 ),
 ( #25516, #72203 ),
 ( #95528, #2691 ),
 ( #33634, #64614 ),
 ( #56983, #5669 ),
 ( #34637, #58481 ),
 ( #81800, #3691 ),
 ( #12275, #36619 ),
 ( #20884, #28020 ),
 ( #42757, #43253 ),
 ( #65606, #81302 ),
 ( #97025, #74193 ),
 ( #67588, #74679 ),
 ( #98505, #13271 ),
 ( #73690, #4686 ),
 ( #89417, #35634 ),
 ( #4186, #27020 ),
 ( #11787, #29002 ),
 ( #66109, #66609 ),
 ( #59468, #90409 ),
 ( #59974, #96524 ),
 ( #57986, #11291 ),
 ( #18895, #51356 ),
 ( #51858, #42272 ),
 ( #44247, #97519 ),
 ( #75175, #98003 ),
 ( #88924, #49876 ),
 ( #82791, #58974 ),
 ( #80808, #35138 ),
 ( #19394, #27524 ),
 ( #19889, #82296 ),
 ( #12774, #73203 ),
 ( #50863, #89913 ),
 ( #50366, #20382 ),
 ( #43744, #5173 ),
 ( #36128, #67098 ),
 ( #28507, #15271 ),
 ( #75664, #39114 ),
 ( #7668, #84283 ),
 ( #76657, #92895 ),
 ( #84785, #14265 ),
 ( #99991, #14767 ),
 ( #85287, #45733 ),
 ( #46231, #15775 ),
 ( #44743, #61471 ),
 ( #61968, #38616 ),
 ( #7161, #58 ),
 ( #69576, #31001 ),
 ( #70067, #46740 ),
 ( #90908, #52353 ),
 ( #23372, #91395 ),
 ( #77664, #54355 ),
 ( #6165, #77164 ),
 ( #38110, #8172 ),
 ( #45241, #69066 ),
 ( #29496, #556 ),
 ( #31502, #21376 ),
 ( #83287, #22868 ),
 ( #76164, #13765 ),
 ( #37117, #6663 ),
 ( #37617, #68077 ),
 ( #22371, #53853 ),
 ( #53355, #29996 ),
 ( #99002, #60479 ),
 ( #21872, #52848 ),
 ( #30499, #83787 ),
 ( #68574, #99500 ),
 ( #60970, #91895 ),
 ( #92394, #23885 ),
 ( #95411, #62980 ),
 ( #79679, #18288 ),
 ( #25898, #33512 ),
 ( #63485, #72585 ),
 ( #56870, #93902 ),
 ( #24391, #94405 ),
 ( #56372, #24888 ),
 ( #86790, #39617 ),
 ( #71585, #25395 ),
 ( #3078, #2078 ),
 ( #78658, #87803 ),
 ( #55868, #10677 ),
 ( #17283, #48246 ),
 ( #55361, #54858 ),
 ( #85798, #2571 ),
 ( #33017, #16278 ),
 ( #79177, #94905 ),
 ( #41137, #63992 ),
 ( #93394, #86292 ),
 ( #9675, #47743 ),
 ( #9167, #62464 ),
 ( #16780, #40126 ),
 ( #80187, #49260 ),
 ( #87292, #41639 ),
 ( #71081, #47239 ),
 ( #10175, #1573 ),
 ( #17790, #32510 ),
 ( #64495, #78163 ),
 ( #8676, #40632 ),
 ( #48753, #70569 ),
 ( #72090, #1065 ),
 ( #32007, #43129 ),
 ( #12161, #82675 ),
 ( #58362, #88305 ),
 ( #89300, #96411 ),
 ( #81688, #26402 ),
 ( #49757, #19768 ),
 ( #26898, #66492 ),
 ( #75052, #90293 ),
 ( #97890, #80684 ),
 ( #95909, #89797 ),
 ( #57870, #36003 ),
 ( #42146, #50742 ),
 ( #11176, #58850 ),
 ( #18775, #13154 ),
 ( #97405, #4067 ),
 ( #27895, #65991 ),
 ( #88808, #73086 ),
 ( #44126, #74079 ),
 ( #3575, #28386 ),
 ( #20266, #51234 ),
 ( #82177, #5055 ),
 ( #66978, #12662 ),
 ( #4572, #43627 ),
 ( #74565, #59345 ),
 ( #34016, #20763 ),
 ( #64992, #57376 ),
 ( #51741, #34517 ),
 ( #65491, #19274 ),
 ( #50246, #81183 ),
 ( #11663, #35521 ),
 ( #42643, #73578 ),
 ( #35014, #96908 ),
 ( #27403, #68460 ),
 ( #61857, #38005 ),
 ( #91291, #7554 ),
 ( #5553, #21760 ),
 ( #52734, #38505 ),
 ( #6556, #54245 ),
 ( #13651, #77052 ),
 ( #98389, #69454 ),
 ( #68955, #53241 ),
 ( #76545, #28892 ),
 ( #60858, #99878 ),
 ( #84673, #14661 ),
 ( #36499, #29388 ),
 ( #83167, #23262 ),
 ( #100377, #30890 ),
 ( #91776, #92780 ),
 ( #60367, #84171 ),
 ( #44624, #61359 ),
 ( #85174, #15662 ),
 ( #75548, #90795 ),
 ( #30386, #45624 ),
 ( #7053, #46631 ),
 ( #83673, #6052 ),
 ( #37504, #92286 ),
 ( #99395, #29890 ),
 ( #67971, #67464 ),
 ( #59859, #46126 ),
 ( #22758, #21264 ),
 ( #22259, #53743 ),
 ( #15159, #52240 ),
 ( #14154, #37005 ),
 ( #45131, #98894 ),
 ( #76055, #54746 ),
 ( #93786, #70460 ),
 ( #56253, #18167 ),
 ( #9551, #41016 ),
 ( #78045, #39001 ),
 ( #25274, #945 ),
 ( #79058, #47631 ),
 ( #87683, #23771 ),
 ( #33385, #62353 ),
 ( #95294, #40519 ),
 ( #64374, #63370 ),
 ( #86676, #71469 ),
 ( #40004, #71970 ),
 ( #39509, #25778 ),
 ( #55249, #70964 ),
 ( #56754, #32901 ),
 ( #77549, #2451 ),
 ( #31895, #32395 ),
 ( #1957, #87178 ),
 ( #24282, #8052 ),
 ( #24768, #69951 ),
 ( #439, #10053 ),
 ( #55750, #31392 ),
 ( #63871, #93279 ),
 ( #1455, #85681 ),
 ( #94284, #16161 ),
 ( #79565, #17164 ),
 ( #48130, #47129 ),
 ( #94786, #8559 ),
 ( #17666, #48639 ),
 ( #62870, #86177 ),
 ( #16661, #78548 ),
 ( #9053, #11058 ),
 ( #58728, #50618 ),
 ( #89678, #96294 ),
 ( #4941, #96789 ),
 ( #10551, #41510 ),
 ( #27285, #66362 ),
 ( #12546, #35886 ),
 ( #4453, #80067 ),
 ( #66857, #65870 ),
 ( #58240, #18658 ),
 ( #35405, #81069 ),
 ( #97779, #43512 ),
 ( #81570, #64878 ),
 ( #51118, #57746 ),
 ( #34395, #49140 ),
 ( #49633, #42022 ),
 ( #12044, #95788 ),
 ( #11546, #90175 ),
 ( #72465, #80563 ),
 ( #20153, #2959 ),
 ( #82062, #89183 ),
 ( #97289, #59230 ),
 ( #74449, #57257 ),
 ( #88686, #72967 ),
 ( #19653, #33892 ),
 ( #26279, #3459 ),
 ( #65373, #43014 ),
 ( #88187, #28272 ),
 ( #26781, #19156 ),
 ( #50126, #27776 ),
 ( #42522, #73459 ),
 ( #3952, #73957 ),
 ( #34897, #45012 ),
 ( #7424, #98770 ),
 ( #60240, #38376 ),
 ( #91660, #14535 ),
 ( #68837, #83042 ),
 ( #30259, #22139 ),
 ( #61239, #67850 ),
 ( #76923, #68340 ),
 ( #82554, #13037 ),
 ( #21148, #99273 ),
 ( #69329, #84549 ),
 ( #74929, #76425 ),
 ( #6436, #100249 ),
 ( #52118, #51621 ),
 ( #6932, #52611 ),
 ( #30766, #15035 ),
 ( #53124, #36385 ),
 ( #22634, #29270 ),
 ( #5930, #20649 ),
 ( #53626, #59737 ),
 ( #61738, #43996 ),
 ( #92159, #5434 ),
 ( #46006, #67348 ),
 ( #98267, #36883 ),
 ( #28774, #90670 ),
 ( #84053, #13532 ),
 ( #29771, #44504 ),
 ( #75429, #91167 ),
 ( #60736, #21638 ),
 ( #83550, #75932 ),
 ( #14030, #37392 ),
 ( #45511, #37884 ),
 ( #99755, #70335 ),
 ( #54123, #48006 ),
 ( #16031, #94665 ),
 ( #62741, #94159 ),
 ( #79438, #24150 ),
 ( #31771, #818 ),
 ( #77423, #9424 ),
 ( #9930, #78430 ),
 ( #1331, #86554 ),
 ( #55117, #71340 ),
 ( #317, #46997 ),
 ( #92655, #85047 ),
 ( #25147, #93152 ),
 ( #40389, #48509 ),
 ( #40884, #46496 ),
 ( #23135, #8929 ),
 ( #39880, #77921 ),
 ( #62233, #31263 ),
 ( #86053, #71844 ),
 ( #87053, #2334 ),
 ( #7926, #8431 ),
 ( #33263, #32265 ),
 ( #93656, #39381 ),
 ( #16528, #15532 ),
 ( #23642, #63749 ),
 ( #38874, #56127 ),
 ( #24643, #70838 ),
 ( #69837, #54612 ),
 ( #63236, #55625 ),
 ( #85548, #17543 ),
 ( #47503, #17039 ),
 ( #78930, #1831 ),
 ( #32766, #4823 ),
 ( #88066, #80446 ),
 ( #96666, #42895 ),
 ( #20043, #27164 ),
 ( #10428, #64757 ),
 ( #95172, #26664 ),
 ( #58126, #58614 ),
 ( #88565, #74332 ),
 ( #89063, #51006 ),
 ( #57624, #49009 ),
 ( #19039, #81940 ),
 ( #66246, #73342 ),
 ( #18543, #50014 ),
 ( #79941, #26157 ),
 ( #12426, #41903 ),
 ( #3345, #43394 ),
 ( #35282, #64250 ),
 ( #19537, #49512 ),
 ( #25656, #34282 ),
 ( #56629, #89558 ),
 ( #50499, #41389 ),
 ( #97171, #72845 ),
 ( #10936, #87558 ),
 ( #27665, #2839 ),
 ( #18045, #72345 ),
 ( #33774, #95673 ),
 ( #57131, #65254 ),
 ( #11432, #4331 ),
 ( #96179, #80948 ),
 ( #81454, #42410 ),
 ( #3835, #34777 ),
 ( #65745, #11931 ),
 ( #73832, #28162 ),
 ( #51503, #91048 ),
 ( #22515, #99637 ),
 ( #30140, #29648 ),
 ( #82928, #13416 ),
 ( #6807, #61114 ),
 ( #98649, #90549 ),
 ( #5812, #37269 ),
 ( #53508, #67735 ),
 ( #75317, #44391 ),
 ( #20528, #53004 ),
 ( #84431, #21521 ),
 ( #44892, #60622 ),
 ( #29149, #92044 ),
 ( #90056, #14911 ),
 ( #91543, #22016 ),
 ( #45885, #82434 ),
 ( #76800, #68221 ),
 ( #60121, #35776 ),
 ( #52498, #83427 ),
 ( #43885, #59617 ),
 ( #66747, #99148 ),
 ( #13915, #97663 ),
 ( #76306, #12917 ),
 ( #75814, #68720 ),
 ( #45391, #36770 ),
 ( #74819, #59120 ),
 ( #67235, #6314 ),
 ( #83935, #14414 ),
 ( #5313, #37763 ),
 ( #36275, #98148 ),
 ( #28656, #21028 ),
 ( #51997, #3101 ),
 ( #69720, #26425 ),
 ( #85427, #70215 ),
 ( #95928, #63117 ),
 ( #57394, #34036 ),
 ( #198, #62611 ),
 ( #8816, #86436 ),
 ( #54489, #88322 ),
 ( #54997, #7301 ),
 ( #24028, #65012 ),
 ( #47884, #84930 ),
 ( #39256, #40267 ),
 ( #16921, #8311 ),
 ( #46373, #71218 ),
 ( #38252, #38751 ),
 ( #696, #18798 ),
 ( #49774, #69211 ),
 ( #23012, #93034 ),
 ( #15913, #100127 ),
 ( #30647, #23514 ),
 ( #77306, #31642 ),
 ( #61621, #15413 ),
 ( #92538, #54000 ),
 ( #7808, #31143 ),
 ( #46880, #78310 ),
 ( #85937, #16409 ),
 ( #62113, #77799 ),
 ( #93532, #47383 ),
 ( #39753, #70712 ),
 ( #1209, #32141 ),
 ( #94042, #24526 ),
 ( #55496, #78802 ),
 ( #9300, #75072 ),
 ( #58381, #58873 ),
 ( #5572, #11194 ),
 ( #82691, #82195 ),
 ( #4590, #90812 ),
 ( #5072, #27424 ),
 ( #89813, #51759 ),
 ( #42166, #43153 ),
 ( #12680, #36517 ),
 ( #35540, #21283 ),
 ( #36021, #67483 ),
 ( #28910, #98406 ),
 ( #50763, #73596 ),
 ( #13172, #20283 ),
 ( #4086, #74097 ),
 ( #96430, #42663 ),
 ( #59878, #89319 ),
 ( #19788, #80706 ),
 ( #51256, #74582 ),
 ( #28402, #35038 ),
 ( #90311, #43644 ),
 ( #20782, #81706 ),
 ( #73104, #27914 ),
 ( #12178, #97425 ),
 ( #44143, #3593 ),
 ( #34537, #66510 ),
 ( #65510, #26919 ),
 ( #57889, #19294 ),
 ( #81204, #88827 ),
 ( #66997, #50264 ),
 ( #97909, #11680 ),
 ( #66009, #96929 ),
 ( #59368, #60872 ),
 ( #31411, #91798 ),
 ( #52751, #14170 ),
 ( #84689, #67986 ),
 ( #84186, #93296 ),
 ( #13668, #21776 ),
 ( #92798, #68477 ),
 ( #44641, #77567 ),
 ( #15177, #8070 ),
 ( #61374, #98910 ),
 ( #76073, #54262 ),
 ( #99894, #75569 ),
 ( #29403, #7070 ),
 ( #45146, #46142 ),
 ( #52257, #39018 ),
 ( #38019, #14677 ),
 ( #15681, #69970 ),
 ( #77066, #46647 ),
 ( #29904, #30403 ),
 ( #455, #83184 ),
 ( #6572, #7571 ),
 ( #53760, #23279 ),
 ( #45640, #60384 ),
 ( #22274, #76564 ),
 ( #69472, #68969 ),
 ( #92302, #85191 ),
 ( #38519, #37523 ),
 ( #22772, #100393 ),
 ( #62368, #30906 ),
 ( #61873, #6068 ),
 ( #37023, #91307 ),
 ( #83690, #99410 ),
 ( #53258, #63387 ),
 ( #86694, #9072 ),
 ( #47650, #86196 ),
 ( #56273, #70983 ),
 ( #49159, #64396 ),
 ( #962, #41530 ),
 ( #56771, #95311 ),
 ( #24788, #33912 ),
 ( #87702, #24299 ),
 ( #55768, #18186 ),
 ( #17180, #72485 ),
 ( #31915, #8579 ),
 ( #87197, #63891 ),
 ( #94805, #2979 ),
 ( #40025, #55265 ),
 ( #48151, #17685 ),
 ( #79075, #9572 ),
 ( #16680, #85700 ),
 ( #16180, #25799 ),
 ( #62887, #80085 ),
 ( #40537, #79583 ),
 ( #10568, #33404 ),
 ( #78564, #64895 ),
 ( #1473, #23790 ),
 ( #54762, #71487 ),
 ( #25293, #2470 ),
 ( #32414, #47147 ),
 ( #1975, #78065 ),
 ( #39526, #70478 ),
 ( #93806, #94301 ),
 ( #32918, #48660 ),
 ( #10073, #41035 ),
 ( #71990, #28290 ),
 ( #26301, #26798 ),
 ( #90190, #89697 ),
 ( #44015, #19670 ),
 ( #11074, #81086 ),
 ( #3972, #95804 ),
 ( #57276, #11562 ),
 ( #57761, #27300 ),
 ( #42041, #89201 ),
 ( #36404, #88704 ),
 ( #65394, #88207 ),
 ( #42540, #66380 ),
 ( #20669, #50635 ),
 ( #51637, #74465 ),
 ( #72986, #18675 ),
 ( #97798, #58257 ),
 ( #49649, #73475 ),
 ( #19173, #34913 ),
 ( #27793, #4958 ),
 ( #82573, #58746 ),
 ( #3475, #96311 ),
 ( #51133, #43529 ),
 ( #59249, #97308 ),
 ( #20172, #66872 ),
 ( #81589, #34413 ),
 ( #65887, #12060 ),
 ( #12565, #43031 ),
 ( #73973, #80581 ),
 ( #50144, #4472 ),
 ( #35421, #82081 ),
 ( #13054, #35903 ),
 ( #96808, #74946 ),
 ( #5452, #54144 ),
 ( #99771, #91181 ),
 ( #29787, #21656 ),
 ( #61756, #75446 ),
 ( #77443, #13551 ),
 ( #6453, #75949 ),
 ( #52134, #84567 ),
 ( #85067, #53143 ),
 ( #76445, #61257 ),
 ( #60754, #92674 ),
 ( #29287, #15553 ),
 ( #45030, #91675 ),
 ( #46514, #22652 ),
 ( #92179, #38395 ),
 ( #60258, #22156 ),
 ( #84069, #14555 ),
 ( #5946, #52629 ),
 ( #7944, #30277 ),
 ( #45526, #23152 ),
 ( #7440, #44522 ),
 ( #99290, #100268 ),
 ( #76944, #68357 ),
 ( #36902, #30787 ),
 ( #98284, #98790 ),
 ( #67365, #53643 ),
 ( #28791, #59756 ),
 ( #6948, #15054 ),
 ( #90688, #37902 ),
 ( #37411, #83565 ),
 ( #14049, #68853 ),
 ( #83057, #46025 ),
 ( #21167, #69350 ),
 ( #67865, #31281 ),
 ( #62759, #24660 ),
 ( #87072, #39896 ),
 ( #40901, #56142 ),
 ( #85567, #63255 ),
 ( #8451, #16546 ),
 ( #62250, #71862 ),
 ( #70859, #47522 ),
 ( #86572, #71359 ),
 ( #17563, #55641 ),
 ( #54634, #47019 ),
 ( #78948, #38895 ),
 ( #24167, #32285 ),
 ( #94176, #40406 ),
 ( #48531, #79457 ),
 ( #9447, #335 ),
 ( #9949, #17056 ),
 ( #48023, #77938 ),
 ( #1847, #78446 ),
 ( #69856, #93174 ),
 ( #32785, #39398 ),
 ( #23661, #1350 ),
 ( #16050, #63766 ),
 ( #8948, #94681 ),
 ( #70352, #25167 ),
 ( #55139, #93677 ),
 ( #836, #31790 ),
 ( #86071, #21481 ),
 ( #31101, #76761 ),
 ( #84890, #39213 ),
 ( #38716, #37230 ),
 ( #68680, #91501 ),
 ( #7261, #52459 ),
 ( #6273, #52961 ),
 ( #21980, #61578 ),
 ( #22971, #23471 ),
 ( #6766, #38215 ),
 ( #54452, #60084 ),
 ( #83893, #92500 ),
 ( #68182, #53465 ),
 ( #75773, #53961 ),
 ( #13878, #77759 ),
 ( #15372, #99600 ),
 ( #14874, #62072 ),
 ( #46335, #14374 ),
 ( #85386, #44850 ),
 ( #46841, #15875 ),
 ( #92004, #30103 ),
 ( #77266, #159 ),
 ( #92995, #7769 ),
 ( #84395, #69678 ),
 ( #8273, #70171 ),
 ( #29108, #91008 ),
 ( #83392, #99108 ),
 ( #29605, #60584 ),
 ( #45350, #76272 ),
 ( #37721, #61076 ),
 ( #30605, #22475 ),
 ( #45842, #69171 ),
 ( #100091, #40228 ),
 ( #63585, #85895 ),
 ( #94507, #87905 ),
 ( #2676, #9771 ),
 ( #24988, #95511 ),
 ( #63076, #18387 ),
 ( #78764, #55965 ),
 ( #49356, #56470 ),
 ( #80286, #25997 ),
 ( #24490, #86892 ),
 ( #71181, #17385 ),
 ( #86396, #8776 ),
 ( #94001, #10780 ),
 ( #47842, #48347 ),
 ( #79277, #17890 ),
 ( #64596, #56969 ),
 ( #87396, #31603 ),
 ( #39714, #33615 ),
 ( #62570, #32102 ),
 ( #41744, #95008 ),
 ( #656, #40725 ),
 ( #16375, #71683 ),
 ( #2180, #93495 ),
 ( #23985, #9264 ),
 ( #70673, #1670 ),
 ( #54957, #1167 ),
 ( #47341, #78264 ),
 ( #55458, #33112 ),
 ( #41232, #16880 ),
 ( #32609, #64090 ),
 ( #48853, #25499 ),
 ( #79778, #10275 ),
 ( #72187, #35119 ),
 ( #72684, #88908 ),
 ( #27509, #4168 ),
 ( #36110, #81785 ),
 ( #3182, #96506 ),
 ( #66092, #57969 ),
 ( #19379, #13257 ),
 ( #27002, #50346 ),
 ( #4669, #51340 ),
 ( #28489, #35619 ),
 ( #18880, #73185 ),
 ( #28000, #20365 ),
 ( #74174, #42742 ),
 ( #43728, #59451 ),
 ( #88405, #11768 ),
 ( #97007, #57472 ),
 ( #58464, #90396 ),
 ( #74662, #12257 ),
 ( #81285, #89399 ),
 ( #49861, #34622 ),
 ( #20870, #73675 ),
 ( #19871, #51841 ),
 ( #43236, #66593 ),
 ( #82281, #65591 ),
 ( #12756, #97505 ),
 ( #5159, #50846 ),
 ( #58957, #82775 ),
 ( #89897, #67079 ),
 ( #97989, #34122 ),
 ( #65094, #96013 ),
 ( #26508, #80792 ),
 ( #11273, #42254 ),
 ( #3674, #3998 ),
 ( #57790, #81112 ),
 ( #35446, #11101 ),
 ( #72019, #96339 ),
 ( #26826, #97336 ),
 ( #66416, #95838 ),
 ( #87734, #49189 ),
 ( #19203, #2501 ),
 ( #33437, #79611 ),
 ( #85848, #50174 ),
 ( #3007, #88737 ),
 ( #12090, #42070 ),
 ( #43059, #65917 ),
 ( #74007, #50668 ),
 ( #81616, #11593 ),
 ( #33943, #64923 ),
 ( #58289, #4501 ),
 ( #49683, #41566 ),
 ( #27825, #95339 ),
 ( #17719, #64424 ),
 ( #26331, #57306 ),
 ( #42569, #88237 ),
 ( #73505, #18701 ),
 ( #72516, #41060 ),
 ( #48688, #34940 ),
 ( #25827, #10102 ),
 ( #96834, #27329 ),
 ( #56802, #18218 ),
 ( #89229, #19697 ),
 ( #80112, #73016 ),
 ( #3503, #80611 ),
 ( #10601, #34446 ),
 ( #65423, #91212 ),
 ( #75475, #84100 ),
 ( #99321, #35935 ),
 ( #14585, #12595 ),
 ( #89729, #44551 ),
 ( #5980, #13082 ),
 ( #45558, #91703 ),
 ( #90723, #37931 ),
 ( #83092, #66905 ),
 ( #67901, #21689 ),
 ( #68879, #98822 ),
 ( #67395, #44050 ),
 ( #20698, #21196 ),
 ( #74493, #52162 ),
 ( #99803, #51670 ),
 ( #28321, #51165 ),
 ( #74980, #29317 ),
 ( #36930, #60289 ),
 ( #37438, #52659 ),
 ( #20199, #82605 ),
 ( #13582, #5483 ),
 ( #36431, #58777 ),
 ( #82112, #22187 ),
 ( #83594, #75978 ),
 ( #53171, #76477 ),
 ( #14081, #43557 ),
 ( #6983, #45059 ),
 ( #97826, #4988 ),
 ( #6487, #68389 ),
 ( #59275, #29814 ),
 ( #90225, #98318 ),
 ( #28824, #59789 ),
 ( #60787, #46548 ),
 ( #69382, #31315 ),
 ( #40442, #38431 ),
 ( #15090, #22685 ),
 ( #30310, #62795 ),
 ( #70894, #53672 ),
 ( #55677, #85599 ),
 ( #86603, #8979 ),
 ( #76977, #61288 ),
 ( #32319, #93209 ),
 ( #92212, #77478 ),
 ( #7471, #54178 ),
 ( #94210, #48053 ),
 ( #24201, #24695 ),
 ( #7978, #8485 ),
 ( #17090, #84604 ),
 ( #63291, #31825 ),
 ( #93709, #1385 ),
 ( #62284, #46058 ),
 ( #38929, #23695 ),
 ( #47558, #54669 ),
 ( #16088, #78983 ),
 ( #55176, #85102 ),
 ( #9482, #100302 ),
 ( #71393, #30819 ),
 ( #47057, #69883 ),
 ( #61785, #92704 ),
 ( #86104, #15584 ),
 ( #23193, #367 ),
 ( #77971, #39435 ),
 ( #70384, #874 ),
 ( #16582, #78478 ),
 ( #39931, #63800 ),
 ( #50058, #25703 ),
 ( #3392, #72395 ),
 ( #73393, #89114 ),
 ( #58170, #87103 ),
 ( #19586, #65304 ),
 ( #95222, #34327 ),
 ( #10985, #96228 ),
 ( #64806, #96712 ),
 ( #64299, #50548 ),
 ( #79990, #95721 ),
 ( #81501, #57671 ),
 ( #11980, #27215 ),
 ( #56681, #26210 ),
 ( #26711, #80997 ),
 ( #49062, #42948 ),
 ( #49561, #1877 ),
 ( #94715, #34827 ),
 ( #80490, #19086 ),
 ( #65797, #32823 ),
 ( #88614, #25200 ),
 ( #40935, #56175 ),
 ( #42454, #11479 ),
 ( #72895, #3888 ),
 ( #17595, #48568 ),
 ( #79493, #87613 ),
 ( #10478, #9981 ),
 ( #71896, #18097 ),
 ( #2381, #2890 ),
 ( #33312, #41438 ),
 ( #33820, #57183 ),
 ( #88117, #18584 ),
 ( #41950, #66291 ),
 ( #75865, #21081 ),
 ( #83983, #68271 ),
 ( #81995, #82978 ),
 ( #35822, #74866 ),
 ( #97219, #14462 ),
 ( #28710, #5369 ),
 ( #37325, #91592 ),
 ( #67789, #99200 ),
 ( #29699, #73884 ),
 ( #44440, #98706 ),
 ( #21572, #66795 ),
 ( #12967, #59671 ),
 ( #59164, #12478 ),
 ( #97714, #53052 ),
 ( #20582, #90601 ),
 ( #52047, #91096 ),
 ( #60669, #22071 ),
 ( #29205, #4382 ),
 ( #35330, #13468 ),
 ( #43447, #27713 ),
 ( #74377, #36323 ),
 ( #58660, #98200 ),
 ( #89608, #75364 ),
 ( #5864, #20087 ),
 ( #51055, #82485 ),
 ( #4875, #28207 ),
 ( #36821, #90108 ),
 ( #67282, #51555 ),
 ( #43934, #60173 ),
 ( #13966, #52544 ),
 ( #6367, #83479 ),
 ( #44942, #24075 ),
 ( #92092, #76357 ),
 ( #47428, #7855 ),
 ( #45443, #61667 ),
 ( #22560, #69260 ),
 ( #38303, #77850 ),
 ( #86479, #1259 ),
 ( #8856, #53553 ),
 ( #6861, #744 ),
 ( #100178, #78355 ),
 ( #84483, #69764 ),
 ( #77353, #61171 ),
 ( #54051, #38802 ),
 ( #62664, #244 ),
 ( #31187, #39805 ),
 ( #39304, #30694 ),
 ( #70763, #14964 ),
 ( #63160, #32188 ),
 ( #62161, #84977 ),
 ( #93083, #31696 ),
 ( #54537, #45936 ),
 ( #92583, #94088 ),
 ( #23063, #37813 ),
 ( #68765, #76846 ),
 ( #15462, #46422 ),
 ( #24572, #70260 ),
 ( #23568, #85473 ),
 ( #16457, #55549 ),
 ( #15958, #46924 ),
 ( #99685, #7348 ),
 ( #30189, #8355 ),
 ( #93579, #55044 ),
 ( #85982, #34208 ),
 ( #3761, #2761 ),
 ( #26082, #10864 ),
 ( #79862, #11361 ),
 ( #79362, #34702 ),
 ( #95097, #10356 ),
 ( #65673, #72773 ),
 ( #41827, #88491 ),
 ( #41313, #96589 ),
 ( #72272, #33701 ),
 ( #25072, #40805 ),
 ( #27088, #49439 ),
 ( #64679, #42334 ),
 ( #57552, #94591 ),
 ( #48933, #49944 ),
 ( #26592, #17974 ),
 ( #56050, #80874 ),
 ( #18967, #65177 ),
 ( #95595, #58054 ),
 ( #73268, #16965 ),
 ( #57054, #80373 ),
 ( #47929, #87990 ),
 ( #25581, #2260 ),
 ( #9854, #18467 ),
 ( #32690, #3267 ),
 ( #78852, #71768 ),
 ( #86976, #9350 ),
 ( #33193, #96104 ),
 ( #40313, #71262 ),
 ( #1753, #63671 ),
 ( #17468, #64175 ),
 ( #48431, #56555 ),
 ( #87482, #13836 ),
 ( #29070, #66174 ),
 ( #44811, #42823 ),
 ( #19460, #74743 ),
 ( #5240, #43318 ),
 ( #75731, #21441 ),
 ( #82854, #51426 ),
 ( #12840, #97093 ),
 ( #98070, #51924 ),
 ( #99068, #28578 ),
 ( #97586, #74255 ),
 ( #50931, #20453 ),
 ( #4253, #82361 ),
 ( #29567, #81868 ),
 ( #58542, #81370 ),
 ( #4749, #59538 ),
 ( #43809, #20952 ),
 ( #67657, #90477 ),
 ( #50428, #12347 ),
 ( #36198, #35700 ),
 ( #66676, #88990 ),
 ( #28088, #59041 ),
 ( #13337, #98575 ),
 ( #6232, #44317 ),
 ( #35203, #89482 ),
 ( #75244, #36690 ),
 ( #5735, #83353 ),
 ( #67162, #11854 ),
 ( #60043, #37187 ),
 ( #90972, #73754 ),
 ( #52421, #68143 ),
 ( #27591, #19959 ),
 ( #89980, #22929 ),
 ( #76230, #22437 ),
 ( #47304, #38169 ),
 ( #100052, #78228 ),
 ( #31058, #54412 ),
 ( #8236, #92455 ),
 ( #6729, #53918 ),
 ( #1128, #53420 ),
 ( #30061, #52922 ),
 ( #76720, #62030 ),
 ( #85861, #15331 ),
 ( #70632, #54917 ),
 ( #68641, #69640 ),
 ( #84349, #61538 ),
 ( #7221, #60544 ),
 ( #14832, #69129 ),
 ( #92955, #39177 ),
 ( #16337, #23430 ),
 ( #37681, #61035 ),
 ( #15833, #70131 ),
 ( #62527, #85347 ),
 ( #46803, #31565 ),
 ( #84852, #99559 ),
 ( #30566, #46293 ),
 ( #77222, #8739 ),
 ( #93456, #118 ),
 ( #45799, #7729 ),
 ( #91966, #38676 ),
 ( #39678, #77723 ),
 ( #620, #91460 ),
 ( #23949, #21937 ),
 ( #83855, #14332 ),
 ( #45310, #71644 ),
 ( #94968, #17347 ),
 ( #88366, #79741 ),
 ( #93962, #24454 ),
 ( #32567, #10235 ),
 ( #18844, #95975 ),
 ( #3145, #41707 ),
 ( #42215, #71143 ),
 ( #63549, #72649 ),
 ( #48307, #2638 ),
 ( #25457, #80757 ),
 ( #9225, #16844 ),
 ( #34086, #40691 ),
 ( #79238, #32066 ),
 ( #65057, #1635 ),
 ( #56434, #40189 ),
 ( #41197, #95475 ),
 ( #73148, #72151 ),
 ( #2144, #9736 ),
 ( #94470, #64056 ),
 ( #24953, #26473 ),
 ( #55422, #57436 ),
 ( #86360, #49825 ),
 ( #33578, #47803 ),
 ( #87356, #64556 ),
 ( #10743, #25960 ),
 ( #33078, #11239 ),
 ( #17854, #56932 ),
 ( #63041, #78722 ),
 ( #48816, #55928 ),
 ( #86849, #87866 ),
 ( #18351, #49319 ),
 ( #80251, #65556 ),
 ( #66560, #58430 ),
 ( #98455, #11729 ),
 ( #13723, #50311 ),
 ( #59929, #88874 ),
 ( #21328, #67045 ),
 ( #96973, #36074 ),
 ( #34585, #89362 ),
 ( #82242, #52305 ),
 ( #27963, #57934 ),
 ( #81749, #97471 ),
 ( #90857, #59413 ),
 ( #83240, #28956 ),
 ( #27473, #58918 ),
 ( #43199, #89861 ),
 ( #50809, #44694 ),
 ( #51302, #3638 ),
 ( #96471, #36565 ),
 ( #12721, #20832 ),
 ( #67535, #26960 ),
 ( #13221, #4632 ),
 ( #42706, #19345 ),
 ( #44194, #51809 ),
 ( #74628, #97953 ),
 ( #81246, #20330 ),
 ( #28450, #73640 ),
 ( #43690, #4132 ),
 ( #90359, #35081 ),
 ( #66053, #19831 ),
 ( #5122, #12222 ),
 ( #74140, #35586 ),
 ( #82739, #75129 ),
 ( #5621, #29448 ),
 ( #30459, #12 ),
 ( #506, #85748 ),
 ( #46187, #69529 ),
 ( #23328, #37573 ),
 ( #85239, #77115 ),
 ( #15728, #22326 ),
 ( #31458, #22822 ),
 ( #53304, #92350 ),
 ( #46697, #77617 ),
 ( #39068, #62422 ),
 ( #30954, #6119 ),
 ( #93346, #53807 ),
 ( #83738, #23837 ),
 ( #76121, #7117 ),
 ( #54810, #70019 ),
 ( #7622, #91353 ),
 ( #8129, #84237 ),
 ( #16232, #14723 ),
 ( #6620, #68525 ),
 ( #38572, #21828 ),
 ( #38065, #75613 ),
 ( #37070, #45194 ),
 ( #68035, #91852 ),
 ( #98960, #84741 ),
 ( #61920, #60429 ),
 ( #52805, #14218 ),
 ( #99455, #29955 ),
 ( #60923, #45689 ),
 ( #76613, #69022 ),
 ( #99946, #92849 ),
 ( #61423, #15229 ),
 ( #54313, #93854 ),
 ( #8627, #2527 ),
 ( #57327, #41591 ),
 ( #10629, #32462 ),
 ( #9121, #48199 ),
 ( #39574, #88257 ),
 ( #79130, #33964 ),
 ( #64946, #72535 ),
 ( #3029, #94356 ),
 ( #25346, #18240 ),
 ( #78114, #9624 ),
 ( #79630, #95860 ),
 ( #71536, #47196 ),
 ( #72041, #26353 ),
 ( #70526, #1015 ),
 ( #17233, #40079 ),
 ( #49209, #56324 ),
 ( #71033, #40586 ),
 ( #62934, #1522 ),
 ( #2030, #33457 ),
 ( #31961, #24348 ),
 ( #17740, #41087 ),
 ( #95362, #63437 ),
 ( #56824, #48709 ),
 ( #87755, #24843 ),
 ( #55314, #94856 ),
 ( #55817, #63947 ),
 ( #80138, #86248 ),
 ( #16728, #32970 ),
 ( #47695, #78614 ),
 ( #86745, #87245 ),
 ( #10123, #64447 ),
 ( #25847, #89754 ),
 ( #37833, #13113 ),
 ( #51195, #34471 ),
 ( #20725, #27355 ),
 ( #99704, #58316 ),
 ( #19233, #81139 ),
 ( #82137, #65445 ),
 ( #50695, #61192 ),
 ( #80640, #88762 ),
 ( #59307, #34968 ),
 ( #11125, #44077 ),
 ( #12622, #43581 ),
 ( #18731, #76378 ),
 ( #82628, #96364 ),
 ( #74521, #66932 ),
 ( #51695, #20225 ),
 ( #5013, #90251 ),
 ( #81642, #26853 ),
 ( #89254, #12114 ),
 ( #35962, #43087 ),
 ( #4525, #6879 ),
 ( #97850, #42596 ),
 ( #68788, #57822 ),
 ( #30209, #49709 ),
 ( #28344, #42094 ),
 ( #73041, #3526 ),
 ( #50197, #11617 ),
 ( #74031, #73531 ),
 ( #35474, #4022 ),
 ( #65942, #96864 ),
 ( #19721, #66442 ),
 ( #97367, #27848 ),
 ( #58805, #9372 ),
 ( #24593, #63182 ),
 ( #77871, #78871 ),
 ( #46443, #100197 ),
 ( #55567, #92604 ),
 ( #71285, #40332 ),
 ( #47950, #24094 ),
 ( #77374, #94106 ),
 ( #92112, #7875 ),
 ( #38823, #86500 ),
 ( #23586, #55064 ),
 ( #85495, #54556 ),
 ( #16984, #22580 ),
 ( #39322, #32207 ),
 ( #30717, #1773 ),
 ( #8377, #47447 ),
 ( #32711, #53577 ),
 ( #69786, #84502 ),
 ( #93105, #70285 ),
 ( #14985, #7370 ),
 ( #15977, #45956 ),
 ( #76868, #765 ),
 ( #38322, #23082 ),
 ( #69282, #54073 ),
 ( #61686, #84997 ),
 ( #15481, #86002 ),
 ( #263, #31208 ),
 ( #62181, #46948 ),
 ( #31717, #62683 ),
 ( #93600, #16476 ),
 ( #78375, #8880 ),
 ( #39824, #70782 ),
 ( #1279, #3780 ),
 ( #34226, #56068 ),
 ( #18489, #96121 ),
 ( #42354, #72790 ),
 ( #48453, #72290 ),
 ( #64701, #10882 ),
 ( #73774, #79383 ),
 ( #95617, #50445 ),
 ( #81392, #58075 ),
 ( #89008, #10375 ),
 ( #64194, #25093 ),
 ( #11378, #87506 ),
 ( #65198, #33721 ),
 ( #34718, #11873 ),
 ( #9875, #2782 ),
 ( #26104, #40826 ),
 ( #57074, #42844 ),
 ( #65693, #3290 ),
 ( #17992, #88009 ),
 ( #49460, #17489 ),
 ( #41335, #80393 ),
 ( #4274, #18984 ),
 ( #63693, #19482 ),
 ( #48953, #41848 ),
 ( #26610, #57573 ),
 ( #79882, #71788 ),
 ( #25604, #94613 ),
 ( #88509, #49963 ),
 ( #96608, #27105 ),
 ( #86997, #80892 ),
 ( #73286, #2284 ),
 ( #33214, #95115 ),
 ( #56574, #36217 ),
 ( #45332, #43338 ),
 ( #19982, #27612 ),
 ( #35223, #67677 ),
 ( #75753, #58561 ),
 ( #37211, #82872 ),
 ( #90991, #76253 ),
 ( #60565, #99089 ),
 ( #5259, #98093 ),
 ( #66194, #51445 ),
 ( #12366, #59064 ),
 ( #28106, #98597 ),
 ( #97115, #91483 ),
 ( #29588, #81889 ),
 ( #21961, #89501 ),
 ( #90001, #29090 ),
 ( #74277, #59561 ),
 ( #4768, #60064 ),
 ( #43829, #28600 ),
 ( #52441, #90496 ),
 ( #20972, #68163 ),
 ( #21462, #20475 ),
 ( #52944, #50951 ),
 ( #83874, #14354 ),
 ( #51943, #74763 ),
 ( #83372, #6254 ),
 ( #35722, #13861 ),
 ( #13359, #66695 ),
 ( #44335, #82382 ),
 ( #12861, #97606 ),
 ( #44832, #67181 ),
 ( #75264, #5757 ),
 ( #36712, #24475 ),
 ( #39698, #78249 ),
 ( #7750, #16864 ),
 ( #70658, #7243 ),
 ( #23969, #22952 ),
 ( #639, #69662 ),
 ( #63062, #39196 ),
 ( #92478, #8760 ),
 ( #99581, #32086 ),
 ( #62552, #47824 ),
 ( #93984, #1150 ),
 ( #55441, #69152 ),
 ( #54436, #30086 ),
 ( #22458, #62053 ),
 ( #86381, #6749 ),
 ( #37703, #31587 ),
 ( #68663, #53444 ),
 ( #61057, #93477 ),
 ( #30588, #91987 ),
 ( #14855, #31081 ),
 ( #84374, #54939 ),
 ( #45822, #76741 ),
 ( #70154, #77246 ),
 ( #92978, #38194 ),
 ( #85881, #61559 ),
 ( #100072, #53943 ),
 ( #84873, #23453 ),
 ( #16358, #15354 ),
 ( #46318, #77742 ),
 ( #38696, #47326 ),
 ( #85370, #139 ),
 ( #15855, #46826 ),
 ( #8258, #34605 ),
 ( #78747, #40209 ),
 ( #11258, #79258 ),
 ( #95995, #65576 ),
 ( #32590, #34106 ),
 ( #64577, #96491 ),
 ( #33096, #86874 ),
 ( #42236, #9755 ),
 ( #57954, #26983 ),
 ( #88892, #10764 ),
 ( #64075, #80776 ),
 ( #9248, #94990 ),
 ( #25478, #73168 ),
 ( #79762, #19365 ),
 ( #72170, #10257 ),
 ( #40710, #71164 ),
 ( #1654, #18866 ),
 ( #63569, #3659 ),
 ( #49339, #17872 ),
 ( #33597, #41218 ),
 ( #17369, #2164 ),
 ( #94489, #41728 ),
 ( #95495, #24973 ),
 ( #49843, #55947 ),
 ( #48330, #71665 ),
 ( #56453, #25981 ),
 ( #56952, #87378 ),
 ( #48836, #2661 ),
 ( #87886, #18371 ),
 ( #80270, #72667 ),
 ( #3165, #65078 ),
 ( #26493, #57456 ),
 ( #88386, #83259 ),
 ( #51323, #98976 ),
 ( #43711, #82265 ),
 ( #12239, #11750 ),
 ( #42728, #90875 ),
 ( #20853, #73659 ),
 ( #5142, #82759 ),
 ( #28973, #59437 ),
 ( #35105, #58939 ),
 ( #12740, #35606 ),
 ( #66577, #91370 ),
 ( #74159, #97490 ),
 ( #68051, #44710 ),
 ( #13241, #13739 ),
 ( #50829, #4153 ),
 ( #98475, #97972 ),
 ( #90378, #81769 ),
 ( #21347, #37088 ),
 ( #66074, #89880 ),
 ( #74647, #96993 ),
 ( #36095, #29465 ),
 ( #52324, #51829 ),
 ( #28472, #60449 ),
 ( #67064, #27492 ),
 ( #44215, #75148 ),
 ( #75634, #50330 ),
 ( #6136, #5638 ),
 ( #27984, #36584 ),
 ( #81267, #58449 ),
 ( #89382, #67556 ),
 ( #19853, #59948 ),
 ( #43221, #4652 ),
 ( #20350, #78130 ),
 ( #22341, #53827 ),
 ( #39590, #16252 ),
 ( #68541, #30475 ),
 ( #23855, #61441 ),
 ( #7133, #21845 ),
 ( #54830, #60939 ),
 ( #70542, #31980 ),
 ( #93364, #6635 ),
 ( #83755, #91870 ),
 ( #62437, #14236 ),
 ( #85765, #69548 ),
 ( #77636, #62948 ),
 ( #47211, #8645 ),
 ( #1030, #84255 ),
 ( #28, #45211 ),
 ( #37591, #77134 ),
 ( #52820, #76138 ),
 ( #99473, #15748 ),
 ( #69037, #99965 ),
 ( #29970, #8147 ),
 ( #30971, #53325 ),
 ( #14740, #46202 ),
 ( #45706, #46713 ),
 ( #76632, #38083 ),
 ( #85255, #92368 ),
 ( #54330, #84758 ),
 ( #22839, #15246 ),
 ( #7642, #61938 ),
 ( #38588, #92868 ),
 ( #23345, #39084 ),
 ( #70038, #526 ),
 ( #31477, #25866 ),
 ( #64464, #32988 ),
 ( #48726, #56341 ),
 ( #1538, #17249 ),
 ( #63963, #86760 ),
 ( #25361, #24364 ),
 ( #47714, #72059 ),
 ( #2541, #17756 ),
 ( #80655, #71553 ),
 ( #94871, #11140 ),
 ( #64964, #42110 ),
 ( #56840, #87261 ),
 ( #79644, #10645 ),
 ( #10141, #79146 ),
 ( #48217, #55834 ),
 ( #87772, #40602 ),
 ( #18744, #33981 ),
 ( #71049, #73056 ),
 ( #95875, #3043 ),
 ( #3541, #32479 ),
 ( #94373, #26369 ),
 ( #9642, #95378 ),
 ( #41104, #34483 ),
 ( #18254, #33473 ),
 ( #49227, #80156 ),
 ( #41607, #93873 ),
 ( #2046, #24859 ),
 ( #72551, #57342 ),
 ( #88274, #78629 ),
 ( #49723, #55331 ),
 ( #86264, #16744 ),
 ( #9136, #40095 ),
 ( #63453, #21235 ),
 ( #74535, #4038 ),
 ( #74043, #35487 ),
 ( #50707, #65459 ),
 ( #6019, #42609 ),
 ( #81657, #58329 ),
 ( #59827, #59319 ),
 ( #12128, #43100 ),
 ( #36470, #90760 ),
 ( #51706, #96377 ),
 ( #20239, #73545 ),
 ( #75519, #11631 ),
 ( #52206, #50211 ),
 ( #4541, #34980 ),
 ( #27369, #44592 ),
 ( #66459, #82148 ),
 ( #43595, #82642 ),
 ( #28865, #83134 ),
 ( #20738, #26867 ),
 ( #13621, #12634 ),
 ( #65956, #57834 ),
 ( #96878, #97378 ),
 ( #88777, #19244 ),
 ( #89266, #27862 ),
 ( #67435, #58818 ),
 ( #89767, #81153 ),
 ( #19734, #51207 ),
 ( #5026, #35974 ),
 ( #66944, #97861 ),
 ( #28357, #90262 ),
 ( #5518, #13124 ),
 ( #98360, #44092 ),
 ( #75020, #47100 ),
 ( #62326, #410 ),
 ( #8021, #99362 ),
 ( #84642, #29356 ),
 ( #14123, #60829 ),
 ( #29857, #69426 ),
 ( #78016, #93255 ),
 ( #31362, #83641 ),
 ( #23741, #67939 ),
 ( #36974, #38971 ),
 ( #45101, #61329 ),
 ( #76022, #61826 ),
 ( #21730, #85651 ),
 ( #100344, #7022 ),
 ( #22725, #69924 ),
 ( #30860, #91748 ),
 ( #54715, #52703 ),
 ( #16131, #98863 ),
 ( #99848, #76516 ),
 ( #92748, #60332 ),
 ( #91256, #23232 ),
 ( #7520, #37972 ),
 ( #15630, #6526 ),
 ( #22228, #53211 ),
 ( #37477, #68427 ),
 ( #84139, #14629 ),
 ( #15132, #45596 ),
 ( #68923, #54218 ),
 ( #30355, #92253 ),
 ( #53715, #46095 ),
 ( #85143, #77020 ),
 ( #38475, #46597 ),
 ( #77522, #1426 ),
 ( #40484, #39479 ),
 ( #32362, #71437 ),
 ( #32873, #62838 ),
 ( #63845, #33359 ),
 ( #33868, #18631 ),
 ( #79537, #2426 ),
 ( #93756, #63339 ),
 ( #10025, #40987 ),
 ( #49110, #55722 ),
 ( #64853, #56222 ),
 ( #70431, #917 ),
 ( #80040, #10526 ),
 ( #26257, #1928 ),
 ( #41487, #18140 ),
 ( #49610, #47602 ),
 ( #9027, #72441 ),
 ( #39974, #94758 ),
 ( #57230, #2934 ),
 ( #55221, #17136 ),
 ( #95763, #48103 ),
 ( #94257, #8528 ),
 ( #70938, #24741 ),
 ( #71945, #24248 ),
 ( #25248, #31869 ),
 ( #86149, #78519 ),
 ( #88161, #86649 ),
 ( #16630, #79028 ),
 ( #64347, #9526 ),
 ( #17640, #87151 ),
 ( #48612, #95266 ),
 ( #25755, #56724 ),
 ( #87659, #42501 ),
 ( #27754, #72939 ),
 ( #96269, #35377 ),
 ( #67322, #43977 ),
 ( #74908, #74427 ),
 ( #27262, #58216 ),
 ( #51595, #5413 ),
 ( #66837, #80538 ),
 ( #66340, #88662 ),
 ( #90644, #26754 ),
 ( #19631, #89157 ),
 ( #65352, #97759 ),
 ( #12520, #12023 ),
 ( #34870, #34371 ),
 ( #28751, #89654 ),
 ( #57720, #36366 ),
 ( #4921, #35865 ),
 ( #21121, #19131 ),
 ( #28250, #82530 ),
 ( #3933, #43487 ),
 ( #97263, #42992 ),
 ( #50103, #65843 ),
 ( #59714, #59210 ),
 ( #58704, #98247 ),
 ( #20628, #81043 ),
 ( #73931, #13011 ),
 ( #11032, #20134 ),
 ( #51096, #96763 ),
 ( #42001, #3438 ),
 ( #4426, #11522 ),
 ( #82041, #90153 ),
 ( #73437, #50594 ),
 ( #81550, #92136 ),
 ( #60714, #37370 ),
 ( #14009, #84026 ),
 ( #67828, #45487 ),
 ( #93131, #44985 ),
 ( #21617, #44481 ),
 ( #68313, #22608 ),
 ( #77401, #6905 ),
 ( #30743, #61217 ),
 ( #36864, #84525 ),
 ( #76402, #14512 ),
 ( #75909, #13510 ),
 ( #75406, #92633 ),
 ( #53602, #5907 ),
 ( #37858, #15012 ),
 ( #61710, #45980 ),
 ( #98751, #91633 ),
 ( #68812, #99245 ),
 ( #62209, #29242 ),
 ( #99732, #38853 ),
 ( #69810, #46471 ),
 ( #76894, #15504 ),
 ( #52586, #60212 ),
 ( #100226, #30235 ),
 ( #7396, #83523 ),
 ( #23111, #291 ),
 ( #91141, #22117 ),
 ( #38354, #6414 ),
 ( #29747, #69306 ),
 ( #83021, #53099 ),
 ( #54100, #31240 ),
 ( #85020, #7901 ),
 ( #52092, #48486 ),
 ( #50348, #35121 ),
 ( #94642, #17520 ),
 ( #55599, #25120 ),
 ( #40855, #78904 ),
 ( #8906, #31745 ),
 ( #71316, #23613 ),
 ( #16008, #57971 ),
 ( #1804, #71821 ),
 ( #88910, #81287 ),
 ( #79412, #54587 ),
 ( #11770, #40362 ),
 ( #62714, #42744 ),
 ( #24124, #86528 ),
 ( #73677, #19381 ),
 ( #70314, #32237 ),
 ( #63212, #85523 ),
 ( #46976, #39852 ),
 ( #93628, #24618 ),
 ( #4170, #9401 ),
 ( #9903, #66094 ),
 ( #77899, #56097 ),
 ( #96508, #8403 ),
 ( #87029, #3676 ),
 ( #34624, #65593 ),
 ( #39355, #793 ),
 ( #27004, #70815 ),
 ( #55095, #86028 ),
 ( #16505, #47476 ),
 ( #78405, #1304 ),
 ( #32741, #94135 ),
 ( #17014, #47978 ),
 ( #63724, #74176 ),
 ( #21366, #59963 ),
 ( #74664, #50848 ),
 ( #13259, #5654 ),
 ( #97991, #52340 ),
 ( #97507, #4671 ),
 ( #82283, #59453 ),
 ( #12758, #51342 ),
 ( #35621, #27511 ),
 ( #58466, #75164 ),
 ( #28491, #89401 ),
 ( #5161, #90398 ),
 ( #98490, #28991 ),
 ( #28002, #36604 ),
 ( #58959, #97009 ),
 ( #19873, #66595 ),
 ( #43730, #20367 ),
 ( #90891, #81787 ),
 ( #67573, #12259 ),
 ( #36112, #89899 ),
 ( #43238, #67081 ),
 ( #20872, #51843 ),
 ( #82777, #44233 ),
 ( #45666, #24318 ),
 ( #76591, #78090 ),
 ( #93324, #92823 ),
 ( #15205, #14701 ),
 ( #9096, #69994 ),
 ( #78586, #55291 ),
 ( #86221, #7594 ),
 ( #39046, #31939 ),
 ( #91827, #47171 ),
 ( #62909, #15706 ),
 ( #85218, #71008 ),
 ( #46670, #40051 ),
 ( #77095, #7095 ),
 ( #54290, #47672 ),
 ( #93832, #480 ),
 ( #84714, #23305 ),
 ( #77593, #38044 ),
 ( #8097, #85722 ),
 ( #16704, #1498 ),
 ( #31434, #54787 ),
 ( #68997, #46165 ),
 ( #8603, #62393 ),
 ( #38546, #99921 ),
 ( #22798, #60901 ),
 ( #69502, #23814 ),
 ( #990, #22304 ),
 ( #53282, #16204 ),
 ( #84210, #70501 ),
 ( #30432, #61402 ),
 ( #92325, #53784 ),
 ( #100419, #39549 ),
 ( #30930, #61898 ),
 ( #95334, #73009 ),
 ( #72508, #42563 ),
 ( #11586, #41054 ),
 ( #32941, #94829 ),
 ( #64916, #48171 ),
 ( #64417, #73495 ),
 ( #94327, #1995 ),
 ( #3496, #48681 ),
 ( #24812, #57784 ),
 ( #88230, #32435 ),
 ( #88728, #96331 ),
 ( #2494, #25822 ),
 ( #63409, #79605 ),
 ( #9598, #56295 ),
 ( #25319, #95829 ),
 ( #17206, #26819 ),
 ( #50168, #26324 ),
 ( #87217, #57298 ),
 ( #55793, #17711 ),
 ( #56794, #19197 ),
 ( #10095, #81105 ),
 ( #72013, #87728 ),
 ( #86716, #18694 ),
 ( #79099, #40558 ),
 ( #18210, #3001 ),
 ( #33937, #11095 ),
 ( #33432, #71511 ),
 ( #80106, #63915 ),
 ( #49182, #65416 ),
 ( #34437, #10593 ),
 ( #41560, #49676 ),
 ( #42064, #80603 ),
 ( #43053, #36923 ),
 ( #44544, #21189 ),
 ( #74973, #98312 ),
 ( #52652, #28313 ),
 ( #66898, #75469 ),
 ( #44042, #14075 ),
 ( #83588, #12587 ),
 ( #66409, #35927 ),
 ( #19690, #97820 ),
 ( #45052, #97329 ),
 ( #74000, #96826 ),
 ( #20192, #5476 ),
 ( #29309, #59269 ),
 ( #60282, #83084 ),
 ( #4493, #89222 ),
 ( #74487, #90217 ),
 ( #3990, #51157 ),
 ( #20691, #51662 ),
 ( #67892, #21680 ),
 ( #28815, #98815 ),
 ( #50661, #35440 ),
 ( #59781, #52155 ),
 ( #27322, #36424 ),
 ( #67388, #5973 ),
 ( #91205, #82106 ),
 ( #58283, #34933 ),
 ( #90715, #65911 ),
 ( #81609, #12080 ),
 ( #27817, #58770 ),
 ( #82599, #89722 ),
 ( #43550, #13075 ),
 ( #4980, #13575 ),
 ( #70376, #69875 ),
 ( #22678, #53664 ),
 ( #37431, #31306 ),
 ( #23182, #99314 ),
 ( #76470, #77468 ),
 ( #22181, #85590 ),
 ( #39426, #38422 ),
 ( #38921, #46049 ),
 ( #7968, #7463 ),
 ( #30303, #29807 ),
 ( #24192, #85091 ),
 ( #60778, #865 ),
 ( #358, #62275 ),
 ( #86096, #91697 ),
 ( #93200, #47048 ),
 ( #23686, #54660 ),
 ( #16077, #77962 ),
 ( #55169, #31818 ),
 ( #75971, #68381 ),
 ( #8476, #6975 ),
 ( #62787, #93701 ),
 ( #16574, #53164 ),
 ( #6479, #61776 ),
 ( #92695, #61280 ),
 ( #84093, #14579 ),
 ( #45549, #69373 ),
 ( #100293, #37924 ),
 ( #68872, #30811 ),
 ( #99796, #15576 ),
 ( #92203, #84593 ),
 ( #76968, #15082 ),
 ( #54169, #46540 ),
 ( #39924, #49553 ),
 ( #79982, #95215 ),
 ( #41429, #18578 ),
 ( #18088, #87096 ),
 ( #2373, #9973 ),
 ( #55669, #71386 ),
 ( #26704, #10471 ),
 ( #64292, #72885 ),
 ( #88110, #24686 ),
 ( #79486, #80482 ),
 ( #57174, #48559 ),
 ( #25696, #1869 ),
 ( #3384, #10978 ),
 ( #72388, #40927 ),
 ( #71889, #49054 ),
 ( #41943, #33304 ),
 ( #57663, #87606 ),
 ( #56168, #32815 ),
 ( #9473, #56671 ),
 ( #63284, #2883 ),
 ( #88606, #40433 ),
 ( #17082, #70887 ),
 ( #63792, #33813 ),
 ( #64797, #95714 ),
 ( #26202, #34319 ),
 ( #32310, #17587 ),
 ( #65296, #94708 ),
 ( #25191, #47549 ),
 ( #96220, #78471 ),
 ( #8971, #1377 ),
 ( #94201, #86596 ),
 ( #48046, #78976 ),
 ( #74856, #67274 ),
 ( #21071, #74368 ),
 ( #43438, #29194 ),
 ( #28702, #3880 ),
 ( #81986, #36812 ),
 ( #89599, #11972 ),
 ( #52039, #28199 ),
 ( #42940, #12469 ),
 ( #34818, #81492 ),
 ( #5856, #97208 ),
 ( #58651, #67780 ),
 ( #98698, #4864 ),
 ( #35813, #59662 ),
 ( #59156, #60165 ),
 ( #19078, #27705 ),
 ( #19578, #73874 ),
 ( #51545, #65789 ),
 ( #51047, #50051 ),
 ( #80989, #89104 ),
 ( #90592, #35322 ),
 ( #82968, #66787 ),
 ( #75356, #98192 ),
 ( #58161, #96704 ),
 ( #20079, #97705 ),
 ( #11472, #66283 ),
 ( #27207, #4374 ),
 ( #90100, #82477 ),
 ( #42446, #73385 ),
 ( #13458, #50538 ),
 ( #20574, #5360 ),
 ( #12957, #43926 ),
 ( #36314, #44432 ),
 ( #37315, #237 ),
 ( #91583, #6850 ),
 ( #7846, #84474 ),
 ( #76838, #93076 ),
 ( #84968, #14454 ),
 ( #85465, #6359 ),
 ( #8347, #77840 ),
 ( #53543, #30180 ),
 ( #46414, #62153 ),
 ( #23560, #75855 ),
 ( #23053, #92575 ),
 ( #69755, #31179 ),
 ( #70252, #46916 ),
 ( #91087, #52535 ),
 ( #54530, #22063 ),
 ( #68262, #39295 ),
 ( #15950, #735 ),
 ( #92082, #31688 ),
 ( #21563, #53044 ),
 ( #83471, #83974 ),
 ( #13958, #44934 ),
 ( #30685, #99190 ),
 ( #29691, #99677 ),
 ( #45433, #76349 ),
 ( #54043, #60661 ),
 ( #22552, #37805 ),
 ( #68757, #61163 ),
 ( #14954, #45927 ),
 ( #7340, #38295 ),
 ( #69251, #100169 ),
 ( #61656, #15454 ),
 ( #77346, #38795 ),
 ( #62655, #78843 ),
 ( #39796, #86472 ),
 ( #55541, #96463 ),
 ( #4624, #19822 ),
 ( #27463, #8848 ),
 ( #24066, #19333 ),
 ( #11229, #85973 ),
 ( #70754, #88357 ),
 ( #1251, #73632 ),
 ( #58421, #26464 ),
 ( #81239, #57427 ),
 ( #49815, #66046 ),
 ( #57925, #16958 ),
 ( #89355, #78347 ),
 ( #81739, #50800 ),
 ( #18833, #1744 ),
 ( #50303, #35073 ),
 ( #96963, #47419 ),
 ( #26952, #65546 ),
 ( #42698, #4123 ),
 ( #43190, #12214 ),
 ( #93571, #55036 ),
 ( #74131, #63153 ),
 ( #11718, #16449 ),
 ( #32180, #94079 ),
 ( #63662, #24564 ),
 ( #47922, #9343 ),
 ( #40306, #71255 ),
 ( #32683, #94584 ),
 ( #80745, #42206 ),
 ( #3629, #73138 ),
 ( #34578, #88866 ),
 ( #67522, #68023 ),
 ( #28947, #98445 ),
 ( #97943, #97461 ),
 ( #27952, #76108 ),
 ( #6107, #58908 ),
 ( #98950, #91839 ),
 ( #44684, #74617 ),
 ( #44182, #5610 ),
 ( #20822, #35573 ),
 ( #76603, #12712 ),
 ( #51797, #28438 ),
 ( #14209, #66551 ),
 ( #29439, #99446 ),
 ( #36060, #89849 ),
 ( #83728, #83230 ),
 ( #90848, #43678 ),
 ( #45680, #82232 ),
 ( #20319, #29942 ),
 ( #53294, #60418 ),
 ( #22316, #21319 ),
 ( #75602, #91342 ),
 ( #59916, #60913 ),
 ( #59402, #84224 ),
 ( #13210, #52292 ),
 ( #14713, #21817 ),
 ( #52792, #6610 ),
 ( #90350, #45184 ),
 ( #37058, #37562 ),
 ( #82729, #51291 ),
 ( #13710, #5111 ),
 ( #67036, #68513 ),
 ( #75115, #36554 ),
 ( #71023, #63425 ),
 ( #16718, #8114 ),
 ( #46177, #40069 ),
 ( #94343, #1513 ),
 ( #39058, #86733 ),
 ( #32451, #93335 ),
 ( #15717, #55305 ),
 ( #46685, #24830 ),
 ( #55807, #1005 ),
 ( #54302, #85230 ),
 ( #78601, #17221 ),
 ( #93845, #7108 ),
 ( #62410, #15220 ),
 ( #48187, #70009 ),
 ( #38055, #494 ),
 ( #70514, #77607 ),
 ( #39564, #31447 ),
 ( #61910, #61413 ),
 ( #69009, #16219 ),
 ( #92338, #99935 ),
 ( #31951, #62923 ),
 ( #30447, #22812 ),
 ( #24335, #9110 ),
 ( #78103, #23827 ),
 ( #54800, #85736 ),
 ( #77106, #30944 ),
 ( #53797, #86236 ),
 ( #47184, #84729 ),
 ( #47686, #7608 ),
 ( #38562, #69516 ),
 ( #15063, #8616 ),
 ( #92836, #23319 ),
 ( #34953, #11605 ),
 ( #73027, #41577 ),
 ( #3018, #80624 ),
 ( #19217, #33954 ),
 ( #89240, #18715 ),
 ( #87744, #64435 ),
 ( #41071, #10616 ),
 ( #94844, #72525 ),
 ( #19709, #72029 ),
 ( #48697, #71526 ),
 ( #2015, #17730 ),
 ( #64933, #11112 ),
 ( #57804, #88246 ),
 ( #63934, #18229 ),
 ( #95850, #95351 ),
 ( #25836, #79119 ),
 ( #2512, #56812 ),
 ( #25335, #42582 ),
 ( #96848, #42082 ),
 ( #33446, #3513 ),
 ( #9613, #49198 ),
 ( #26342, #73519 ),
 ( #80124, #27343 ),
 ( #34458, #65433 ),
 ( #40574, #32958 ),
 ( #96352, #50185 ),
 ( #57315, #26840 ),
 ( #88750, #81124 ),
 ( #49695, #58302 ),
 ( #4009, #56313 ),
 ( #87232, #65928 ),
 ( #79620, #10112 ),
 ( #82616, #83612 ),
 ( #60302, #51683 ),
 ( #89742, #14097 ),
 ( #91226, #67915 ),
 ( #21210, #44565 ),
 ( #45073, #36445 ),
 ( #59290, #98835 ),
 ( #90236, #50682 ),
 ( #81628, #66918 ),
 ( #12607, #13095 ),
 ( #66429, #44063 ),
 ( #91721, #43569 ),
 ( #20210, #43072 ),
 ( #97838, #52176 ),
 ( #75993, #5496 ),
 ( #6501, #29331 ),
 ( #51180, #35459 ),
 ( #20710, #74995 ),
 ( #12102, #28332 ),
 ( #74505, #67411 ),
 ( #83108, #21703 ),
 ( #37451, #13597 ),
 ( #97350, #82123 ),
 ( #5994, #52675 ),
 ( #74017, #90737 ),
 ( #75492, #68402 ),
 ( #98331, #27836 ),
 ( #4512, #36944 ),
 ( #28838, #58791 ),
 ( #5000, #59803 ),
 ( #35948, #99334 ),
 ( #29830, #60801 ),
 ( #39450, #15599 ),
 ( #7992, #24216 ),
 ( #16102, #46070 ),
 ( #16596, #37943 ),
 ( #39947, #8993 ),
 ( #85114, #61798 ),
 ( #77986, #93723 ),
 ( #55191, #6996 ),
 ( #54682, #23711 ),
 ( #887, #62809 ),
 ( #1398, #78493 ),
 ( #22201, #84116 ),
 ( #86119, #22698 ),
 ( #70399, #70907 ),
 ( #47573, #32333 ),
 ( #23205, #63306 ),
 ( #53185, #53685 ),
 ( #14600, #84616 ),
 ( #45572, #76489 ),
 ( #38941, #68892 ),
 ( #31840, #99819 ),
 ( #30325, #7488 ),
 ( #38444, #61300 ),
 ( #54190, #92226 ),
 ( #15104, #76990 ),
 ( #69396, #100316 ),
 ( #85613, #69896 ),
 ( #30833, #92717 ),
 ( #381, #8500 ),
 ( #46562, #77491 ),
 ( #31329, #62298 ),
 ( #93222, #47071 ),
 ( #3902, #9495 ),
 ( #25720, #81013 ),
 ( #11492, #88631 ),
 ( #19100, #40951 ),
 ( #50073, #26225 ),
 ( #72412, #65321 ),
 ( #24711, #80508 ),
 ( #96242, #49079 ),
 ( #18113, #34841 ),
 ( #80006, #73408 ),
 ( #9995, #78998 ),
 ( #87629, #42469 ),
 ( #26726, #2905 ),
 ( #17611, #56698 ),
 ( #40457, #56193 ),
 ( #10494, #18600 ),
 ( #94225, #55691 ),
 ( #64823, #88132 ),
 ( #71406, #48583 ),
 ( #95736, #57199 ),
 ( #34343, #71913 ),
 ( #86619, #41454 ),
 ( #17105, #48070 ),
 ( #57686, #1893 ),
 ( #32839, #33835 ),
 ( #49576, #63814 ),
 ( #94728, #11000 ),
 ( #25215, #87117 ),
 ( #79507, #41967 ),
 ( #2396, #33326 ),
 ( #64317, #95236 ),
 ( #72910, #3407 ) ),
 .UNSPECIFIED., .F., .F., .F.,
 ( 4, 2, 2, 2, 2, 2, 2, 2, 2, 2, 2, 2, 2, 2, 2, 2, 2, 2, 2, 2, 2, 2, 2, 2, 2, 2, 2, 2, 2, 2, 2, 2, 2, 2, 2, 2, 2, 2, 2, 2, 2, 2, 2, 2, 2, 2, 2, 2, 2, 2, 2, 2, 2, 2, 2, 2, 2, 2, 2, 2, 2, 2, 2, 2, 2, 2, 2, 2, 2, 2, 2, 2, 2, 2, 2, 2, 2, 2, 2, 2, 2, 2, 2, 2, 2, 2, 2, 2, 2, 2, 2, 2, 2, 2, 2, 2, 2, 2, 2, 2, 2, 2, 2, 2, 2, 2, 2, 2, 2, 2, 2, 2, 2, 2, 2, 2, 2, 2, 2, 2, 2, 2, 2, 2, 2, 2, 2, 2, 2, 2, 2, 2, 2, 2, 2, 2, 2, 2, 2, 2, 2, 2, 2, 2, 2, 2, 2, 2, 2, 2, 2, 2, 2, 2, 2, 2, 2, 2, 2, 2, 2, 2, 2, 2, 2, 2, 2, 2, 2, 2, 2, 2, 2, 2, 2, 2, 2, 2, 2, 2, 2, 2, 2, 2, 2, 2, 2, 2, 2, 2, 2, 2, 2, 2, 2, 2, 2, 2, 2, 2, 2, 2, 2, 2, 2, 2, 2, 2, 2, 2, 2, 2, 2, 2, 2, 2, 2, 2, 2, 2, 2, 2, 2, 2, 2, 2, 2, 2, 2, 2, 2, 2, 2, 2, 2, 2, 2, 2, 2, 2, 2, 2, 2, 2, 2, 2, 2, 2, 2, 2, 2, 2, 2, 2, 2, 2, 2, 2, 2, 2, 2, 2, 2, 2, 2, 2, 2, 2, 2, 2, 2, 2, 2, 2, 2, 2, 2, 2, 2, 2, 2, 2, 2, 2, 2, 2, 2, 2, 2, 2, 2, 2, 2, 2, 2, 2, 2, 2, 2, 2, 2, 2, 2, 2, 2, 2, 2, 2, 2, 2, 2, 2, 2, 2, 2, 2, 2, 2, 2, 2, 2, 2, 2, 2, 2, 2, 2, 2, 2, 2, 2, 2, 2, 2, 2, 2, 2, 2, 2, 2, 2, 2, 2, 2, 2, 2, 2, 2, 2, 2, 2, 2, 2, 2, 2, 2, 2, 2, 2, 2, 2, 2, 2, 2, 2, 2, 2, 2, 2, 2, 2, 2, 2, 2, 2, 2, 2, 2, 2, 2, 2, 2, 2, 2, 2, 2, 2, 2, 2, 2, 2, 2, 2, 2, 2, 2, 2, 2, 2, 2, 2, 2, 2, 2, 2, 2, 2, 2, 2, 2, 2, 2, 2, 2, 2, 2, 2, 2, 2, 2, 2, 2, 2, 2, 2, 2, 2, 2, 2, 2, 2, 2, 2, 2, 2, 2, 2, 2, 2, 2, 2, 2, 2, 2, 2, 2, 2, 2, 2, 2, 2, 2, 2, 2, 2, 2, 2, 2, 2, 2, 2, 2, 2, 2, 2, 2, 2, 2, 2, 2, 2, 2, 2, 2, 2, 2, 2, 2, 2, 2, 2, 2, 2, 2, 2, 2, 2, 2, 2, 2, 2, 2, 2, 2, 2, 2, 2, 2, 2, 2, 2, 2, 2, 2, 2, 2, 2, 2, 2, 2, 2, 2, 2, 2, 2, 2, 2, 2, 2, 2, 2, 2, 2, 2, 2, 2, 2, 2, 2, 2, 2, 2, 2, 2, 2, 2, 2, 2, 2, 2, 2, 2, 2, 2, 2, 2, 2, 2, 2, 2, 2, 2, 2, 2, 2, 2, 2, 2, 2, 2, 2, 2, 2, 2, 2, 2, 2, 2, 2, 2, 2, 2, 2, 2, 2, 2, 2, 2, 2, 2, 2, 2, 2, 2, 2, 2, 2, 2, 2, 2, 2, 2, 2, 2, 2, 2, 2, 2, 2, 2, 2, 2, 2, 2, 2, 2, 2, 2, 2, 2, 2, 2, 2, 2, 2, 2, 2, 2, 2, 2, 2, 2, 2, 2, 2, 2, 2, 2, 2, 2, 2, 2, 2, 2, 2, 2, 2, 2, 2, 2, 2, 2, 2, 2, 2, 2, 2, 2, 2, 2, 2, 2, 2, 2, 2, 2, 2, 2, 2, 2, 2, 2, 2, 2, 2, 2, 2, 2, 2, 2, 2, 2, 2, 2, 2, 2, 2, 2, 2, 2, 2, 2, 2, 2, 2, 2, 2, 2, 2, 2, 2, 2, 2, 2, 2, 2, 2, 2, 2, 2, 2, 2, 2, 2, 2, 2, 2, 2, 2, 2, 2, 2, 2, 2, 2, 2, 2, 2, 2, 2, 2, 2, 2, 2, 2, 2, 2, 2, 2, 2, 2, 2, 2, 2, 2, 2, 2, 2, 2, 2, 2, 2, 2, 2, 2, 2, 2, 2, 2, 2, 2, 2, 2, 2, 2, 2, 2, 2, 2, 2, 2, 2, 2, 2, 2, 2, 2, 2, 2, 2, 2, 2, 2, 2, 2, 2, 2, 2, 2, 2, 2, 2, 2, 2, 2, 2, 2, 2, 2, 2, 2, 2, 2, 2, 2, 2, 2, 2, 2, 2, 2, 2, 2, 2, 2, 2, 2, 2, 2, 2, 2, 2, 2, 2, 2, 2, 2, 2, 2, 2, 2, 2, 2, 2, 2, 2, 2, 2, 2, 2, 2, 2, 2, 2, 2, 2, 2, 2, 2, 2, 2, 2, 2, 2, 2, 2, 2, 2, 2, 2, 2, 2, 2, 2, 2, 2, 2, 2, 2, 2, 2, 2, 2, 2, 2, 2, 2, 2, 2, 2, 2, 2, 2, 2, 2, 2, 2, 2, 2, 2, 2, 2, 2, 2, 2, 2, 2, 2, 2, 2, 2, 2, 2, 2, 2, 2, 2, 2, 2, 2, 2, 2, 2, 2, 2, 2, 2, 2, 2, 2, 2, 2, 2, 2, 2, 2, 2, 2, 2, 2, 2, 2, 2, 2, 2, 2, 2, 2, 2, 2, 2, 2, 2, 2, 2, 2, 2, 2, 2, 2, 2, 2, 2, 2, 2, 2, 2, 2, 2, 2, 2, 2, 2, 2, 2, 2, 2, 2, 2, 2, 2, 2, 2, 2, 2, 2, 2, 2, 2, 2, 2, 2, 2, 2, 2, 2, 2, 2, 2, 2, 2, 2, 2, 2, 2, 2, 2, 2, 2, 2, 2, 2, 2, 2, 2, 2, 2, 2, 2, 2, 2, 2, 2, 2, 2, 2, 2, 2, 2, 2, 2, 2, 2, 2, 2, 2, 2, 2, 2, 2, 2, 2, 2, 2, 2, 2, 2, 2, 2, 2, 2, 2, 2, 2, 2, 2, 2, 2, 2, 2, 2, 2, 2, 2, 2, 2, 2, 2, 2, 2, 2, 2, 2, 2, 2, 2, 2, 2, 2, 2, 2, 2, 2, 2, 2, 2, 2, 2, 2, 2, 2, 2, 2, 2, 2, 2, 2, 2, 2, 2, 2, 2, 2, 2, 2, 2, 2, 2, 2, 2, 2, 2, 2, 2, 2, 2, 2, 2, 2, 2, 2, 2, 2, 2, 2, 2, 2, 2, 2, 2, 2, 2, 2, 2, 2, 2, 2, 2, 2, 2, 2, 2, 2, 2, 2, 2, 2, 2, 2, 2, 2, 2, 2, 2, 2, 2, 2, 2, 2, 2, 2, 2, 2, 2, 2, 2, 2, 2, 2, 2, 2, 2, 2, 2, 2, 2, 2, 2, 2, 2, 2, 2, 2, 2, 2, 2, 2, 2, 2, 2, 2, 2, 2, 2, 2, 2, 2, 2, 2, 2, 2, 2, 2, 2, 2, 2, 2, 2, 2, 2, 2, 2, 2, 2, 2, 2, 2, 2, 2, 2, 2, 2, 2, 2, 2, 2, 2, 2, 2, 2, 2, 2, 2, 2, 2, 2, 2, 2, 2, 2, 2, 2, 2, 2, 2, 2, 2, 2, 2, 2, 2, 2, 2, 2, 2, 2, 2, 2, 2, 2, 2, 2, 2, 2, 2, 2, 2, 2, 2, 2, 2, 2, 2, 2, 2, 2, 2, 2, 2, 2, 2, 2, 2, 2, 2, 2, 2, 2, 2, 2, 2, 2, 2, 2, 2, 2, 2, 2, 2, 2, 2, 2, 2, 2, 2, 2, 2, 2, 2, 2, 2, 2, 2, 2, 2, 2, 2, 2, 2, 2, 2, 2, 2, 2, 2, 2, 2, 2, 2, 2, 2, 2, 2, 2, 2, 2, 2, 2, 2, 2, 2, 2, 2, 2, 2, 2, 2, 2, 2, 2, 2, 2, 2, 2, 2, 2, 2, 2, 2, 2, 2, 2, 2, 2, 2, 2, 2, 2, 2, 2, 2, 2, 2, 2, 2, 2, 2, 2, 2, 2, 2, 2, 2, 2, 2, 2, 2, 2, 2, 2, 2, 2, 2, 2, 2, 2, 2, 2, 2, 2, 2, 2, 2, 2, 2, 2, 2, 2, 2, 2, 2, 2, 2, 2, 2, 2, 2, 2, 2, 2, 2, 2, 2, 2, 2, 2, 2, 2, 2, 2, 2, 2, 2, 2, 2, 2, 2, 2, 2, 2, 2, 2, 2, 2, 2, 2, 2, 2, 2, 2, 2, 2, 2, 2, 2, 2, 2, 2, 2, 2, 2, 2, 2, 2, 2, 2, 2, 2, 2, 2, 2, 2, 2, 2, 2, 2, 2, 2, 2, 2, 2, 2, 2, 2, 2, 2, 2, 2, 2, 2, 2, 2, 2, 2, 2, 2, 2, 2, 2, 2, 2, 2, 2, 2, 2, 2, 2, 2, 2, 2, 2, 2, 2, 2, 2, 2, 2, 2, 2, 2, 2, 2, 2, 2, 2, 2, 2, 2, 2, 2, 2, 2, 2, 2, 2, 2, 2, 2, 2, 2, 2, 2, 2, 2, 2, 2, 2, 2, 2, 2, 2, 2, 2, 2, 2, 2, 2, 2, 2, 2, 2, 2, 2, 2, 2, 2, 2, 2, 2, 2, 2, 2, 2, 2, 2, 2, 2, 2, 2, 2, 2, 2, 2, 2, 2, 2, 2, 2, 2, 2, 2, 2, 2, 2, 2, 2, 2, 2, 2, 2, 2, 2, 2, 2, 2, 2, 2, 2, 2, 2, 2, 2, 2, 2, 2, 2, 2, 2, 2, 2, 2, 2, 2, 2, 2, 2, 2, 2, 2, 2, 2, 2, 2, 2, 2, 2, 2, 2, 2, 2, 2, 2, 2, 2, 2, 2, 2, 2, 2, 2, 2, 2, 2, 2, 2, 2, 2, 2, 2, 2, 2, 2, 2, 2, 2, 2, 2, 2, 2, 2, 2, 2, 2, 2, 2, 2, 2, 2, 2, 2, 2, 2, 2, 2, 2, 2, 2, 2, 2, 2, 2, 2, 2, 2, 2, 2, 2, 2, 2, 2, 2, 2, 2, 2, 2, 2, 2, 2, 2, 2, 2, 2, 2, 2, 2, 2, 2, 2, 2, 2, 2, 2, 2, 2, 2, 2, 2, 2, 2, 2, 2, 2, 2, 2, 2, 2, 2, 2, 2, 2, 2, 2, 2, 2, 2, 2, 2, 2, 2, 2, 2, 2, 2, 2, 2, 2, 2, 2, 2, 2, 2, 2, 2, 2, 2, 2, 2, 2, 2, 2, 2, 2, 2, 2, 2, 2, 2, 2, 2, 2, 2, 2, 2, 2, 2, 2, 2, 2, 2, 2, 2, 2, 2, 2, 2, 2, 2, 2, 2, 2, 2, 2, 2, 2, 2, 2, 2, 2, 2, 2, 2, 2, 2, 2, 2, 2, 2, 2, 2, 2, 2, 2, 2, 2, 2, 2, 2, 2, 2, 2, 2, 2, 2, 2, 2, 2, 2, 2, 2, 2, 2, 2, 2, 2, 2, 2, 2, 2, 2, 2, 2, 2, 2, 2, 2, 2, 2, 2, 2, 2, 2, 2, 2, 2, 2, 2, 2, 2, 2, 2, 2, 2, 2, 2, 2, 2, 2, 2, 2, 2, 2, 2, 2, 2, 2, 2, 2, 2, 2, 2, 2, 2, 2, 2, 2, 2, 2, 2, 2, 2, 2, 2, 2, 2, 2, 2, 2, 2, 2, 2, 2, 2, 2, 2, 2, 2, 2, 2, 2, 2, 2, 2, 2, 2, 2, 2, 2, 2, 2, 2, 2, 2, 2, 2, 2, 2, 2, 2, 2, 2, 2, 2, 2, 2, 2, 2, 2, 2, 2, 2, 2, 2, 2, 2, 2, 2, 2, 2, 2, 2, 2, 2, 2, 2, 2, 2, 2, 2, 2, 2, 2, 2, 2, 2, 2, 2, 2, 2, 2, 2, 2, 2, 2, 2, 2, 2, 2, 2, 2, 2, 2, 2, 2, 2, 2, 2, 2, 2, 2, 2, 2, 2, 2, 2, 2, 2, 2, 2, 2, 2, 2, 2, 2, 2, 2, 2, 2, 2, 2, 2, 2, 2, 2, 2, 2, 2, 2, 2, 2, 2, 2, 2, 2, 2, 2, 2, 2, 2, 2, 2, 2, 2, 2, 2, 2, 2, 2, 2, 2, 2, 2, 2, 2, 2, 2, 2, 2, 2, 2, 2, 2, 2, 2, 2, 2, 2, 2, 2, 4 ),
 ( 2, 2 ),
 ( 0.000000000000000000, 0.0004882812500000001084, 0.0009765625000000002168, 0.001464843750000000434, 0.001953125000000000000, 0.002441406250000000000, 0.002929687499999999566, 0.003417968749999999566, 0.003906249999999999133, 0.004394531249999998265, 0.004882812499999997398, 0.005371093749999997398, 0.005859374999999997398, 0.006347656249999998265, 0.006835937499999998265, 0.007324218749999998265, 0.007812499999999998265, 0.008300781249999998265, 0.008789062499999998265, 0.009277343749999998265, 0.009765624999999998265, 0.01025390624999999827, 0.01074218749999999827, 0.01123046874999999827, 0.01171874999999999827, 0.01220703125000000000, 0.01269531250000000000, 0.01318359375000000000, 0.01367187500000000000, 0.01416015625000000000, 0.01464843750000000000, 0.01513671875000000000, 0.01562500000000000000, 0.01611328125000000000, 0.01660156250000000000, 0.01708984375000000000, 0.01757812500000000000, 0.01806640625000000000, 0.01855468750000000000, 0.01904296875000000000, 0.01953125000000000000, 0.02001953125000000000, 0.02050781250000000000, 0.02099609375000000000, 0.02148437500000000000, 0.02197265625000000000, 0.02246093750000000000, 0.02294921875000000000, 0.02343750000000000000, 0.02392578125000000347, 0.02441406250000000347, 0.02490234375000000347, 0.02539062500000000347, 0.02587890625000000347, 0.02636718750000000347, 0.02685546875000000347, 0.02734375000000000347, 0.02783203125000000347, 0.02832031250000000347, 0.02880859375000000347, 0.02929687500000000347, 0.02978515625000000347, 0.03027343750000000347, 0.03076171875000000347, 0.03125000000000000000, 0.03173828125000000000, 0.03222656250000000000, 0.03271484375000000000, 0.03320312500000000000, 0.03369140625000000000, 0.03417968750000000000, 0.03466796875000000000, 0.03515625000000000000, 0.03564453125000000000, 0.03613281250000000000, 0.03662109375000000000, 0.03710937500000000000, 0.03759765625000000000, 0.03808593750000000000, 0.03857421875000000000, 0.03906250000000000000, 0.03955078125000000000, 0.04003906250000000000, 0.04052734375000000000, 0.04101562500000000000, 0.04150390625000000000, 0.04199218750000000000, 0.04248046875000000000, 0.04296875000000000000, 0.04345703125000000000, 0.04394531250000000000, 0.04443359375000000000, 0.04492187500000000000, 0.04541015625000000000, 0.04589843750000000000, 0.04638671875000000000, 0.04687500000000000000, 0.04736328125000000694, 0.04785156250000000694, 0.04833984375000000694, 0.04882812500000000694, 0.04931640625000000694, 0.04980468750000000694, 0.05029296875000000694, 0.05078125000000000694, 0.05126953125000000694, 0.05175781250000000694, 0.05224609375000000694, 0.05273437500000000694, 0.05322265625000000694, 0.05371093750000000694, 0.05419921875000000694, 0.05468750000000000694, 0.05517578125000000694, 0.05566406250000000694, 0.05615234375000000694, 0.05664062500000000694, 0.05712890625000000694, 0.05761718750000000694, 0.05810546875000000694, 0.05859375000000000694, 0.05908203125000000694, 0.05957031250000000694, 0.06005859375000000694, 0.06054687500000000694, 0.06103515625000000694, 0.06152343750000000694, 0.06201171875000000694, 0.06250000000000000000, 0.06298828125000000000, 0.06347656250000000000, 0.06396484375000000000, 0.06445312500000000000, 0.06494140625000000000, 0.06542968750000000000, 0.06591796875000000000, 0.06640625000000000000, 0.06689453125000000000, 0.06738281250000000000, 0.06787109375000000000, 0.06835937500000000000, 0.06884765625000000000, 0.06933593750000000000, 0.06982421875000000000, 0.07031250000000000000, 0.07080078125000000000, 0.07128906250000000000, 0.07177734375000000000, 0.07226562500000000000, 0.07275390625000000000, 0.07324218750000000000, 0.07373046875000000000, 0.07421875000000000000, 0.07470703125000000000, 0.07519531250000000000, 0.07568359375000000000, 0.07617187500000000000, 0.07666015625000000000, 0.07714843750000000000, 0.07763671875000000000, 0.07812500000000000000, 0.07861328125000000000, 0.07910156250000000000, 0.07958984375000000000, 0.08007812500000000000, 0.08056640625000000000, 0.08105468750000000000, 0.08154296875000000000, 0.08203125000000000000, 0.08251953125000000000, 0.08300781250000000000, 0.08349609375000000000, 0.08398437500000000000, 0.08447265625000000000, 0.08496093750000000000, 0.08544921875000000000, 0.08593750000000000000, 0.08642578125000000000, 0.08691406250000000000, 0.08740234375000000000, 0.08789062500000000000, 0.08837890625000000000, 0.08886718750000000000, 0.08935546875000000000, 0.08984375000000000000, 0.09033203125000000000, 0.09082031250000000000, 0.09130859375000000000, 0.09179687500000000000, 0.09228515625000000000, 0.09277343750000000000, 0.09326171875000000000, 0.09375000000000000000, 0.09423828125000001388, 0.09472656250000001388, 0.09521484375000001388, 0.09570312500000001388, 0.09619140625000001388, 0.09667968750000001388, 0.09716796875000001388, 0.09765625000000001388, 0.09814453125000001388, 0.09863281250000001388, 0.09912109375000001388, 0.09960937500000001388, 0.1000976562500000139, 0.1005859375000000139, 0.1010742187500000139, 0.1015625000000000139, 0.1020507812500000139, 0.1025390625000000139, 0.1030273437500000139, 0.1035156250000000139, 0.1040039062500000139, 0.1044921875000000139, 0.1049804687500000139, 0.1054687500000000139, 0.1059570312500000139, 0.1064453125000000139, 0.1069335937500000139, 0.1074218750000000139, 0.1079101562500000139, 0.1083984375000000139, 0.1088867187500000139, 0.1093750000000000139, 0.1098632812500000139, 0.1103515625000000139, 0.1108398437500000139, 0.1113281250000000139, 0.1118164062500000139, 0.1123046875000000139, 0.1127929687500000139, 0.1132812500000000139, 0.1137695312500000139, 0.1142578125000000139, 0.1147460937500000139, 0.1152343750000000139, 0.1157226562500000139, 0.1162109375000000139, 0.1166992187500000139, 0.1171875000000000139, 0.1176757812500000139, 0.1181640625000000139, 0.1186523437500000139, 0.1191406250000000139, 0.1196289062500000139, 0.1201171875000000139, 0.1206054687500000139, 0.1210937500000000139, 0.1215820312500000139, 0.1220703125000000139, 0.1225585937500000139, 0.1230468750000000139, 0.1235351562500000139, 0.1240234375000000139, 0.1245117187500000139, 0.1250000000000000000, 0.1254882812500000000, 0.1259765625000000000, 0.1264648437500000000, 0.1269531250000000000, 0.1274414062500000000, 0.1279296875000000000, 0.1284179687500000000, 0.1289062500000000000, 0.1293945312500000000, 0.1298828125000000000, 0.1303710937500000000, 0.1308593750000000000, 0.1313476562500000000, 0.1318359375000000000, 0.1323242187500000000, 0.1328125000000000000, 0.1333007812500000000, 0.1337890625000000000, 0.1342773437500000000, 0.1347656250000000000, 0.1352539062500000000, 0.1357421875000000000, 0.1362304687500000000, 0.1367187500000000000, 0.1372070312500000000, 0.1376953125000000000, 0.1381835937500000000, 0.1386718750000000000, 0.1391601562500000000, 0.1396484375000000000, 0.1401367187500000000, 0.1406250000000000000, 0.1411132812500000000, 0.1416015625000000000, 0.1420898437500000000, 0.1425781250000000000, 0.1430664062500000000, 0.1435546875000000000, 0.1440429687500000000, 0.1445312500000000000, 0.1450195312500000000, 0.1455078125000000000, 0.1459960937500000000, 0.1464843750000000000, 0.1469726562500000000, 0.1474609375000000000, 0.1479492187500000000, 0.1484375000000000000, 0.1489257812500000000, 0.1494140625000000000, 0.1499023437500000000, 0.1503906250000000000, 0.1508789062500000000, 0.1513671875000000000, 0.1518554687500000000, 0.1523437500000000000, 0.1528320312500000000, 0.1533203125000000000, 0.1538085937500000000, 0.1542968750000000000, 0.1547851562500000000, 0.1552734375000000000, 0.1557617187500000000, 0.1562500000000000000, 0.1567382812500000000, 0.1572265625000000000, 0.1577148437500000000, 0.1582031250000000000, 0.1586914062500000000, 0.1591796875000000000, 0.1596679687500000000, 0.1601562500000000000, 0.1606445312500000000, 0.1611328125000000000, 0.1616210937500000000, 0.1621093750000000000, 0.1625976562500000000, 0.1630859375000000000, 0.1635742187500000000, 0.1640625000000000000, 0.1645507812500000000, 0.1650390625000000000, 0.1655273437500000000, 0.1660156250000000000, 0.1665039062500000000, 0.1669921875000000000, 0.1674804687500000000, 0.1679687500000000000, 0.1684570312500000000, 0.1689453125000000000, 0.1694335937500000000, 0.1699218750000000000, 0.1704101562500000000, 0.1708984375000000000, 0.1713867187500000000, 0.1718750000000000000, 0.1723632812500000000, 0.1728515625000000000, 0.1733398437500000000, 0.1738281250000000000, 0.1743164062500000000, 0.1748046875000000000, 0.1752929687500000000, 0.1757812500000000000, 0.1762695312500000000, 0.1767578125000000000, 0.1772460937500000000, 0.1777343750000000000, 0.1782226562500000000, 0.1787109375000000000, 0.1791992187500000000, 0.1796875000000000000, 0.1801757812500000000, 0.1806640625000000000, 0.1811523437500000000, 0.1816406250000000000, 0.1821289062500000000, 0.1826171875000000000, 0.1831054687500000000, 0.1835937500000000000, 0.1840820312500000000, 0.1845703125000000000, 0.1850585937500000000, 0.1855468750000000000, 0.1860351562500000000, 0.1865234375000000000, 0.1870117187500000000, 0.1875000000000000000, 0.1879882812500000278, 0.1884765625000000278, 0.1889648437500000278, 0.1894531250000000278, 0.1899414062500000278, 0.1904296875000000278, 0.1909179687500000278, 0.1914062500000000278, 0.1918945312500000278, 0.1923828125000000278, 0.1928710937500000278, 0.1933593750000000278, 0.1938476562500000278, 0.1943359375000000278, 0.1948242187500000278, 0.1953125000000000278, 0.1958007812500000278, 0.1962890625000000278, 0.1967773437500000278, 0.1972656250000000278, 0.1977539062500000278, 0.1982421875000000278, 0.1987304687500000278, 0.1992187500000000278, 0.1997070312500000278, 0.2001953125000000278, 0.2006835937500000278, 0.2011718750000000278, 0.2016601562500000278, 0.2021484375000000278, 0.2026367187500000278, 0.2031250000000000278, 0.2036132812500000278, 0.2041015625000000278, 0.2045898437500000278, 0.2050781250000000278, 0.2055664062500000278, 0.2060546875000000278, 0.2065429687500000278, 0.2070312500000000278, 0.2075195312500000278, 0.2080078125000000278, 0.2084960937500000278, 0.2089843750000000278, 0.2094726562500000278, 0.2099609375000000278, 0.2104492187500000278, 0.2109375000000000278, 0.2114257812500000278, 0.2119140625000000278, 0.2124023437500000278, 0.2128906250000000278, 0.2133789062500000278, 0.2138671875000000278, 0.2143554687500000278, 0.2148437500000000278, 0.2153320312500000278, 0.2158203125000000278, 0.2163085937500000278, 0.2167968750000000278, 0.2172851562500000278, 0.2177734375000000278, 0.2182617187500000278, 0.2187500000000000278, 0.2192382812500000278, 0.2197265625000000278, 0.2202148437500000278, 0.2207031250000000278, 0.2211914062500000278, 0.2216796875000000278, 0.2221679687500000278, 0.2226562500000000278, 0.2231445312500000278, 0.2236328125000000278, 0.2241210937500000278, 0.2246093750000000278, 0.2250976562500000278, 0.2255859375000000278, 0.2260742187500000278, 0.2265625000000000278, 0.2270507812500000278, 0.2275390625000000278, 0.2280273437500000278, 0.2285156250000000278, 0.2290039062500000278, 0.2294921875000000278, 0.2299804687500000278, 0.2304687500000000278, 0.2309570312500000278, 0.2314453125000000278, 0.2319335937500000278, 0.2324218750000000278, 0.2329101562500000278, 0.2333984375000000278, 0.2338867187500000278, 0.2343750000000000278, 0.2348632812500000278, 0.2353515625000000278, 0.2358398437500000278, 0.2363281250000000278, 0.2368164062500000278, 0.2373046875000000278, 0.2377929687500000278, 0.2382812500000000278, 0.2387695312500000278, 0.2392578125000000278, 0.2397460937500000278, 0.2402343750000000278, 0.2407226562500000278, 0.2412109375000000278, 0.2416992187500000278, 0.2421875000000000278, 0.2426757812500000278, 0.2431640625000000278, 0.2436523437500000278, 0.2441406250000000278, 0.2446289062500000278, 0.2451171875000000278, 0.2456054687500000278, 0.2460937500000000278, 0.2465820312500000278, 0.2470703125000000278, 0.2475585937500000278, 0.2480468750000000278, 0.2485351562500000278, 0.2490234375000000278, 0.2495117187500000278, 0.2500000000000000000, 0.2504882812500000000, 0.2509765625000000000, 0.2514648437500000000, 0.2519531250000000000, 0.2524414062500000000, 0.2529296875000000000, 0.2534179687500000000, 0.2539062500000000000, 0.2543945312500000000, 0.2548828125000000000, 0.2553710937500000000, 0.2558593750000000000, 0.2563476562500000000, 0.2568359375000000000, 0.2573242187500000000, 0.2578125000000000000, 0.2583007812500000000, 0.2587890625000000000, 0.2592773437500000000, 0.2597656250000000000, 0.2602539062500000000, 0.2607421875000000000, 0.2612304687500000000, 0.2617187500000000000, 0.2622070312500000000, 0.2626953125000000000, 0.2631835937500000000, 0.2636718750000000000, 0.2641601562500000000, 0.2646484375000000000, 0.2651367187500000000, 0.2656250000000000000, 0.2661132812500000000, 0.2666015625000000000, 0.2670898437500000000, 0.2675781250000000000, 0.2680664062500000000, 0.2685546875000000000, 0.2690429687500000000, 0.2695312500000000000, 0.2700195312500000000, 0.2705078125000000000, 0.2709960937500000000, 0.2714843750000000000, 0.2719726562500000000, 0.2724609375000000000, 0.2729492187500000000, 0.2734375000000000000, 0.2739257812500000000, 0.2744140625000000000, 0.2749023437500000000, 0.2753906250000000000, 0.2758789062500000000, 0.2763671875000000000, 0.2768554687500000000, 0.2773437500000000000, 0.2778320312500000000, 0.2783203125000000000, 0.2788085937500000000, 0.2792968750000000000, 0.2797851562500000000, 0.2802734375000000000, 0.2807617187500000000, 0.2812500000000000000, 0.2817382812500000000, 0.2822265625000000000, 0.2827148437500000000, 0.2832031250000000000, 0.2836914062500000000, 0.2841796875000000000, 0.2846679687500000000, 0.2851562500000000000, 0.2856445312500000000, 0.2861328125000000000, 0.2866210937500000000, 0.2871093750000000000, 0.2875976562500000000, 0.2880859375000000000, 0.2885742187500000000, 0.2890625000000000000, 0.2895507812500000000, 0.2900390625000000000, 0.2905273437500000000, 0.2910156250000000000, 0.2915039062500000000, 0.2919921875000000000, 0.2924804687500000000, 0.2929687500000000000, 0.2934570312500000000, 0.2939453125000000000, 0.2944335937500000000, 0.2949218750000000000, 0.2954101562500000000, 0.2958984375000000000, 0.2963867187500000000, 0.2968750000000000000, 0.2973632812500000000, 0.2978515625000000000, 0.2983398437500000000, 0.2988281250000000000, 0.2993164062500000000, 0.2998046875000000000, 0.3002929687500000000, 0.3007812500000000000, 0.3012695312500000000, 0.3017578125000000000, 0.3022460937500000000, 0.3027343750000000000, 0.3032226562500000000, 0.3037109375000000000, 0.3041992187500000000, 0.3046875000000000000, 0.3051757812500000000, 0.3056640625000000000, 0.3061523437500000000, 0.3066406250000000000, 0.3071289062500000000, 0.3076171875000000000, 0.3081054687500000000, 0.3085937500000000000, 0.3090820312500000000, 0.3095703125000000000, 0.3100585937500000000, 0.3105468750000000000, 0.3110351562500000000, 0.3115234375000000000, 0.3120117187500000000, 0.3125000000000000000, 0.3129882812500000000, 0.3134765625000000000, 0.3139648437500000000, 0.3144531250000000000, 0.3149414062500000000, 0.3154296875000000000, 0.3159179687500000000, 0.3164062500000000000, 0.3168945312500000000, 0.3173828125000000000, 0.3178710937500000000, 0.3183593750000000000, 0.3188476562500000000, 0.3193359375000000000, 0.3198242187500000000, 0.3203125000000000000, 0.3208007812500000000, 0.3212890625000000000, 0.3217773437500000000, 0.3222656250000000000, 0.3227539062500000000, 0.3232421875000000000, 0.3237304687500000000, 0.3242187500000000000, 0.3247070312500000000, 0.3251953125000000000, 0.3256835937500000000, 0.3261718750000000000, 0.3266601562500000000, 0.3271484375000000000, 0.3276367187500000000, 0.3281250000000000000, 0.3286132812500000000, 0.3291015625000000000, 0.3295898437500000000, 0.3300781250000000000, 0.3305664062500000000, 0.3310546875000000000, 0.3315429687500000000, 0.3320312500000000000, 0.3325195312500000000, 0.3330078125000000000, 0.3334960937500000000, 0.3339843750000000000, 0.3344726562500000000, 0.3349609375000000000, 0.3354492187500000000, 0.3359375000000000000, 0.3364257812500000000, 0.3369140625000000000, 0.3374023437500000000, 0.3378906250000000000, 0.3383789062500000000, 0.3388671875000000000, 0.3393554687500000000, 0.3398437500000000000, 0.3403320312500000000, 0.3408203125000000000, 0.3413085937500000000, 0.3417968750000000000, 0.3422851562500000000, 0.3427734375000000000, 0.3432617187500000000, 0.3437500000000000000, 0.3442382812500000000, 0.3447265625000000000, 0.3452148437500000000, 0.3457031250000000000, 0.3461914062500000000, 0.3466796875000000000, 0.3471679687500000000, 0.3476562500000000000, 0.3481445312500000000, 0.3486328125000000000, 0.3491210937500000000, 0.3496093750000000000, 0.3500976562500000000, 0.3505859375000000000, 0.3510742187500000000, 0.3515625000000000000, 0.3520507812500000000, 0.3525390625000000000, 0.3530273437500000000, 0.3535156250000000000, 0.3540039062500000000, 0.3544921875000000000, 0.3549804687500000000, 0.3554687500000000000, 0.3559570312500000000, 0.3564453125000000000, 0.3569335937500000000, 0.3574218750000000000, 0.3579101562500000000, 0.3583984375000000000, 0.3588867187500000000, 0.3593750000000000000, 0.3598632812500000000, 0.3603515625000000000, 0.3608398437500000000, 0.3613281250000000000, 0.3618164062500000000, 0.3623046875000000000, 0.3627929687500000000, 0.3632812500000000000, 0.3637695312500000000, 0.3642578125000000000, 0.3647460937500000000, 0.3652343750000000000, 0.3657226562500000000, 0.3662109375000000000, 0.3666992187500000000, 0.3671875000000000000, 0.3676757812500000000, 0.3681640625000000000, 0.3686523437500000000, 0.3691406250000000000, 0.3696289062500000000, 0.3701171875000000000, 0.3706054687500000000, 0.3710937500000000000, 0.3715820312500000000, 0.3720703125000000000, 0.3725585937500000000, 0.3730468750000000000, 0.3735351562500000000, 0.3740234375000000000, 0.3745117187500000000, 0.3750000000000000000, 0.3754882812500000555, 0.3759765625000000555, 0.3764648437500000555, 0.3769531250000000555, 0.3774414062500000555, 0.3779296875000000555, 0.3784179687500000555, 0.3789062500000000555, 0.3793945312500000555, 0.3798828125000000555, 0.3803710937500000555, 0.3808593750000000555, 0.3813476562500000555, 0.3818359375000000555, 0.3823242187500000555, 0.3828125000000000555, 0.3833007812500000555, 0.3837890625000000555, 0.3842773437500000555, 0.3847656250000000555, 0.3852539062500000555, 0.3857421875000000555, 0.3862304687500000555, 0.3867187500000000555, 0.3872070312500000555, 0.3876953125000000555, 0.3881835937500000555, 0.3886718750000000555, 0.3891601562500000555, 0.3896484375000000555, 0.3901367187500000555, 0.3906250000000000555, 0.3911132812500000555, 0.3916015625000000555, 0.3920898437500000555, 0.3925781250000000555, 0.3930664062500000555, 0.3935546875000000555, 0.3940429687500000555, 0.3945312500000000555, 0.3950195312500000555, 0.3955078125000000555, 0.3959960937500000555, 0.3964843750000000555, 0.3969726562500000555, 0.3974609375000000555, 0.3979492187500000555, 0.3984375000000000555, 0.3989257812500000555, 0.3994140625000000555, 0.3999023437500000555, 0.4003906250000000555, 0.4008789062500000555, 0.4013671875000000555, 0.4018554687500000555, 0.4023437500000000555, 0.4028320312500000555, 0.4033203125000000555, 0.4038085937500000555, 0.4042968750000000555, 0.4047851562500000555, 0.4052734375000000555, 0.4057617187500000555, 0.4062500000000000555, 0.4067382812500000555, 0.4072265625000000555, 0.4077148437500000555, 0.4082031250000000555, 0.4086914062500000555, 0.4091796875000000555, 0.4096679687500000555, 0.4101562500000000555, 0.4106445312500000555, 0.4111328125000000555, 0.4116210937500000555, 0.4121093750000000555, 0.4125976562500000555, 0.4130859375000000555, 0.4135742187500000555, 0.4140625000000000555, 0.4145507812500000555, 0.4150390625000000555, 0.4155273437500000555, 0.4160156250000000555, 0.4165039062500000555, 0.4169921875000000555, 0.4174804687500000555, 0.4179687500000000555, 0.4184570312500000555, 0.4189453125000000555, 0.4194335937500000555, 0.4199218750000000555, 0.4204101562500000555, 0.4208984375000000555, 0.4213867187500000555, 0.4218750000000000555, 0.4223632812500000555, 0.4228515625000000555, 0.4233398437500000555, 0.4238281250000000555, 0.4243164062500000555, 0.4248046875000000555, 0.4252929687500000555, 0.4257812500000000555, 0.4262695312500000555, 0.4267578125000000555, 0.4272460937500000555, 0.4277343750000000555, 0.4282226562500000555, 0.4287109375000000555, 0.4291992187500000555, 0.4296875000000000555, 0.4301757812500000555, 0.4306640625000000555, 0.4311523437500000555, 0.4316406250000000555, 0.4321289062500000555, 0.4326171875000000555, 0.4331054687500000555, 0.4335937500000000555, 0.4340820312500000555, 0.4345703125000000555, 0.4350585937500000555, 0.4355468750000000555, 0.4360351562500000555, 0.4365234375000000555, 0.4370117187500000555, 0.4375000000000000555, 0.4379882812500000555, 0.4384765625000000555, 0.4389648437500000555, 0.4394531250000000555, 0.4399414062500000555, 0.4404296875000000555, 0.4409179687500000555, 0.4414062500000000555, 0.4418945312500000555, 0.4423828125000000555, 0.4428710937500000555, 0.4433593750000000555, 0.4438476562500000555, 0.4443359375000000555, 0.4448242187500000555, 0.4453125000000000555, 0.4458007812500000555, 0.4462890625000000555, 0.4467773437500000555, 0.4472656250000000555, 0.4477539062500000555, 0.4482421875000000555, 0.4487304687500000555, 0.4492187500000000555, 0.4497070312500000555, 0.4501953125000000555, 0.4506835937500000555, 0.4511718750000000555, 0.4516601562500000555, 0.4521484375000000555, 0.4526367187500000555, 0.4531250000000000555, 0.4536132812500000555, 0.4541015625000000555, 0.4545898437500000555, 0.4550781250000000555, 0.4555664062500000555, 0.4560546875000000555, 0.4565429687500000555, 0.4570312500000000555, 0.4575195312500000555, 0.4580078125000000555, 0.4584960937500000555, 0.4589843750000000555, 0.4594726562500000555, 0.4599609375000000555, 0.4604492187500000555, 0.4609375000000000555, 0.4614257812500000555, 0.4619140625000000555, 0.4624023437500000555, 0.4628906250000000555, 0.4633789062500000555, 0.4638671875000000555, 0.4643554687500000555, 0.4648437500000000555, 0.4653320312500000555, 0.4658203125000000555, 0.4663085937500000555, 0.4667968750000000555, 0.4672851562500000555, 0.4677734375000000555, 0.4682617187500000555, 0.4687500000000000555, 0.4692382812500000555, 0.4697265625000000555, 0.4702148437500000555, 0.4707031250000000555, 0.4711914062500000555, 0.4716796875000000555, 0.4721679687500000555, 0.4726562500000000555, 0.4731445312500000555, 0.4736328125000000555, 0.4741210937500000555, 0.4746093750000000555, 0.4750976562500000555, 0.4755859375000000555, 0.4760742187500000555, 0.4765625000000000555, 0.4770507812500000555, 0.4775390625000000555, 0.4780273437500000555, 0.4785156250000000555, 0.4790039062500000555, 0.4794921875000000555, 0.4799804687500000555, 0.4804687500000000555, 0.4809570312500000555, 0.4814453125000000555, 0.4819335937500000555, 0.4824218750000000555, 0.4829101562500000555, 0.4833984375000000555, 0.4838867187500000555, 0.4843750000000000555, 0.4848632812500000555, 0.4853515625000000555, 0.4858398437500000555, 0.4863281250000000555, 0.4868164062500000555, 0.4873046875000000555, 0.4877929687500000555, 0.4882812500000000555, 0.4887695312500000555, 0.4892578125000000555, 0.4897460937500000555, 0.4902343750000000555, 0.4907226562500000555, 0.4912109375000000555, 0.4916992187500000555, 0.4921875000000000555, 0.4926757812500000555, 0.4931640625000000555, 0.4936523437500000555, 0.4941406250000000555, 0.4946289062500000555, 0.4951171875000000555, 0.4956054687500000555, 0.4960937500000000555, 0.4965820312500000555, 0.4970703125000000555, 0.4975585937500000555, 0.4980468750000000555, 0.4985351562500000555, 0.4990234375000000555, 0.4995117187500000555, 0.5000000000000000000, 0.5004882812500000000, 0.5009765625000000000, 0.5014648437500000000, 0.5019531250000000000, 0.5024414062500000000, 0.5029296875000000000, 0.5034179687500000000, 0.5039062500000000000, 0.5043945312500000000, 0.5048828125000000000, 0.5053710937500000000, 0.5058593750000000000, 0.5063476562500000000, 0.5068359375000000000, 0.5073242187500000000, 0.5078125000000000000, 0.5083007812500000000, 0.5087890625000000000, 0.5092773437500000000, 0.5097656250000000000, 0.5102539062500000000, 0.5107421875000000000, 0.5112304687500000000, 0.5117187500000000000, 0.5122070312500000000, 0.5126953125000000000, 0.5131835937500000000, 0.5136718750000000000, 0.5141601562500000000, 0.5146484375000000000, 0.5151367187500000000, 0.5156250000000000000, 0.5161132812500000000, 0.5166015625000000000, 0.5170898437500000000, 0.5175781250000000000, 0.5180664062500000000, 0.5185546875000000000, 0.5190429687500000000, 0.5195312500000000000, 0.5200195312500000000, 0.5205078125000000000, 0.5209960937500000000, 0.5214843750000000000, 0.5219726562500000000, 0.5224609375000000000, 0.5229492187500000000, 0.5234375000000000000, 0.5239257812500000000, 0.5244140625000000000, 0.5249023437500000000, 0.5253906250000000000, 0.5258789062500000000, 0.5263671875000000000, 0.5268554687500000000, 0.5273437500000000000, 0.5278320312500000000, 0.5283203125000000000, 0.5288085937500000000, 0.5292968750000000000, 0.5297851562500000000, 0.5302734375000000000, 0.5307617187500000000, 0.5312500000000000000, 0.5317382812500000000, 0.5322265625000000000, 0.5327148437500000000, 0.5332031250000000000, 0.5336914062500000000, 0.5341796875000000000, 0.5346679687500000000, 0.5351562500000000000, 0.5356445312500000000, 0.5361328125000000000, 0.5366210937500000000, 0.5371093750000000000, 0.5375976562500000000, 0.5380859375000000000, 0.5385742187500000000, 0.5390625000000000000, 0.5395507812500000000, 0.5400390625000000000, 0.5405273437500000000, 0.5410156250000000000, 0.5415039062500000000, 0.5419921875000000000, 0.5424804687500000000, 0.5429687500000000000, 0.5434570312500000000, 0.5439453125000000000, 0.5444335937500000000, 0.5449218750000000000, 0.5454101562500000000, 0.5458984375000000000, 0.5463867187500000000, 0.5468750000000000000, 0.5473632812500000000, 0.5478515625000000000, 0.5483398437500000000, 0.5488281250000000000, 0.5493164062500000000, 0.5498046875000000000, 0.5502929687500000000, 0.5507812500000000000, 0.5512695312500000000, 0.5517578125000000000, 0.5522460937500000000, 0.5527343750000000000, 0.5532226562500000000, 0.5537109375000000000, 0.5541992187500000000, 0.5546875000000000000, 0.5551757812500000000, 0.5556640625000000000, 0.5561523437500000000, 0.5566406250000000000, 0.5571289062500000000, 0.5576171875000000000, 0.5581054687500000000, 0.5585937500000000000, 0.5590820312500000000, 0.5595703125000000000, 0.5600585937500000000, 0.5605468750000000000, 0.5610351562500000000, 0.5615234375000000000, 0.5620117187500000000, 0.5625000000000000000, 0.5629882812500000000, 0.5634765625000000000, 0.5639648437500000000, 0.5644531250000000000, 0.5649414062500000000, 0.5654296875000000000, 0.5659179687500000000, 0.5664062500000000000, 0.5668945312500000000, 0.5673828125000000000, 0.5678710937500000000, 0.5683593750000000000, 0.5688476562500000000, 0.5693359375000000000, 0.5698242187500000000, 0.5703125000000000000, 0.5708007812500000000, 0.5712890625000000000, 0.5717773437500000000, 0.5722656250000000000, 0.5727539062500000000, 0.5732421875000000000, 0.5737304687500000000, 0.5742187500000000000, 0.5747070312500000000, 0.5751953125000000000, 0.5756835937500000000, 0.5761718750000000000, 0.5766601562500000000, 0.5771484375000000000, 0.5776367187500000000, 0.5781250000000000000, 0.5786132812500000000, 0.5791015625000000000, 0.5795898437500000000, 0.5800781250000000000, 0.5805664062500000000, 0.5810546875000000000, 0.5815429687500000000, 0.5820312500000000000, 0.5825195312500000000, 0.5830078125000000000, 0.5834960937500000000, 0.5839843750000000000, 0.5844726562500000000, 0.5849609375000000000, 0.5854492187500000000, 0.5859375000000000000, 0.5864257812500000000, 0.5869140625000000000, 0.5874023437500000000, 0.5878906250000000000, 0.5883789062500000000, 0.5888671875000000000, 0.5893554687500000000, 0.5898437500000000000, 0.5903320312500000000, 0.5908203125000000000, 0.5913085937500000000, 0.5917968750000000000, 0.5922851562500000000, 0.5927734375000000000, 0.5932617187500000000, 0.5937500000000000000, 0.5942382812500000000, 0.5947265625000000000, 0.5952148437500000000, 0.5957031250000000000, 0.5961914062500000000, 0.5966796875000000000, 0.5971679687500000000, 0.5976562500000000000, 0.5981445312500000000, 0.5986328125000000000, 0.5991210937500000000, 0.5996093750000000000, 0.6000976562500000000, 0.6005859375000000000, 0.6010742187500000000, 0.6015625000000000000, 0.6020507812500000000, 0.6025390625000000000, 0.6030273437500000000, 0.6035156250000000000, 0.6040039062500000000, 0.6044921875000000000, 0.6049804687500000000, 0.6054687500000000000, 0.6059570312500000000, 0.6064453125000000000, 0.6069335937500000000, 0.6074218750000000000, 0.6079101562500000000, 0.6083984375000000000, 0.6088867187500000000, 0.6093750000000000000, 0.6098632812500000000, 0.6103515625000000000, 0.6108398437500000000, 0.6113281250000000000, 0.6118164062500000000, 0.6123046875000000000, 0.6127929687500000000, 0.6132812500000000000, 0.6137695312500000000, 0.6142578125000000000, 0.6147460937500000000, 0.6152343750000000000, 0.6157226562500000000, 0.6162109375000000000, 0.6166992187500000000, 0.6171875000000000000, 0.6176757812500000000, 0.6181640625000000000, 0.6186523437500000000, 0.6191406250000000000, 0.6196289062500000000, 0.6201171875000000000, 0.6206054687500000000, 0.6210937500000000000, 0.6215820312500000000, 0.6220703125000000000, 0.6225585937500000000, 0.6230468750000000000, 0.6235351562500000000, 0.6240234375000000000, 0.6245117187500000000, 0.6250000000000000000, 0.6254882812500000000, 0.6259765625000000000, 0.6264648437500000000, 0.6269531250000000000, 0.6274414062500000000, 0.6279296875000000000, 0.6284179687500000000, 0.6289062500000000000, 0.6293945312500000000, 0.6298828125000000000, 0.6303710937500000000, 0.6308593750000000000, 0.6313476562500000000, 0.6318359375000000000, 0.6323242187500000000, 0.6328125000000000000, 0.6333007812500000000, 0.6337890625000000000, 0.6342773437500000000, 0.6347656250000000000, 0.6352539062500000000, 0.6357421875000000000, 0.6362304687500000000, 0.6367187500000000000, 0.6372070312500000000, 0.6376953125000000000, 0.6381835937500000000, 0.6386718750000000000, 0.6391601562500000000, 0.6396484375000000000, 0.6401367187500000000, 0.6406250000000000000, 0.6411132812500000000, 0.6416015625000000000, 0.6420898437500000000, 0.6425781250000000000, 0.6430664062500000000, 0.6435546875000000000, 0.6440429687500000000, 0.6445312500000000000, 0.6450195312500000000, 0.6455078125000000000, 0.6459960937500000000, 0.6464843750000000000, 0.6469726562500000000, 0.6474609375000000000, 0.6479492187500000000, 0.6484375000000000000, 0.6489257812500000000, 0.6494140625000000000, 0.6499023437500000000, 0.6503906250000000000, 0.6508789062500000000, 0.6513671875000000000, 0.6518554687500000000, 0.6523437500000000000, 0.6528320312500000000, 0.6533203125000000000, 0.6538085937500000000, 0.6542968750000000000, 0.6547851562500000000, 0.6552734375000000000, 0.6557617187500000000, 0.6562500000000000000, 0.6567382812500000000, 0.6572265625000000000, 0.6577148437500000000, 0.6582031250000000000, 0.6586914062500000000, 0.6591796875000000000, 0.6596679687500000000, 0.6601562500000000000, 0.6606445312500000000, 0.6611328125000000000, 0.6616210937500000000, 0.6621093750000000000, 0.6625976562500000000, 0.6630859375000000000, 0.6635742187500000000, 0.6640625000000000000, 0.6645507812500000000, 0.6650390625000000000, 0.6655273437500000000, 0.6660156250000000000, 0.6665039062500000000, 0.6669921875000000000, 0.6674804687500000000, 0.6679687500000000000, 0.6684570312500000000, 0.6689453125000000000, 0.6694335937500000000, 0.6699218750000000000, 0.6704101562500000000, 0.6708984375000000000, 0.6713867187500000000, 0.6718750000000000000, 0.6723632812500000000, 0.6728515625000000000, 0.6733398437500000000, 0.6738281250000000000, 0.6743164062500000000, 0.6748046875000000000, 0.6752929687500000000, 0.6757812500000000000, 0.6762695312500000000, 0.6767578125000000000, 0.6772460937500000000, 0.6777343750000000000, 0.6782226562500000000, 0.6787109375000000000, 0.6791992187500000000, 0.6796875000000000000, 0.6801757812500000000, 0.6806640625000000000, 0.6811523437500000000, 0.6816406250000000000, 0.6821289062500000000, 0.6826171875000000000, 0.6831054687500000000, 0.6835937500000000000, 0.6840820312500000000, 0.6845703125000000000, 0.6850585937500000000, 0.6855468750000000000, 0.6860351562500000000, 0.6865234375000000000, 0.6870117187500000000, 0.6875000000000000000, 0.6879882812500000000, 0.6884765625000000000, 0.6889648437500000000, 0.6894531250000000000, 0.6899414062500000000, 0.6904296875000000000, 0.6909179687500000000, 0.6914062500000000000, 0.6918945312500000000, 0.6923828125000000000, 0.6928710937500000000, 0.6933593750000000000, 0.6938476562500000000, 0.6943359375000000000, 0.6948242187500000000, 0.6953125000000000000, 0.6958007812500000000, 0.6962890625000000000, 0.6967773437500000000, 0.6972656250000000000, 0.6977539062500000000, 0.6982421875000000000, 0.6987304687500000000, 0.6992187500000000000, 0.6997070312500000000, 0.7001953125000000000, 0.7006835937500000000, 0.7011718750000000000, 0.7016601562500000000, 0.7021484375000000000, 0.7026367187500000000, 0.7031250000000000000, 0.7036132812500000000, 0.7041015625000000000, 0.7045898437500000000, 0.7050781250000000000, 0.7055664062500000000, 0.7060546875000000000, 0.7065429687500000000, 0.7070312500000000000, 0.7075195312500000000, 0.7080078125000000000, 0.7084960937500000000, 0.7089843750000000000, 0.7094726562500000000, 0.7099609375000000000, 0.7104492187500000000, 0.7109375000000000000, 0.7114257812500000000, 0.7119140625000000000, 0.7124023437500000000, 0.7128906250000000000, 0.7133789062500000000, 0.7138671875000000000, 0.7143554687500000000, 0.7148437500000000000, 0.7153320312500000000, 0.7158203125000000000, 0.7163085937500000000, 0.7167968750000000000, 0.7172851562500000000, 0.7177734375000000000, 0.7182617187500000000, 0.7187500000000000000, 0.7192382812500000000, 0.7197265625000000000, 0.7202148437500000000, 0.7207031250000000000, 0.7211914062500000000, 0.7216796875000000000, 0.7221679687500000000, 0.7226562500000000000, 0.7231445312500000000, 0.7236328125000000000, 0.7241210937500000000, 0.7246093750000000000, 0.7250976562500000000, 0.7255859375000000000, 0.7260742187500000000, 0.7265625000000000000, 0.7270507812500000000, 0.7275390625000000000, 0.7280273437500000000, 0.7285156250000000000, 0.7290039062500000000, 0.7294921875000000000, 0.7299804687500000000, 0.7304687500000000000, 0.7309570312500000000, 0.7314453125000000000, 0.7319335937500000000, 0.7324218750000000000, 0.7329101562500000000, 0.7333984375000000000, 0.7338867187500000000, 0.7343750000000000000, 0.7348632812500000000, 0.7353515625000000000, 0.7358398437500000000, 0.7363281250000000000, 0.7368164062500000000, 0.7373046875000000000, 0.7377929687500000000, 0.7382812500000000000, 0.7387695312500000000, 0.7392578125000000000, 0.7397460937500000000, 0.7402343750000000000, 0.7407226562500000000, 0.7412109375000000000, 0.7416992187500000000, 0.7421875000000000000, 0.7426757812500000000, 0.7431640625000000000, 0.7436523437500000000, 0.7441406250000000000, 0.7446289062500000000, 0.7451171875000000000, 0.7456054687500000000, 0.7460937500000000000, 0.7465820312500000000, 0.7470703125000000000, 0.7475585937500000000, 0.7480468750000000000, 0.7485351562500000000, 0.7490234375000000000, 0.7495117187500000000, 0.7500000000000000000, 0.7504882812500001110, 0.7509765625000001110, 0.7514648437500001110, 0.7519531250000001110, 0.7524414062500001110, 0.7529296875000001110, 0.7534179687500001110, 0.7539062500000001110, 0.7543945312500001110, 0.7548828125000001110, 0.7553710937500001110, 0.7558593750000001110, 0.7563476562500001110, 0.7568359375000001110, 0.7573242187500001110, 0.7578125000000001110, 0.7583007812500001110, 0.7587890625000001110, 0.7592773437500001110, 0.7597656250000001110, 0.7602539062500001110, 0.7607421875000001110, 0.7612304687500001110, 0.7617187500000001110, 0.7622070312500001110, 0.7626953125000001110, 0.7631835937500001110, 0.7636718750000001110, 0.7641601562500001110, 0.7646484375000001110, 0.7651367187500001110, 0.7656250000000001110, 0.7661132812500001110, 0.7666015625000001110, 0.7670898437500001110, 0.7675781250000001110, 0.7680664062500001110, 0.7685546875000001110, 0.7690429687500001110, 0.7695312500000001110, 0.7700195312500001110, 0.7705078125000001110, 0.7709960937500001110, 0.7714843750000001110, 0.7719726562500001110, 0.7724609375000001110, 0.7729492187500001110, 0.7734375000000001110, 0.7739257812500001110, 0.7744140625000001110, 0.7749023437500001110, 0.7753906250000001110, 0.7758789062500001110, 0.7763671875000001110, 0.7768554687500001110, 0.7773437500000001110, 0.7778320312500001110, 0.7783203125000001110, 0.7788085937500001110, 0.7792968750000001110, 0.7797851562500001110, 0.7802734375000001110, 0.7807617187500001110, 0.7812500000000001110, 0.7817382812500001110, 0.7822265625000001110, 0.7827148437500001110, 0.7832031250000001110, 0.7836914062500001110, 0.7841796875000001110, 0.7846679687500001110, 0.7851562500000001110, 0.7856445312500001110, 0.7861328125000001110, 0.7866210937500001110, 0.7871093750000001110, 0.7875976562500001110, 0.7880859375000001110, 0.7885742187500001110, 0.7890625000000001110, 0.7895507812500001110, 0.7900390625000001110, 0.7905273437500001110, 0.7910156250000001110, 0.7915039062500001110, 0.7919921875000001110, 0.7924804687500001110, 0.7929687500000001110, 0.7934570312500001110, 0.7939453125000001110, 0.7944335937500001110, 0.7949218750000001110, 0.7954101562500001110, 0.7958984375000001110, 0.7963867187500001110, 0.7968750000000001110, 0.7973632812500001110, 0.7978515625000001110, 0.7983398437500001110, 0.7988281250000001110, 0.7993164062500001110, 0.7998046875000001110, 0.8002929687500001110, 0.8007812500000001110, 0.8012695312500001110, 0.8017578125000001110, 0.8022460937500001110, 0.8027343750000001110, 0.8032226562500001110, 0.8037109375000001110, 0.8041992187500001110, 0.8046875000000001110, 0.8051757812500001110, 0.8056640625000001110, 0.8061523437500001110, 0.8066406250000001110, 0.8071289062500001110, 0.8076171875000001110, 0.8081054687500001110, 0.8085937500000001110, 0.8090820312500001110, 0.8095703125000001110, 0.8100585937500001110, 0.8105468750000001110, 0.8110351562500001110, 0.8115234375000001110, 0.8120117187500001110, 0.8125000000000001110, 0.8129882812500001110, 0.8134765625000001110, 0.8139648437500001110, 0.8144531250000001110, 0.8149414062500001110, 0.8154296875000001110, 0.8159179687500001110, 0.8164062500000001110, 0.8168945312500001110, 0.8173828125000001110, 0.8178710937500001110, 0.8183593750000001110, 0.8188476562500001110, 0.8193359375000001110, 0.8198242187500001110, 0.8203125000000001110, 0.8208007812500001110, 0.8212890625000001110, 0.8217773437500001110, 0.8222656250000001110, 0.8227539062500001110, 0.8232421875000001110, 0.8237304687500001110, 0.8242187500000001110, 0.8247070312500001110, 0.8251953125000001110, 0.8256835937500001110, 0.8261718750000001110, 0.8266601562500001110, 0.8271484375000001110, 0.8276367187500001110, 0.8281250000000001110, 0.8286132812500001110, 0.8291015625000001110, 0.8295898437500001110, 0.8300781250000001110, 0.8305664062500001110, 0.8310546875000001110, 0.8315429687500001110, 0.8320312500000001110, 0.8325195312500001110, 0.8330078125000001110, 0.8334960937500001110, 0.8339843750000001110, 0.8344726562500001110, 0.8349609375000001110, 0.8354492187500001110, 0.8359375000000001110, 0.8364257812500001110, 0.8369140625000001110, 0.8374023437500001110, 0.8378906250000001110, 0.8383789062500001110, 0.8388671875000001110, 0.8393554687500001110, 0.8398437500000001110, 0.8403320312500001110, 0.8408203125000001110, 0.8413085937500001110, 0.8417968750000001110, 0.8422851562500001110, 0.8427734375000001110, 0.8432617187500001110, 0.8437500000000001110, 0.8442382812500001110, 0.8447265625000001110, 0.8452148437500001110, 0.8457031250000001110, 0.8461914062500001110, 0.8466796875000001110, 0.8471679687500001110, 0.8476562500000001110, 0.8481445312500001110, 0.8486328125000001110, 0.8491210937500001110, 0.8496093750000001110, 0.8500976562500001110, 0.8505859375000001110, 0.8510742187500001110, 0.8515625000000001110, 0.8520507812500001110, 0.8525390625000001110, 0.8530273437500001110, 0.8535156250000001110, 0.8540039062500001110, 0.8544921875000001110, 0.8549804687500001110, 0.8554687500000001110, 0.8559570312500001110, 0.8564453125000001110, 0.8569335937500001110, 0.8574218750000001110, 0.8579101562500001110, 0.8583984375000001110, 0.8588867187500001110, 0.8593750000000001110, 0.8598632812500001110, 0.8603515625000001110, 0.8608398437500001110, 0.8613281250000001110, 0.8618164062500001110, 0.8623046875000001110, 0.8627929687500001110, 0.8632812500000001110, 0.8637695312500001110, 0.8642578125000001110, 0.8647460937500001110, 0.8652343750000001110, 0.8657226562500001110, 0.8662109375000001110, 0.8666992187500001110, 0.8671875000000001110, 0.8676757812500001110, 0.8681640625000001110, 0.8686523437500001110, 0.8691406250000001110, 0.8696289062500001110, 0.8701171875000001110, 0.8706054687500001110, 0.8710937500000001110, 0.8715820312500001110, 0.8720703125000001110, 0.8725585937500001110, 0.8730468750000001110, 0.8735351562500001110, 0.8740234375000001110, 0.8745117187500001110, 0.8750000000000001110, 0.8754882812500001110, 0.8759765625000001110, 0.8764648437500001110, 0.8769531250000001110, 0.8774414062500001110, 0.8779296875000001110, 0.8784179687500001110, 0.8789062500000001110, 0.8793945312500001110, 0.8798828125000001110, 0.8803710937500001110, 0.8808593750000001110, 0.8813476562500001110, 0.8818359375000001110, 0.8823242187500001110, 0.8828125000000001110, 0.8833007812500001110, 0.8837890625000001110, 0.8842773437500001110, 0.8847656250000001110, 0.8852539062500001110, 0.8857421875000001110, 0.8862304687500001110, 0.8867187500000001110, 0.8872070312500001110, 0.8876953125000001110, 0.8881835937500001110, 0.8886718750000001110, 0.8891601562500001110, 0.8896484375000001110, 0.8901367187500001110, 0.8906250000000001110, 0.8911132812500001110, 0.8916015625000001110, 0.8920898437500001110, 0.8925781250000001110, 0.8930664062500001110, 0.8935546875000001110, 0.8940429687500001110, 0.8945312500000001110, 0.8950195312500001110, 0.8955078125000001110, 0.8959960937500001110, 0.8964843750000001110, 0.8969726562500001110, 0.8974609375000001110, 0.8979492187500001110, 0.8984375000000001110, 0.8989257812500001110, 0.8994140625000001110, 0.8999023437500001110, 0.9003906250000001110, 0.9008789062500001110, 0.9013671875000001110, 0.9018554687500001110, 0.9023437500000001110, 0.9028320312500001110, 0.9033203125000001110, 0.9038085937500001110, 0.9042968750000001110, 0.9047851562500001110, 0.9052734375000001110, 0.9057617187500001110, 0.9062500000000001110, 0.9067382812500001110, 0.9072265625000001110, 0.9077148437500001110, 0.9082031250000001110, 0.9086914062500001110, 0.9091796875000001110, 0.9096679687500001110, 0.9101562500000001110, 0.9106445312500001110, 0.9111328125000001110, 0.9116210937500001110, 0.9121093750000001110, 0.9125976562500001110, 0.9130859375000001110, 0.9135742187500001110, 0.9140625000000001110, 0.9145507812500001110, 0.9150390625000001110, 0.9155273437500001110, 0.9160156250000001110, 0.9165039062500001110, 0.9169921875000001110, 0.9174804687500001110, 0.9179687500000001110, 0.9184570312500001110, 0.9189453125000001110, 0.9194335937500001110, 0.9199218750000001110, 0.9204101562500001110, 0.9208984375000001110, 0.9213867187500001110, 0.9218750000000001110, 0.9223632812500001110, 0.9228515625000001110, 0.9233398437500001110, 0.9238281250000001110, 0.9243164062500001110, 0.9248046875000001110, 0.9252929687500001110, 0.9257812500000001110, 0.9262695312500001110, 0.9267578125000001110, 0.9272460937500001110, 0.9277343750000001110, 0.9282226562500001110, 0.9287109375000001110, 0.9291992187500001110, 0.9296875000000001110, 0.9301757812500001110, 0.9306640625000001110, 0.9311523437500001110, 0.9316406250000001110, 0.9321289062500001110, 0.9326171875000001110, 0.9331054687500001110, 0.9335937500000001110, 0.9340820312500001110, 0.9345703125000001110, 0.9350585937500001110, 0.9355468750000001110, 0.9360351562500001110, 0.9365234375000001110, 0.9370117187500001110, 0.9375000000000001110, 0.9379882812500001110, 0.9384765625000001110, 0.9389648437500001110, 0.9394531250000001110, 0.9399414062500001110, 0.9404296875000001110, 0.9409179687500001110, 0.9414062500000001110, 0.9418945312500001110, 0.9423828125000001110, 0.9428710937500001110, 0.9433593750000001110, 0.9438476562500001110, 0.9443359375000001110, 0.9448242187500001110, 0.9453125000000001110, 0.9458007812500001110, 0.9462890625000001110, 0.9467773437500001110, 0.9472656250000001110, 0.9477539062500001110, 0.9482421875000001110, 0.9487304687500001110, 0.9492187500000001110, 0.9497070312500001110, 0.9501953125000001110, 0.9506835937500001110, 0.9511718750000001110, 0.9516601562500001110, 0.9521484375000001110, 0.9526367187500001110, 0.9531250000000001110, 0.9536132812500001110, 0.9541015625000001110, 0.9545898437500001110, 0.9550781250000001110, 0.9555664062500001110, 0.9560546875000001110, 0.9565429687500001110, 0.9570312500000001110, 0.9575195312500001110, 0.9580078125000001110, 0.9584960937500001110, 0.9589843750000001110, 0.9594726562500001110, 0.9599609375000001110, 0.9604492187500001110, 0.9609375000000001110, 0.9614257812500001110, 0.9619140625000001110, 0.9624023437500001110, 0.9628906250000001110, 0.9633789062500001110, 0.9638671875000001110, 0.9643554687500001110, 0.9648437500000001110, 0.9653320312500001110, 0.9658203125000001110, 0.9663085937500001110, 0.9667968750000001110, 0.9672851562500001110, 0.9677734375000001110, 0.9682617187500001110, 0.9687500000000001110, 0.9692382812500001110, 0.9697265625000001110, 0.9702148437500001110, 0.9707031250000001110, 0.9711914062500001110, 0.9716796875000001110, 0.9721679687500001110, 0.9726562500000001110, 0.9731445312500001110, 0.9736328125000001110, 0.9741210937500001110, 0.9746093750000001110, 0.9750976562500001110, 0.9755859375000001110, 0.9760742187500001110, 0.9765625000000001110, 0.9770507812500001110, 0.9775390625000001110, 0.9780273437500001110, 0.9785156250000001110, 0.9790039062500001110, 0.9794921875000001110, 0.9799804687500001110, 0.9804687500000001110, 0.9809570312500001110, 0.9814453125000001110, 0.9819335937500001110, 0.9824218750000001110, 0.9829101562500001110, 0.9833984375000001110, 0.9838867187500001110, 0.9843750000000001110, 0.9848632812500001110, 0.9853515625000001110, 0.9858398437500001110, 0.9863281250000001110, 0.9868164062500001110, 0.9873046875000001110, 0.9877929687500001110, 0.9882812500000001110, 0.9887695312500001110, 0.9892578125000001110, 0.9897460937500001110, 0.9902343750000001110, 0.9907226562500001110, 0.9912109375000001110, 0.9916992187500001110, 0.9921875000000001110, 0.9926757812500001110, 0.9931640625000001110, 0.9936523437500001110, 0.9941406250000001110, 0.9946289062500001110, 0.9951171875000001110, 0.9956054687500001110, 0.9960937500000001110, 0.9965820312500001110, 0.9970703125000001110, 0.9975585937500001110, 0.9980468750000001110, 0.9985351562500001110, 0.9990234375000001110, 0.9995117187500001110, 1.000000000000000000 ),
 ( 0.000000000000000000, 1.000000000000000000 ),
 .UNSPECIFIED. ) ;
#70299 = ADVANCED_FACE ( 'NONE', ( #82861 ), #89555, .T. ) ;
#70298 = CARTESIAN_POINT ( 'NONE',  ( -58.52287095715006870, -23.72773821059536914, 11.05748984161097326 ) ) ;
#70300 = CARTESIAN_POINT ( 'NONE',  ( -20.02981537788295441, -6.213780249082809348, -1.500000000000002220 ) ) ;
#70301 = ORIENTED_EDGE ( 'NONE', *, *, #30185, .F. ) ;
#70302 = CARTESIAN_POINT ( 'NONE',  ( -2.794871794871795156, -6.376774720514417183, 20.36318108974359475 ) ) ;
#70303 = CARTESIAN_POINT ( 'NONE',  ( 22.81105451610979173, 4.772774720514425972, -18.46691820600746681 ) ) ;
#70304 = CARTESIAN_POINT ( 'NONE',  ( 10.73283225829863952, -3.316774720511335595, -27.03068772560423838 ) ) ;
#70305 = LINE ( 'NONE', #75903, #100383 ) ;
#70306 = CARTESIAN_POINT ( 'NONE',  ( -59.63220076935764524, -24.34968618360933235, 0.1864209137778795600 ) ) ;
#70307 = CARTESIAN_POINT ( 'NONE',  ( -20.77875734969026311, 6.143225279485574397, 27.31649921512899937 ) ) ;
#70309 = VERTEX_POINT ( 'NONE', #21449 ) ;
#70308 = CARTESIAN_POINT ( 'NONE',  ( -22.11311035156252558, 1.696007508605793301, 11.49999999999999645 ) ) ;
#70310 = LINE ( 'NONE', #62710, #77701 ) ;
#70311 = DIRECTION ( 'NONE',  ( -1.000000000000000000, -0.000000000000000000, -0.000000000000000000 ) ) ;
#70312 = VERTEX_POINT ( 'NONE', #75253 ) ;
#70313 = VECTOR ( 'NONE', #38163, 1000.000000000000114 ) ;
#70314 = CARTESIAN_POINT ( 'NONE',  ( -12.01393383709116947, -19.22582291892495121, -1.500000000000002220 ) ) ;
#70316 = ORIENTED_EDGE ( 'NONE', *, *, #43625, .F. ) ;
#70315 = CARTESIAN_POINT ( 'NONE',  ( -28.24880736952684046, -24.86983583622034644, 7.480645431890892816 ) ) ;
#70317 = VECTOR ( 'NONE', #48631, 1000.000000000000114 ) ;
#70318 = ORIENTED_EDGE ( 'NONE', *, *, #63532, .T. ) ;
#70319 = CARTESIAN_POINT ( 'NONE',  ( 30.76755528059973699, 5.112846897994304918, -0.3209731499738198157 ) ) ;
#70320 = CARTESIAN_POINT ( 'NONE',  ( -7.946508460909448956, -18.53024980520100939, 11.49999999999998934 ) ) ;
#70321 = FACE_OUTER_BOUND ( 'NONE', #16994, .T. ) ;
#70322 = ORIENTED_EDGE ( 'NONE', *, *, #12321, .F. ) ;
#70323 = CARTESIAN_POINT ( 'NONE',  ( 12.92500000000000249, 14.49999999999999645, 12.73734666247253244 ) ) ;
#70324 = CARTESIAN_POINT ( 'NONE',  ( 16.55124408090292576, 15.08944307983326638, -1.500000000000002220 ) ) ;
#70325 = ORIENTED_EDGE ( 'NONE', *, *, #62083, .T. ) ;
#70326 = ORIENTED_EDGE ( 'NONE', *, *, #97731, .T. ) ;
#70327 = DIRECTION ( 'NONE',  ( 0.000000000000000000, -1.000000000000000000, 0.000000000000000000 ) ) ;
#70328 = CARTESIAN_POINT ( 'NONE',  ( -4.169309590939843879, -5.876774720514411854, 19.59793130852656518 ) ) ;
#70329 = DIRECTION ( 'NONE',  ( -3.773278334453079618E-23, 0.9999999999976377785, 2.173523156925979975E-06 ) ) ;
#70330 = CARTESIAN_POINT ( 'NONE',  ( -116.5228709571500616, -23.47596703998600631, 11.44779298504227860 ) ) ;
#70332 = ADVANCED_FACE ( 'NONE', ( #67664 ), #91471, .F. ) ;
#70331 = FACE_BOUND ( 'NONE', #81527, .T. ) ;
#70333 = CARTESIAN_POINT ( 'NONE',  ( -19.49195742049215241, -1.735909528584683947, -1.500000000000002220 ) ) ;
#70334 = CARTESIAN_POINT ( 'NONE',  ( -5.654682302363691626, -5.876774720514410077, 19.41635569784906323 ) ) ;
#70335 = CARTESIAN_POINT ( 'NONE',  ( -4.253298834618286506, 21.06115358058179154, 11.49999999999998934 ) ) ;
#70336 = DIRECTION ( 'NONE',  ( 0.000000000000000000, -2.173523156925979552E-06, 0.9999999999976378895 ) ) ;
#70337 = LINE ( 'NONE', #40886, #72385 ) ;
#70338 = CARTESIAN_POINT ( 'NONE',  ( -68.52287095715006160, -29.50248528299804818, 1.056150453629036701 ) ) ;
#70339 = EDGE_CURVE ( 'NONE', #18921, #10125, #89106, .T. ) ;
#70340 = CARTESIAN_POINT ( 'NONE',  ( -68.62287095715004170, -24.50321055353803601, 9.387540953477524042 ) ) ;
#70341 = CARTESIAN_POINT ( 'NONE',  ( 21.82588152991271713, 6.770963248321698380, -1.500000000000002220 ) ) ;
#70342 = COORDINATED_UNIVERSAL_TIME_OFFSET ( 0, 0, .AHEAD. ) ;
#70343 = CARTESIAN_POINT ( 'NONE',  ( -124.6228709571500559, -24.64965695001469115, 8.947790433994175174 ) ) ;
#70344 = CARTESIAN_POINT ( 'NONE',  ( -53.50785965996792726, -23.96119346886879953, -0.6495511937832126881 ) ) ;
#70345 = CARTESIAN_POINT ( 'NONE',  ( 0.1258803491696451060, 20.03332480481931199, 11.49999999999999645 ) ) ;
#70346 = CARTESIAN_POINT ( 'NONE',  ( -100.5228709571500758, -23.47593901973090524, -1.443836447538996648 ) ) ;
#70347 = CARTESIAN_POINT ( 'NONE',  ( -107.6228709571500701, -24.64898659630368272, 1.056161002820831474 ) ) ;
#70348 = CARTESIAN_POINT ( 'NONE',  ( -53.52287095715006870, -24.64965694238574656, 8.947790433994203596 ) ) ;
#70349 = DIRECTION ( 'NONE',  ( 1.000000000000000000, 0.000000000000000000, 0.000000000000000000 ) ) ;
#70350 = VERTEX_POINT ( 'NONE', #69650 ) ;
#70351 = CARTESIAN_POINT ( 'NONE',  ( -85.62287095715008434, -23.84047902841601640, -0.8780736468305717635 ) ) ;
#70352 = CARTESIAN_POINT ( 'NONE',  ( -19.76859095128058996, -9.124614402804876789, -1.500000000000002220 ) ) ;
#70353 = DIRECTION ( 'NONE',  ( 0.000000000000000000, 1.000000000000000000, 0.000000000000000000 ) ) ;
#70354 = CARTESIAN_POINT ( 'NONE',  ( -8.027368788987615744, 17.96763083595211441, -1.500000000000002220 ) ) ;
#70355 = PLANE ( 'NONE',  #78217 ) ;
#70356 = B_SPLINE_CURVE_WITH_KNOTS ( 'NONE', 3,
 ( #99882, #59863, #98394, #45629 ),
 .UNSPECIFIED., .F., .F.,
 ( 4, 4 ),
 ( 0.9804860655770837319, 0.9894924968491983774 ),
 .UNSPECIFIED. ) ;
#70357 = CARTESIAN_POINT ( 'NONE',  ( -109.6940667814372006, -25.27925840780774536, 5.011372401766285734 ) ) ;
#70358 = APPROVAL_DATE_TIME ( #39405, #15255 ) ;
#70359 = DIRECTION ( 'NONE',  ( 0.000000000000000000, 1.478457507934778393E-16, -1.000000000000000000 ) ) ;
#70360 = CARTESIAN_POINT ( 'NONE',  ( -39.29876498011696384, -25.30691688891204905, 5.130634121476438381 ) ) ;
#70361 = CARTESIAN_POINT ( 'NONE',  ( -4.563637348303267949, -20.04915943051449645, 11.49999999999999645 ) ) ;
#70362 = AXIS2_PLACEMENT_3D ( 'NONE', #99425, #6085, #7584 ) ;
#70363 = CARTESIAN_POINT ( 'NONE',  ( -120.5922450961300143, -23.85016227208581441, -0.8807180028928249804 ) ) ;
#70364 = CARTESIAN_POINT ( 'NONE',  ( 6.494847429386178206, -21.66115869805930672, 11.49999999999999645 ) ) ;
#70365 = ORIENTED_EDGE ( 'NONE', *, *, #4451, .T. ) ;
#70366 = CARTESIAN_POINT ( 'NONE',  ( -80.88924702628075636, -25.30869131066464561, 4.592921213095906730 ) ) ;
#70367 = PLANE ( 'NONE',  #94764 ) ;
#70368 = CARTESIAN_POINT ( 'NONE',  ( -125.6241953133450409, -24.63419186844610920, 9.035850630976920428 ) ) ;
#70369 = DIRECTION ( 'NONE',  ( 0.000000000000000000, -1.000000000000000000, 0.000000000000000000 ) ) ;
#70370 = DIRECTION ( 'NONE',  ( -3.773278334453080206E-23, 0.9999999999976377785, 2.173523156925979975E-06 ) ) ;
#70371 = VECTOR ( 'NONE', #34462, 1000.000000000000000 ) ;
#70372 = CARTESIAN_POINT ( 'NONE',  ( -2.772696838893043747, -6.376774720514413630, 19.95463486386180207 ) ) ;
#70373 = B_SPLINE_CURVE_WITH_KNOTS ( 'NONE', 3,
 ( #18297, #9174, #40135, #40640 ),
 .UNSPECIFIED., .F., .F.,
 ( 4, 4 ),
 ( 0.000000000000000000, 0.0005192307692307995826 ),
 .UNSPECIFIED. ) ;
#70374 = EDGE_LOOP ( 'NONE', ( #33118, #65231 ) ) ;
#70375 = CARTESIAN_POINT ( 'NONE',  ( -22.22199965279648737, -6.226755796435518242, 11.49999999999999645 ) ) ;
#70376 = CARTESIAN_POINT ( 'NONE',  ( 10.87194125936840194, 20.03610521102953257, -1.500000000000002220 ) ) ;
#70377 = CARTESIAN_POINT ( 'NONE',  ( 4.613443512364428400, -5.876774720514412742, 19.38647409819875733 ) ) ;
#70378 = CARTESIAN_POINT ( 'NONE',  ( -96.51886588111300114, -23.73766607897670511, -1.055555164236452681 ) ) ;
#70379 = CARTESIAN_POINT ( 'NONE',  ( -86.52287095715006160, -23.47596703998600631, 11.44779298504228393 ) ) ;
#70380 = CARTESIAN_POINT ( 'NONE',  ( 22.31695869535024102, -2.478243017838637652, 11.49999999999999645 ) ) ;
#70381 = ORIENTED_EDGE ( 'NONE', *, *, #50856, .F. ) ;
#70382 = CARTESIAN_POINT ( 'NONE',  ( -106.5228709571500758, -24.64898659630368627, 1.056161002820831474 ) ) ;
#70383 = CARTESIAN_POINT ( 'NONE',  ( -34.62287095715007013, -24.50321055353804311, 9.387540953477543582 ) ) ;
#70384 = CARTESIAN_POINT ( 'NONE',  ( 21.59112034314636119, 3.954845139028329015, -1.500000000000002220 ) ) ;
#70385 = CARTESIAN_POINT ( 'NONE',  ( -5.824076695599092801, -6.376774720514413630, 19.72913074730691108 ) ) ;
#70386 = CARTESIAN_POINT ( 'NONE',  ( -45.52287095715006160, -29.50250786944525672, 11.44777988621624054 ) ) ;
#70387 = DIRECTION ( 'NONE',  ( -3.773278334444166432E-23, 1.000000000000000000, 0.000000000000000000 ) ) ;
#70388 = VERTEX_POINT ( 'NONE', #6240 ) ;
#70389 = CARTESIAN_POINT ( 'NONE',  ( -92.62287095715005592, -24.64898659630368627, 1.056161002820827921 ) ) ;
#70390 = FACE_OUTER_BOUND ( 'NONE', #12224, .T. ) ;
#70391 = ORIENTED_EDGE ( 'NONE', *, *, #65306, .T. ) ;
#70392 = EDGE_CURVE ( 'NONE', #54069, #60061, #98817, .T. ) ;
#70393 = CARTESIAN_POINT ( 'NONE',  ( -16.05948562299510485, -12.68841425896798469, 11.49999999999998934 ) ) ;
#70394 = VERTEX_POINT ( 'NONE', #68152 ) ;
#70395 = EDGE_LOOP ( 'NONE', ( #82190, #46847, #74155, #57481 ) ) ;
#70396 = ORIENTED_EDGE ( 'NONE', *, *, #28822, .T. ) ;
#70397 = B_SPLINE_CURVE_WITH_KNOTS ( 'NONE', 3,
 ( #18473, #81375, #82366, #49444 ),
 .UNSPECIFIED., .F., .F.,
 ( 4, 4 ),
 ( 1.387778780781445676E-17, 0.0001000000000000028508 ),
 .UNSPECIFIED. ) ;
#70398 = VERTEX_POINT ( 'NONE', #100060 ) ;
#70399 = CARTESIAN_POINT ( 'NONE',  ( -13.16640216892762894, -18.94680327863774849, -1.500000000000002220 ) ) ;
#70400 = CARTESIAN_POINT ( 'NONE',  ( -50.06200402506829761, -25.12646615760390034, 2.865550471351198336 ) ) ;
#70401 = CARTESIAN_POINT ( 'NONE',  ( -20.27173212042777806, -0.06527795377243154895, -1.500000000000002220 ) ) ;
#70402 = EDGE_CURVE ( 'NONE', #24545, #71288, #74738, .T. ) ;
#70403 = EDGE_LOOP ( 'NONE', ( #6763, #17114, #47195, #91093 ) ) ;
#70404 = CARTESIAN_POINT ( 'NONE',  ( 29.71608694565284026, 4.561299274004467996, 27.78615310300602559 ) ) ;
#70405 = CARTESIAN_POINT ( 'NONE',  ( -92.50697978749521155, -24.51314013834316796, 0.6176544820404240577 ) ) ;
#70406 = EDGE_CURVE ( 'NONE', #67931, #93833, #49256, .T. ) ;
#70407 = LINE ( 'NONE', #2913, #48104 ) ;
#70408 = CARTESIAN_POINT ( 'NONE',  ( 4.017909867803298063, -5.876774720514403860, 18.55402206357357286 ) ) ;
#70410 = ORIENTED_EDGE ( 'NONE', *, *, #27290, .T. ) ;
#70409 = CARTESIAN_POINT ( 'NONE',  ( 14.19067371521932230, 16.14321034643037578, 11.49999999999999645 ) ) ;
#70411 = CARTESIAN_POINT ( 'NONE',  ( -75.57899749970765413, -25.00158670708910691, 2.256160236439223699 ) ) ;
#70412 = CARTESIAN_POINT ( 'NONE',  ( 15.11782173391118889, 3.530785491095175921, -28.35562479723308016 ) ) ;
#70413 = EDGE_CURVE ( 'NONE', #31094, #55321, #99078, .T. ) ;
#70414 = VECTOR ( 'NONE', #50382, 1000.000000000000114 ) ;
#70415 = VERTEX_POINT ( 'NONE', #60554 ) ;
#70416 = EDGE_CURVE ( 'NONE', #95213, #97694, #51766, .T. ) ;
#70417 = CARTESIAN_POINT ( 'NONE',  ( 10.87737074370964407, 17.65887017642603851, -1.500000000000002220 ) ) ;
#70418 = EDGE_LOOP ( 'NONE', ( #45466, #9514 ) ) ;
#70420 = EDGE_LOOP ( 'NONE', ( #80261, #51033, #89997, #25320, #16518, #90150, #17438, #83864, #55937, #88171, #49782, #19116, #48155, #31242, #97916, #9688, #74127, #57708, #52573, #87667, #7741, #93332, #748, #98217, #46705, #51311, #85490, #81506, #66839, #50478, #91760, #68800, #99745, #89985, #73592, #6773, #34375, #66661, #86817, #10761, #58525, #18873, #74749, #29400, #35502, #70177, #59589, #93721, #1948, #21394, #52972, #55226, #50203, #56035, #41261, #77010, #14308, #63649, #81315, #29744, #86350, #37079, #636, #70322, #62844, #48146, #34113, #22360, #60081, #32631, #14368, #4665, #56185, #6518, #11603, #86638, #16848, #56587, #81541, #96720, #17976, #5676, #90730, #12747, #18429, #95882, #34632, #50486, #44012, #8666, #10748, #14720, #36228, #50734, #89443, #6848, #92223, #25189, #25107, #13002, #64942 ) ) ;
#70419 = CARTESIAN_POINT ( 'NONE',  ( -7.999999999999996447, -5.876774720514426953, 22.50000000000000355 ) ) ;
#70421 = CARTESIAN_POINT ( 'NONE',  ( -41.64113801341388665, -24.15620529776627379, 10.23563542870660825 ) ) ;
#70422 = CARTESIAN_POINT ( 'NONE',  ( -129.5895376238167387, -23.47596703998600631, 11.44779298504227683 ) ) ;
#70423 = ORIENTED_EDGE ( 'NONE', *, *, #30203, .F. ) ;
#70424 = ORIENTED_EDGE ( 'NONE', *, *, #97294, .F. ) ;
#70425 = DIRECTION ( 'NONE',  ( 0.000000000000000000, -1.478457507934778393E-16, -1.000000000000000000 ) ) ;
#70426 = DIRECTION ( 'NONE',  ( 0.000000000000000000, -2.173523156925979552E-06, 0.9999999999976378895 ) ) ;
#70427 = EDGE_CURVE ( 'NONE', #27337, #884, #67390, .T. ) ;
#70428 = CARTESIAN_POINT ( 'NONE',  ( -31.52287095715006160, -23.47593901973090169, -1.443836447538997536 ) ) ;
#70429 = CARTESIAN_POINT ( 'NONE',  ( 2.959355296939036872, -21.81356824310248399, 11.49999999999999645 ) ) ;
#70430 = DIRECTION ( 'NONE',  ( -0.000000000000000000, 1.000000000000000000, -0.000000000000000000 ) ) ;
#70431 = CARTESIAN_POINT ( 'NONE',  ( -22.55165446212525993, 1.111233042438415808, -1.500000000000002220 ) ) ;
#70432 = CARTESIAN_POINT ( 'NONE',  ( 14.09988904737591575, 15.55221489148801872, -1.500000000000002220 ) ) ;
#70433 = CARTESIAN_POINT ( 'NONE',  ( 6.499999999999992895, -1.818455879622361558E-15, 4.499999999999999112 ) ) ;
#70435 = VERTEX_POINT ( 'NONE', #45319 ) ;
#70434 = FACE_OUTER_BOUND ( 'NONE', #99594, .T. ) ;
#70436 = ORIENTED_EDGE ( 'NONE', *, *, #18400, .T. ) ;
#70437 = CARTESIAN_POINT ( 'NONE',  ( -88.52287095715004739, -24.50321055353805377, 9.387540953477513384 ) ) ;
#70438 = AXIS2_PLACEMENT_3D ( 'NONE', #19320, #34565, #9719 ) ;
#70439 = B_SPLINE_CURVE_WITH_KNOTS ( 'NONE', 3,
 ( #52693, #45089, #29848, #60817 ),
 .UNSPECIFIED., .F., .F.,
 ( 4, 4 ),
 ( 0.000000000000000000, 9.999999999997510880E-05 ),
 .UNSPECIFIED. ) ;
#70440 = CARTESIAN_POINT ( 'NONE',  ( -10.24059822343757808, -6.376774720514426953, 17.17691942396160698 ) ) ;
#70441 = ORIENTED_EDGE ( 'NONE', *, *, #41778, .T. ) ;
#70442 = CARTESIAN_POINT ( 'NONE',  ( 15.93590435955092843, -13.91358336426615239, -1.500000000000002220 ) ) ;
#70443 = CARTESIAN_POINT ( 'NONE',  ( -82.62287095715007013, -24.34917612406837861, 0.1852690917426655925 ) ) ;
#70444 = CARTESIAN_POINT ( 'NONE',  ( -51.63614490863932360, -25.03148624446666304, 7.022166193333077011 ) ) ;
#70445 = CARTESIAN_POINT ( 'NONE',  ( -121.5205784047497275, -23.96119346886880308, -0.6495511937832032512 ) ) ;
#70446 = LINE ( 'NONE', #24264, #5379 ) ;
#70447 = CARTESIAN_POINT ( 'NONE',  ( 4.784292611718075072, 3.316774720514426456, -25.54547254883186014 ) ) ;
#70448 = CARTESIAN_POINT ( 'NONE',  ( -5.848988146064017180, 21.40304369876291446, -1.500000000000002220 ) ) ;
#70449 = CARTESIAN_POINT ( 'NONE',  ( -81.55435809614610321, -23.96169478059713143, 10.65365249895718591 ) ) ;
#70450 = EDGE_CURVE ( 'NONE', #41069, #76295, #4495, .T. ) ;
#70451 = AXIS2_PLACEMENT_3D ( 'NONE', #49457, #19479, #43335 ) ;
#70452 = ORIENTED_EDGE ( 'NONE', *, *, #18605, .T. ) ;
#70453 = CARTESIAN_POINT ( 'NONE',  ( -51.85051548866884019, -25.31633255200107158, 5.725680900099839654 ) ) ;
#70454 = CARTESIAN_POINT ( 'NONE',  ( -60.62287095715004881, -29.50247984919015209, -1.443849546365056913 ) ) ;
#70455 = CARTESIAN_POINT ( 'NONE',  ( -126.5902073896861282, -23.96119346886880663, -0.6495511937832031402 ) ) ;
#70456 = EDGE_CURVE ( 'NONE', #53720, #46308, #6737, .T. ) ;
#70457 = DIRECTION ( 'NONE',  ( -1.000000000000000000, -3.773278334444167608E-23, -8.201307833595939069E-29 ) ) ;
#70458 = CARTESIAN_POINT ( 'NONE',  ( 10.83356970694445209, -2.682774720514426114, -27.03405577723113140 ) ) ;
#70459 = CARTESIAN_POINT ( 'NONE',  ( -3.206006181753352724, -19.19236486397402430, -1.500000000000002220 ) ) ;
#70460 = CARTESIAN_POINT ( 'NONE',  ( 21.30238844577196389, 2.035401582669650544, 11.49999999999998934 ) ) ;
#70461 = LINE ( 'NONE', #60859, #59583 ) ;
#70462 = FACE_OUTER_BOUND ( 'NONE', #85872, .T. ) ;
#70463 = LINE ( 'NONE', #54749, #21154 ) ;
#70464 = CARTESIAN_POINT ( 'NONE',  ( -44.52287095715006870, -23.72773821059535848, 11.05748984161097326 ) ) ;
#70465 = CARTESIAN_POINT ( 'NONE',  ( -12.60694655700363143, 18.86142483545513926, -1.500000000000002220 ) ) ;
#70466 = EDGE_CURVE ( 'NONE', #25473, #37715, #44387, .T. ) ;
#70467 = DIRECTION ( 'NONE',  ( -1.334402673828313093E-16, -0.000000000000000000, -1.000000000000000000 ) ) ;
#70468 = CARTESIAN_POINT ( 'NONE',  ( 14.61581670307174008, 2.682774720514426559, -27.35847990810646024 ) ) ;
#70469 = CARTESIAN_POINT ( 'NONE',  ( 19.84127317031322946, -0.4231496731191971561, 11.49999999999999645 ) ) ;
#70470 = CARTESIAN_POINT ( 'NONE',  ( 5.367993895751241418, -6.376774720514418959, 20.45854982692612722 ) ) ;
#70471 = CARTESIAN_POINT ( 'NONE',  ( -73.62287095715009855, -23.94994826722515313, -0.6494450866351700880 ) ) ;
#70472 = CARTESIAN_POINT ( 'NONE',  ( 32.98733314340959311, -0.3587747205144265483, 2.074222136288530027 ) ) ;
#70473 = ORIENTED_EDGE ( 'NONE', *, *, #66200, .T. ) ;
#70474 = DIRECTION ( 'NONE',  ( 0.000000000000000000, 0.000000000000000000, 1.000000000000000000 ) ) ;
#70475 = ADVANCED_FACE ( 'NONE', ( #61043 ), #91975, .T. ) ;
#70476 = CARTESIAN_POINT ( 'NONE',  ( -30.47287095715007510, -23.47594215783195537, -5.102550391006585557E-05 ) ) ;
#70477 = CARTESIAN_POINT ( 'NONE',  ( -74.52287095715004739, -24.66019654487200441, 8.947790411086112172 ) ) ;
#70478 = CARTESIAN_POINT ( 'NONE',  ( -0.4625342273119020797, 21.68341340789531912, 11.49999999999998934 ) ) ;
#70479 = CARTESIAN_POINT ( 'NONE',  ( -31.62287095715005236, -24.66019654487199020, 8.947790411086138818 ) ) ;
#70480 = CARTESIAN_POINT ( 'NONE',  ( 19.46547125265945155, -1.073068822128883104, -1.500000000000002220 ) ) ;
#70481 = B_SPLINE_CURVE_WITH_KNOTS ( 'NONE', 3,
 ( #77384, #61694, #60698, #14996, #38335, #37841 ),
 .UNSPECIFIED., .F., .F.,
 ( 4, 2, 4 ),
 ( 6.391158118952235087E-06, 0.001387004593080770317, 0.002767618028042588118 ),
 .UNSPECIFIED. ) ;
#70482 = CARTESIAN_POINT ( 'NONE',  ( -123.6228709571501270, -24.35013146730204525, 9.818937971375101270 ) ) ;
#70483 = ORIENTED_EDGE ( 'NONE', *, *, #27693, .T. ) ;
#70484 = B_SPLINE_CURVE_WITH_KNOTS ( 'NONE', 3,
 ( #76060, #15162, #30894, #68463, #53245, #6055 ),
 .UNSPECIFIED., .F., .F.,
 ( 4, 2, 4 ),
 ( 1.570755371633993761E-05, 0.001396183895866086669, 0.002776660238015833410 ),
 .UNSPECIFIED. ) ;
#70485 = AXIS2_PLACEMENT_3D ( 'NONE', #834, #63253, #55640 ) ;
#70486 = CARTESIAN_POINT ( 'NONE',  ( -20.29798418530817017, 1.744846428065259136, 11.49999999999999645 ) ) ;
#70487 = CARTESIAN_POINT ( 'NONE',  ( -80.54344909021948240, -24.63355581998386157, 0.9682620441943954326 ) ) ;
#70488 = PRODUCT_DEFINITION ( 'UNKNOWN', '', #11661, #4356 ) ;
#70489 = CARTESIAN_POINT ( 'NONE',  ( 9.843544857143434967, 6.475225279485573360, -27.49819965379373343 ) ) ;
#70490 = ORIENTED_EDGE ( 'NONE', *, *, #18510, .T. ) ;
#70491 = CARTESIAN_POINT ( 'NONE',  ( -0.06345841168740280758, -22.22848099251229570, 9.439037205594624780 ) ) ;
#70492 = DIRECTION ( 'NONE',  ( 0.000000000000000000, 0.000000000000000000, -1.000000000000000000 ) ) ;
#70493 = CARTESIAN_POINT ( 'NONE',  ( -49.20147844880023058, -25.31601899827206381, 5.321223608784601211 ) ) ;
#70494 = CYLINDRICAL_SURFACE ( 'NONE', #50547, 1.250000000000001110 ) ;
#70495 = CARTESIAN_POINT ( 'NONE',  ( -1.012926118674504883, -5.876774720514415407, 19.92818918856637822 ) ) ;
#70496 = CARTESIAN_POINT ( 'NONE',  ( 7.746586651691365510, 18.53313339873204058, 11.49999999999998934 ) ) ;
#70497 = CARTESIAN_POINT ( 'NONE',  ( -109.5591676267192156, -23.48783264082476663, -1.443836473390089692 ) ) ;
#70498 = ORIENTED_EDGE ( 'NONE', *, *, #59342, .T. ) ;
#70499 = FACE_OUTER_BOUND ( 'NONE', #11244, .T. ) ;
#70500 = CARTESIAN_POINT ( 'NONE',  ( -14.16064136294604303, -18.02537036913223290, 11.49999999999999645 ) ) ;
#70501 = CARTESIAN_POINT ( 'NONE',  ( -20.46125754976198508, 9.905080999540670561, 11.49999999999998934 ) ) ;
#70502 = VERTEX_POINT ( 'NONE', #15341 ) ;
#70503 = CARTESIAN_POINT ( 'NONE',  ( -53.62287095715009855, -24.35013146730203459, 9.818937971375113705 ) ) ;
#70504 = CARTESIAN_POINT ( 'NONE',  ( -28.52287095715004739, -24.18758155425416945, 0.1850819526199724008 ) ) ;
#70505 = DIRECTION ( 'NONE',  ( 0.000000000000000000, 1.000000000000000000, 0.000000000000000000 ) ) ;
#70506 = CARTESIAN_POINT ( 'NONE',  ( -30.57287095715007297, -24.05819166410570276, 10.46738261685066007 ) ) ;
#70507 = VECTOR ( 'NONE', #16212, 1000.000000000000000 ) ;
#70508 = FACE_OUTER_BOUND ( 'NONE', #19603, .T. ) ;
#70509 = CARTESIAN_POINT ( 'NONE',  ( -98.89396085167129513, -25.31200736282745112, 6.074556455972243363 ) ) ;
#70510 = ORIENTED_EDGE ( 'NONE', *, *, #85401, .F. ) ;
#70511 = CARTESIAN_POINT ( 'NONE',  ( -19.36681041099238598, 6.328833669845586485, 11.49999999999998934 ) ) ;
#70512 = EDGE_LOOP ( 'NONE', ( #81678, #11721, #81193, #40941, #83527, #36596, #84700, #46299, #72178, #64672, #52360, #86115, #80424, #74375, #70580, #69139, #7185, #82491, #35910, #96273 ) ) ;
#70513 = EDGE_CURVE ( 'NONE', #52940, #85301, #63827, .T. ) ;
#70514 = CARTESIAN_POINT ( 'NONE',  ( -16.20615075098634961, 16.30094363606528418, -1.500000000000002220 ) ) ;
#70515 = CARTESIAN_POINT ( 'NONE',  ( -7.304748120944324796, -5.876774720514418071, 19.95463486386180563 ) ) ;
#70516 = DIRECTION ( 'NONE',  ( -1.286817348990133655E-16, 0.000000000000000000, 1.000000000000000000 ) ) ;
#70517 = AXIS2_PLACEMENT_3D ( 'NONE', #73304, #88027, #18503 ) ;
#70518 = VERTEX_POINT ( 'NONE', #63557 ) ;
#70519 = DIRECTION ( 'NONE',  ( 0.000000000000000000, 1.000000000000000000, -0.000000000000000000 ) ) ;
#70520 = CIRCLE ( 'NONE', #12200, 91.74549126261076992 ) ;
#70521 = CARTESIAN_POINT ( 'NONE',  ( -53.49127501850180977, -24.51419770103157347, 9.386484678747180510 ) ) ;
#70523 = EDGE_LOOP ( 'NONE', ( #14161, #2029, #38944, #42877 ) ) ;
#70522 = CARTESIAN_POINT ( 'NONE',  ( 21.27783752795556538, -0.9766432368044721812, 11.49999999999999645 ) ) ;
#70524 = EDGE_CURVE ( 'NONE', #13524, #40340, #22612, .T. ) ;
#70525 = ORIENTED_EDGE ( 'NONE', *, *, #59185, .F. ) ;
#70526 = CARTESIAN_POINT ( 'NONE',  ( -21.61287440533560300, 5.199345243644041936, -1.500000000000002220 ) ) ;
#70527 = EDGE_CURVE ( 'NONE', #84975, #32236, #14178, .T. ) ;
#70528 = CARTESIAN_POINT ( 'NONE',  ( 19.88596897151998633, -5.565664080715476913, 11.49999999999998934 ) ) ;
#70529 = ORIENTED_EDGE ( 'NONE', *, *, #99608, .F. ) ;
#70530 = CARTESIAN_POINT ( 'NONE',  ( -109.3320997930167806, -25.31627335646685495, 5.169840710465035905 ) ) ;
#70531 = CARTESIAN_POINT ( 'NONE',  ( -95.50968202525180573, -24.40133493613050319, 9.663955038902802386 ) ) ;
#70532 = ORIENTED_EDGE ( 'NONE', *, *, #81448, .T. ) ;
#70533 = PLANE ( 'NONE',  #36468 ) ;
#70534 = ORIENTED_EDGE ( 'NONE', *, *, #60336, .F. ) ;
#70535 = CARTESIAN_POINT ( 'NONE',  ( -58.48920519830264908, -24.66019654487199730, 8.947790411086117501 ) ) ;
#70536 = CARTESIAN_POINT ( 'NONE',  ( -48.52287095715008292, -23.94994826722564341, -0.6494450866342713624 ) ) ;
#70537 = CARTESIAN_POINT ( 'NONE',  ( -20.64841573231975147, 3.066018724555340746, -1.500000000000002220 ) ) ;
#70538 = EDGE_CURVE ( 'NONE', #28046, #51976, #73497, .T. ) ;
#70539 = CARTESIAN_POINT ( 'NONE',  ( -5.042499505632127565, 21.24692939306837758, 11.49999999999999645 ) ) ;
#70540 = CARTESIAN_POINT ( 'NONE',  ( -26.92109862195654202, -24.89279950334402614, 7.359061847596003680 ) ) ;
#70541 = DIRECTION ( 'NONE',  ( 0.000000000000000000, 0.000000000000000000, -1.000000000000000000 ) ) ;
#70542 = CARTESIAN_POINT ( 'NONE',  ( 18.89768980500364037, -12.13386209897132773, -1.500000000000002220 ) ) ;
#70543 = CARTESIAN_POINT ( 'NONE',  ( -118.5555930860171401, -23.96169478059713853, 10.65365249895717348 ) ) ;
#70544 = CARTESIAN_POINT ( 'NONE',  ( -58.52287095715008292, -24.51283580621365132, 0.6167428607019717068 ) ) ;
#70545 = CARTESIAN_POINT ( 'NONE',  ( 19.57151214508649772, 3.625915217019311583E-15, 0.5000000000000000000 ) ) ;
#70546 = VECTOR ( 'NONE', #85964, 1000.000000000000000 ) ;
#70547 = ORIENTED_EDGE ( 'NONE', *, *, #79097, .F. ) ;
#70548 = EDGE_LOOP ( 'NONE', ( #93726, #97946, #94379, #90382, #40323, #23256, #81753, #60947, #71270, #40661, #50955, #25834 ) ) ;
#70549 = ORIENTED_EDGE ( 'NONE', *, *, #72147, .T. ) ;
#70550 = CARTESIAN_POINT ( 'NONE',  ( 12.49974722350246736, 17.29906535522423638, -1.500000000000002220 ) ) ;
#70551 = CARTESIAN_POINT ( 'NONE',  ( 6.497064355747536268, 21.42967291005575348, 11.49999999999999645 ) ) ;
#70552 = ORIENTED_EDGE ( 'NONE', *, *, #64587, .T. ) ;
#70553 = CARTESIAN_POINT ( 'NONE',  ( -16.48755246578841849, -13.11705038010048163, -1.500000000000002220 ) ) ;
#70554 = CARTESIAN_POINT ( 'NONE',  ( -30.62471892381331529, -24.05745470861603152, -0.4713115009884515927 ) ) ;
#70555 = CARTESIAN_POINT ( 'NONE',  ( -14.87316555497233495, -13.31901947624662519, -1.500000000000002220 ) ) ;
#70556 = FACE_OUTER_BOUND ( 'NONE', #43942, .T. ) ;
#70557 = CARTESIAN_POINT ( 'NONE',  ( 32.85081302853804885, 3.622774720514426949, -13.10817780685210643 ) ) ;
#70558 = CARTESIAN_POINT ( 'NONE',  ( -20.77788740438921522, -7.151594987469691134, -1.500000000000002220 ) ) ;
#70559 = CYLINDRICAL_SURFACE ( 'NONE', #88475, 2.399999999999999911 ) ;
#70560 = VERTEX_POINT ( 'NONE', #8747 ) ;
#70561 = CARTESIAN_POINT ( 'NONE',  ( 0.000000000000000000, 1.826774720514426464, 0.000000000000000000 ) ) ;
#70562 = CARTESIAN_POINT ( 'NONE',  ( -70.58953762381672448, -23.47593901973091235, -1.443836447539006196 ) ) ;
#70563 = CARTESIAN_POINT ( 'NONE',  ( 19.25983760003161294, 7.974354923662064998, 11.49999999999999645 ) ) ;
#70564 = EDGE_CURVE ( 'NONE', #68398, #15801, #32576, .T. ) ;
#70566 = B_SPLINE_CURVE_WITH_KNOTS ( 'NONE', 3,
 ( #91032, #19520, #13401, #83413 ),
 .UNSPECIFIED., .F., .F.,
 ( 4, 4 ),
 ( 0.8411006093570028153, 0.8501070406291183490 ),
 .UNSPECIFIED. ) ;
#70565 = CARTESIAN_POINT ( 'NONE',  ( 31.61404304915243202, -4.508643932895013862, 26.44173824648443727 ) ) ;
#70567 = DIRECTION ( 'NONE',  ( -0.000000000000000000, 2.173523156925979552E-06, -0.9999999999976378895 ) ) ;
#70568 = DIRECTION ( 'NONE',  ( 0.000000000000000000, -0.000000000000000000, -1.000000000000000000 ) ) ;
#70569 = CARTESIAN_POINT ( 'NONE',  ( 0.2649960030224881025, 21.33594185153759426, 11.49999999999998934 ) ) ;
#70570 = CARTESIAN_POINT ( 'NONE',  ( -41.32836283488544638, -4.132774720514426292, 39.26872235229541985 ) ) ;
#70571 = CARTESIAN_POINT ( 'NONE',  ( -117.5228709571501184, -23.96177878511310055, 10.65340807706329684 ) ) ;
#70572 = AXIS2_PLACEMENT_3D ( 'NONE', #56136, #26168, #96676 ) ;
#70573 = EDGE_CURVE ( 'NONE', #75496, #83737, #62536, .T. ) ;
#70574 = CARTESIAN_POINT ( 'NONE',  ( -125.6228709571500559, -29.50247984919015209, -1.443849546365044922 ) ) ;
#70575 = DIRECTION ( 'NONE',  ( -3.773278334453079618E-23, 0.9999999999976377785, 2.173523156925978705E-06 ) ) ;
#70576 = CARTESIAN_POINT ( 'NONE',  ( -11.40494320173684351, 19.43794304404440254, -1.500000000000002220 ) ) ;
#70577 = ADVANCED_FACE ( 'NONE', ( #16852 ), #63049, .T. ) ;
#70578 = VECTOR ( 'NONE', #21443, 1000.000000000000114 ) ;
#70579 = FACE_OUTER_BOUND ( 'NONE', #80445, .T. ) ;
#70580 = ORIENTED_EDGE ( 'NONE', *, *, #45028, .F. ) ;
#70581 = CARTESIAN_POINT ( 'NONE',  ( 5.271800844963591359, 3.316774720514426011, -28.56638892015329034 ) ) ;
#70582 = CARTESIAN_POINT ( 'NONE',  ( -20.27875734969026311, 7.743225279485574042, 25.40402280011862146 ) ) ;
#70583 = CARTESIAN_POINT ( 'NONE',  ( 18.75866648459458830, -6.009157199652424453, 11.49999999999999645 ) ) ;
#70584 = FACE_OUTER_BOUND ( 'NONE', #33732, .T. ) ;
#70585 = VECTOR ( 'NONE', #8794, 1000.000000000000000 ) ;
#70586 = CARTESIAN_POINT ( 'NONE',  ( -120.6228709571500417, -29.50248528299804818, 1.056150453629045360 ) ) ;
#70587 = ORIENTED_EDGE ( 'NONE', *, *, #20566, .F. ) ;
#70588 = AXIS2_PLACEMENT_3D ( 'NONE', #16774, #78655, #9164 ) ;
#70589 = CARTESIAN_POINT ( 'NONE',  ( -99.55496185298399325, -23.96119346886881374, -0.6495511937831867089 ) ) ;
#70590 = CARTESIAN_POINT ( 'NONE',  ( -16.22218391600152643, -6.376774720514426953, -54.85883559227303863 ) ) ;
#70591 = CARTESIAN_POINT ( 'NONE',  ( -61.52287095715009002, -23.73934037231757088, 11.05740245334329153 ) ) ;
#70592 = CARTESIAN_POINT ( 'NONE',  ( -9.607006924060957687, -21.85068815744421045, 11.44779298504228038 ) ) ;
#70593 = CARTESIAN_POINT ( 'NONE',  ( 9.261118129494249729, -17.44851725036260248, -1.500000000000002220 ) ) ;
#70594 = ORIENTED_EDGE ( 'NONE', *, *, #83211, .T. ) ;
#70595 = CARTESIAN_POINT ( 'NONE',  ( -109.4872011792213442, -25.24971315249232262, 3.733106366897268380 ) ) ;
#70596 = EDGE_CURVE ( 'NONE', #93033, #2149, #79750, .T. ) ;
#70597 = PERSON ( 'UNSPECIFIED', 'UNSPECIFIED', 'UNSPECIFIED', ('UNSPECIFIED'), ('UNSPECIFIED'), ('UNSPECIFIED') ) ;
#70598 = COORDINATED_UNIVERSAL_TIME_OFFSET ( 0, 0, .AHEAD. ) ;
#70599 = ORIENTED_EDGE ( 'NONE', *, *, #1144, .T. ) ;
#70600 = DIRECTION ( 'NONE',  ( 0.000000000000000000, 0.000000000000000000, 1.000000000000000000 ) ) ;
#70601 = CARTESIAN_POINT ( 'NONE',  ( 1.949999999999999956, 0.1925000000000000044, -0.1925000000000000600 ) ) ;
#70602 = CARTESIAN_POINT ( 'NONE',  ( -100.5551968661962832, -25.30262289663432185, 4.733994061935349329 ) ) ;
#70603 = CARTESIAN_POINT ( 'NONE',  ( -98.89534031563961491, -25.26638239608887915, 6.173962649882215104 ) ) ;
#70604 = CARTESIAN_POINT ( 'NONE',  ( -67.62287095715005592, -23.47593901973091235, -1.443836447539006196 ) ) ;
#70605 = CARTESIAN_POINT ( 'NONE',  ( -89.81226385320381667, -25.26877915520014994, 5.947789088310639904 ) ) ;
#70606 = CARTESIAN_POINT ( 'NONE',  ( -86.62287095715005592, -23.48786465467241413, 11.44779295918254469 ) ) ;
#70607 = CARTESIAN_POINT ( 'NONE',  ( -3.121018476474317183, -19.76494895549465980, 11.49999999999998934 ) ) ;
#70608 = CARTESIAN_POINT ( 'NONE',  ( -58.62287095715004881, -23.47593901973091235, -1.443836447539007972 ) ) ;
#70609 = CARTESIAN_POINT ( 'NONE',  ( -116.6242992002620440, -24.51419770103160189, 9.386484678747169852 ) ) ;
#70610 = VERTEX_POINT ( 'NONE', #23957 ) ;
#70611 = EDGE_CURVE ( 'NONE', #66746, #90746, #62525, .T. ) ;
#70612 = ADVANCED_FACE ( 'NONE', ( #78730 ), #1136, .F. ) ;
#70613 = CARTESIAN_POINT ( 'NONE',  ( -79.51271330033607398, -23.96169478059713143, 10.65365249895718058 ) ) ;
#70614 = AXIS2_PLACEMENT_3D ( 'NONE', #99051, #6713, #37666 ) ;
#70615 = CARTESIAN_POINT ( 'NONE',  ( -109.6405337342305302, -25.18430212153996095, 3.562353486846156603 ) ) ;
#70616 = CARTESIAN_POINT ( 'NONE',  ( -35.54076835017719560, -24.40034930558991277, 0.3402023900116170063 ) ) ;
#70617 = DIRECTION ( 'NONE',  ( 0.9831680378442392287, 0.000000000000000000, 0.1827036106964188000 ) ) ;
#70618 = CARTESIAN_POINT ( 'NONE',  ( 13.91401389203221406, 6.376774720514426953, 158.0376437107427137 ) ) ;
#70619 = CARTESIAN_POINT ( 'NONE',  ( 30.93860345374796594, -2.297196155479622526, 24.67598410064775294 ) ) ;
#70620 = B_SPLINE_CURVE_WITH_KNOTS ( 'NONE', 3,
 ( #78122, #66692, #97603, #89998, #80146, #3036 ),
 .UNSPECIFIED., .F., .F.,
 ( 4, 2, 4 ),
 ( 0.000000000000000000, 0.001380901958385387894, 0.002761803916770775788 ),
 .UNSPECIFIED. ) ;
#70621 = CARTESIAN_POINT ( 'NONE',  ( -62.62287095715004881, -23.48786465467241058, 11.44779295918254824 ) ) ;
#70622 = CARTESIAN_POINT ( 'NONE',  ( -73.62287095715007013, -23.96127896941632685, -0.6493128931037860374 ) ) ;
#70623 = ORIENTED_EDGE ( 'NONE', *, *, #8253, .T. ) ;
#70624 = CARTESIAN_POINT ( 'NONE',  ( 14.62039552936377085, -14.08751720214925207, -1.500000000000002220 ) ) ;
#70625 = EDGE_CURVE ( 'NONE', #73156, #11909, #91637, .T. ) ;
#70626 = FACE_OUTER_BOUND ( 'NONE', #627, .T. ) ;
#70627 = DIRECTION ( 'NONE',  ( 1.000000000000000000, 3.773278334444166432E-23, 8.201307841325785021E-29 ) ) ;
#70628 = ORIENTED_EDGE ( 'NONE', *, *, #67200, .F. ) ;
#70629 = CARTESIAN_POINT ( 'NONE',  ( -32.99388727629348494, -25.12026506542017046, 2.831122744435439209 ) ) ;
#70630 = CARTESIAN_POINT ( 'NONE',  ( -17.16780662754360520, -10.58209718439171176, -1.500000000000002220 ) ) ;
#70631 = CARTESIAN_POINT ( 'NONE',  ( 17.61891135320703938, 11.69080507458975227, 11.49999999999999645 ) ) ;
#70632 = CARTESIAN_POINT ( 'NONE',  ( 14.84500176111689207, -16.38379996218902335, -1.500000000000002220 ) ) ;
#70633 = EDGE_CURVE ( 'NONE', #2140, #41031, #83191, .T. ) ;
#70634 = CARTESIAN_POINT ( 'NONE',  ( 18.81462172601333549, -8.267562025728075525, 11.49999999999998934 ) ) ;
#70635 = AXIS2_PLACEMENT_3D ( 'NONE', #4497, #59271, #43552 ) ;
#70636 = DIRECTION ( 'NONE',  ( 0.6599726524652352877, -0.000000000000000000, -0.7512896232465891000 ) ) ;
#70637 = EDGE_LOOP ( 'NONE', ( #99746, #13889, #47181, #63435 ) ) ;
#70638 = LINE ( 'NONE', #92961, #18520 ) ;
#70639 = VERTEX_POINT ( 'NONE', #1642 ) ;
#70640 = EDGE_CURVE ( 'NONE', #25509, #96582, #64063, .T. ) ;
#70641 = DIRECTION ( 'NONE',  ( -3.773278334444166432E-23, 1.000000000000000000, 0.000000000000000000 ) ) ;
#70642 = CARTESIAN_POINT ( 'NONE',  ( -86.22287095715006444, -23.47593901973090169, -1.443836447538996870 ) ) ;
#70643 = ORIENTED_EDGE ( 'NONE', *, *, #31698, .F. ) ;
#70644 = AXIS2_PLACEMENT_3D ( 'NONE', #64602, #95516, #73190 ) ;
#70645 = ORIENTED_EDGE ( 'NONE', *, *, #19983, .F. ) ;
#70646 = AXIS2_PLACEMENT_3D ( 'NONE', #23013, #33533, #25417 ) ;
#70647 = ORIENTED_EDGE ( 'NONE', *, *, #49112, .F. ) ;
#70648 = CARTESIAN_POINT ( 'NONE',  ( -110.9760276224984779, -25.14607537338261523, 2.978229960058158099 ) ) ;
#70649 = CARTESIAN_POINT ( 'NONE',  ( 6.910430652544937935, -5.876774720514418071, 20.24472806504191169 ) ) ;
#70650 = CARTESIAN_POINT ( 'NONE',  ( -68.63577537931014660, -24.15620529776627734, 10.23563542870660825 ) ) ;
#70651 = CARTESIAN_POINT ( 'NONE',  ( -4.528870947376731237, 20.18191347215651987, -1.500000000000002220 ) ) ;
#70652 = EDGE_CURVE ( 'NONE', #92001, #51471, #72655, .T. ) ;
#70653 = AXIS2_PLACEMENT_3D ( 'NONE', #78673, #2095, #25410 ) ;
#70654 = CARTESIAN_POINT ( 'NONE',  ( 18.46943957830784555, -11.30625484363265265, 11.49999999999999645 ) ) ;
#70655 = ORIENTED_EDGE ( 'NONE', *, *, #5015, .T. ) ;
#70656 = CARTESIAN_POINT ( 'NONE',  ( 13.57151214508650305, 0.000000000000000000, 1.500000000000000666 ) ) ;
#70657 = CARTESIAN_POINT ( 'NONE',  ( 3.797776442307698286, -5.876774720514402084, 18.16025641025640525 ) ) ;
#70658 = CARTESIAN_POINT ( 'NONE',  ( -1.374798071107336206, -22.32369649477951512, -1.500000000000002220 ) ) ;
#70659 = AXIS2_PLACEMENT_3D ( 'NONE', #90587, #21065, #36807 ) ;
#70660 = EDGE_CURVE ( 'NONE', #25743, #20125, #60219, .T. ) ;
#70661 = CARTESIAN_POINT ( 'NONE',  ( -47.53537244378864557, -24.51419770103156637, 9.386484678747176957 ) ) ;
#70662 = CARTESIAN_POINT ( 'NONE',  ( -101.5228709571500332, -23.95044443724991723, 10.65354141964649237 ) ) ;
#70663 = ORIENTED_EDGE ( 'NONE', *, *, #2132, .F. ) ;
#70664 = CARTESIAN_POINT ( 'NONE',  ( -119.2832211118485333, -25.38369257465123496, 5.756917303100165029 ) ) ;
#70665 = CARTESIAN_POINT ( 'NONE',  ( -52.55620429048339304, -24.64965694238575011, 8.947790433994201820 ) ) ;
#70666 = EDGE_LOOP ( 'NONE', ( #19256, #78281, #45834, #51817 ) ) ;
#70667 = CARTESIAN_POINT ( 'NONE',  ( -45.52287095715006160, -24.82576562948885623, 8.398263436605494903 ) ) ;
#70668 = ORIENTED_EDGE ( 'NONE', *, *, #60323, .F. ) ;
#70669 = FACE_OUTER_BOUND ( 'NONE', #34160, .T. ) ;
#70670 = CARTESIAN_POINT ( 'NONE',  ( -10.65520286329281596, -18.28862552182625123, -1.500000000000002220 ) ) ;
#70671 = ORIENTED_EDGE ( 'NONE', *, *, #32701, .T. ) ;
#70672 = CARTESIAN_POINT ( 'NONE',  ( -50.55080355490176203, -24.15503026093912808, -0.2815557561904566963 ) ) ;
#70673 = CARTESIAN_POINT ( 'NONE',  ( -21.69466673205137752, 2.402554924997643226, -1.500000000000002220 ) ) ;
#70674 = CARTESIAN_POINT ( 'NONE',  ( -7.635352852713973348, -6.376774720514415407, 20.14409848895066091 ) ) ;
#70675 = DIRECTION ( 'NONE',  ( 0.9848077530122089085, 0.1736481776669261956, 0.000000000000000000 ) ) ;
#70676 = CARTESIAN_POINT ( 'NONE',  ( -109.5562042904833788, -24.65952944569305316, 1.056160979905704345 ) ) ;
#70677 = CARTESIAN_POINT ( 'NONE',  ( -21.01659442711627790, -5.882202039844940167, -1.500000000000002220 ) ) ;
#70678 = LINE ( 'NONE', #93500, #30153 ) ;
#70679 = ORIENTED_EDGE ( 'NONE', *, *, #32754, .T. ) ;
#70680 = CARTESIAN_POINT ( 'NONE',  ( -41.62287095715006302, -23.47593901973091235, -1.443836447539011525 ) ) ;
#70681 = CARTESIAN_POINT ( 'NONE',  ( -51.62287095715005592, -23.48783264082478084, -1.443836473390070596 ) ) ;
#70682 = ORIENTED_EDGE ( 'NONE', *, *, #2908, .T. ) ;
#70683 = AXIS2_PLACEMENT_3D ( 'NONE', #6183, #52869, #6682 ) ;
#70684 = ORIENTED_EDGE ( 'NONE', *, *, #73670, .F. ) ;
#70685 = EDGE_CURVE ( 'NONE', #30482, #59154, #58924, .T. ) ;
#70686 = EDGE_LOOP ( 'NONE', ( #83054, #8986, #24707, #91389 ) ) ;
#70687 = DIRECTION ( 'NONE',  ( -0.9913618264504693300, -5.365801633547209345E-16, 0.1311553622875920033 ) ) ;
#70688 = FACE_OUTER_BOUND ( 'NONE', #72065, .T. ) ;
#70689 = CARTESIAN_POINT ( 'NONE',  ( 3.248270302591931724, 20.98854991013365279, -1.500000000000002220 ) ) ;
#70690 = CARTESIAN_POINT ( 'NONE',  ( -121.6228709571500417, -24.50216790748098816, 0.6166512839513769162 ) ) ;
#70691 = CARTESIAN_POINT ( 'NONE',  ( -130.5728709571500588, -24.57438384523504027, 0.5319095616429418971 ) ) ;
#70692 = CARTESIAN_POINT ( 'NONE',  ( 27.53860345374808105, -5.356774720496559894, 1.647607965253213402 ) ) ;
#70693 = PLANE ( 'NONE',  #91281 ) ;
#70694 = CARTESIAN_POINT ( 'NONE',  ( 15.46825748771582631, 11.69065726450791409, -1.500000000000002220 ) ) ;
#70695 = EDGE_CURVE ( 'NONE', #22271, #9985, #73647, .T. ) ;
#70696 = CARTESIAN_POINT ( 'NONE',  ( -40.94210688951491051, -25.03707806782366418, 7.590868867492675420 ) ) ;
#70697 = ORIENTED_EDGE ( 'NONE', *, *, #62263, .T. ) ;
#70698 = B_SPLINE_CURVE_WITH_KNOTS ( 'NONE', 3,
 ( #8440, #78437, #76433, #8938 ),
 .UNSPECIFIED., .F., .F.,
 ( 4, 4 ),
 ( 0.000000000000000000, 0.0001000000000000167422 ),
 .UNSPECIFIED. ) ;
#70699 = CARTESIAN_POINT ( 'NONE',  ( -16.16875682573952133, 10.94412424577950915, 11.49999999999999645 ) ) ;
#70700 = CARTESIAN_POINT ( 'NONE',  ( -42.52287095715007581, -24.33927499327854349, 9.819080762295817166 ) ) ;
#70701 = CARTESIAN_POINT ( 'NONE',  ( -68.52287095715004739, -24.50216790748206463, 0.6166512839542471758 ) ) ;
#70702 = ORIENTED_EDGE ( 'NONE', *, *, #18038, .F. ) ;
#70703 = B_SPLINE_CURVE_WITH_KNOTS ( 'NONE', 3,
 ( #69707, #76297, #30129, #30632 ),
 .UNSPECIFIED., .F., .F.,
 ( 4, 4 ),
 ( 0.2206575661668280786, 0.2296639974389436401 ),
 .UNSPECIFIED. ) ;
#70704 = CARTESIAN_POINT ( 'NONE',  ( -93.62287095715005592, -24.64898659630367916, 1.056161002820827921 ) ) ;
#70705 = PLANE ( 'NONE',  #85449 ) ;
#70706 = AXIS2_PLACEMENT_3D ( 'NONE', #64397, #25294, #25800 ) ;
#70707 = DIRECTION ( 'NONE',  ( -0.000000000000000000, 1.000000000000000000, -0.000000000000000000 ) ) ;
#70708 = CARTESIAN_POINT ( 'NONE',  ( -93.63682493047612354, -23.73791477778911840, 11.05961554403170410 ) ) ;
#70709 = CARTESIAN_POINT ( 'NONE',  ( -15.16444148636751521, -12.51942901160708921, 11.49999999999998934 ) ) ;
#70710 = CARTESIAN_POINT ( 'NONE',  ( -41.08147698621603894, -25.31583728001788103, 4.883364621082173507 ) ) ;
#70711 = ORIENTED_EDGE ( 'NONE', *, *, #39788, .F. ) ;
#70712 = CARTESIAN_POINT ( 'NONE',  ( 21.54666897473465070, 1.519730039111064412, 11.49999999999998934 ) ) ;
#70713 = DIRECTION ( 'NONE',  ( -3.773278334453080206E-23, 0.9999999999976377785, 2.173523156925979975E-06 ) ) ;
#70714 = CARTESIAN_POINT ( 'NONE',  ( -5.366453405989236813, 7.470345474798854293E-16, -6.099999999999999645 ) ) ;
#70715 = CARTESIAN_POINT ( 'NONE',  ( 1.702247502073919394, 23.03039350466679025, -1.500000000000002220 ) ) ;
#70716 = ADVANCED_FACE ( 'NONE', ( #34092 ), #74634, .F. ) ;
#70717 = DATE_AND_TIME ( #70220, #63548 ) ;
#70718 = CARTESIAN_POINT ( 'NONE',  ( -92.52287095715006160, -23.47593901973090169, -1.443836447538996426 ) ) ;
#70719 = PLANE ( 'NONE',  #65279 ) ;
#70720 = CYLINDRICAL_SURFACE ( 'NONE', #81732, 1.050000000000000488 ) ;
#70721 = CARTESIAN_POINT ( 'NONE',  ( -104.5228709571500190, -23.95044443724992078, 10.65354141964649415 ) ) ;
#70722 = AXIS2_PLACEMENT_3D ( 'NONE', #28339, #74025, #82623 ) ;
#70724 = CARTESIAN_POINT ( 'NONE',  ( -111.6658724870577117, -25.10921570101833211, 3.734856220746116673 ) ) ;
#70723 = AXIS2_PLACEMENT_3D ( 'NONE', #56089, #36977, #84141 ) ;
#70725 = FACE_OUTER_BOUND ( 'NONE', #76441, .T. ) ;
#70726 = CARTESIAN_POINT ( 'NONE',  ( -99.12380231474227799, -25.31565897376004415, 4.001575044103979018 ) ) ;
#70727 = CARTESIAN_POINT ( 'NONE',  ( 2.927915493035635031, 19.71835975189664936, 11.49999999999998934 ) ) ;
#70729 = ADVANCED_FACE ( 'NONE', ( #88372 ), #43696, .T. ) ;
#70728 = CARTESIAN_POINT ( 'NONE',  ( -75.54715773856550243, -24.40133493613049964, 9.663955038902805939 ) ) ;
#70730 = CARTESIAN_POINT ( 'NONE',  ( 1.158388978951967463, 19.79969207489630634, -1.500000000000002220 ) ) ;
#70731 = EDGE_LOOP ( 'NONE', ( #51697, #98484, #87902, #31213 ) ) ;
#70732 = EDGE_CURVE ( 'NONE', #10916, #29962, #57941, .T. ) ;
#70733 = AXIS2_PLACEMENT_3D ( 'NONE', #2481, #77576, #1984 ) ;
#70734 = CARTESIAN_POINT ( 'NONE',  ( -56.51486553911006183, -23.73766607897670511, -1.055555164236459342 ) ) ;
#70735 = EDGE_CURVE ( 'NONE', #22648, #82699, #98796, .T. ) ;
#70736 = EDGE_CURVE ( 'NONE', #39701, #73698, #54103, .T. ) ;
#70737 = DIRECTION ( 'NONE',  ( 0.000000000000000000, 0.000000000000000000, -1.000000000000000000 ) ) ;
#70738 = LINE ( 'NONE', #32667, #44313 ) ;
#70739 = CARTESIAN_POINT ( 'NONE',  ( -20.55201672899488585, 2.666056886502145673, 11.49999999999999645 ) ) ;
#70740 = CARTESIAN_POINT ( 'NONE',  ( -86.52287095715006160, -24.65952944569304606, 1.056160979905700570 ) ) ;
#70741 = CARTESIAN_POINT ( 'NONE',  ( -88.62287095715005592, -24.33832256526968862, 0.1851278514119913954 ) ) ;
#70742 = CARTESIAN_POINT ( 'NONE',  ( 7.803535043518188274, -21.38454823780343617, 11.49999999999999645 ) ) ;
#70743 = ORIENTED_EDGE ( 'NONE', *, *, #85492, .F. ) ;
#70744 = DIRECTION ( 'NONE',  ( -0.000000000000000000, -0.000000000000000000, -1.000000000000000000 ) ) ;
#70745 = CARTESIAN_POINT ( 'NONE',  ( -70.07901916590789426, -25.12717508165702895, 7.077626925157802340 ) ) ;
#70746 = ORIENTED_EDGE ( 'NONE', *, *, #75795, .T. ) ;
#70747 = CARTESIAN_POINT ( 'NONE',  ( -17.27845874757997535, -10.49745931960568335, 11.49999999999998934 ) ) ;
#70748 = EDGE_CURVE ( 'NONE', #33585, #53678, #80681, .T. ) ;
#70749 = EDGE_CURVE ( 'NONE', #98717, #34234, #27499, .T. ) ;
#70750 = LINE ( 'NONE', #46911, #20873 ) ;
#70751 = CARTESIAN_POINT ( 'NONE',  ( -97.62287095715004170, -24.50321055353806088, 9.387540953477529371 ) ) ;
#70752 = ORIENTED_EDGE ( 'NONE', *, *, #39000, .T. ) ;
#70753 = FACE_OUTER_BOUND ( 'NONE', #71321, .T. ) ;
#70754 = CARTESIAN_POINT ( 'NONE',  ( -8.048360580058307789, -21.46040670285860230, -1.500000000000002220 ) ) ;
#70755 = CARTESIAN_POINT ( 'NONE',  ( -50.75699389676201889, -25.18439660648728307, 3.343798628745027202 ) ) ;
#70756 = CARTESIAN_POINT ( 'NONE',  ( 10.17626895549074817, -17.22257424524772418, -1.500000000000002220 ) ) ;
#70757 = DIRECTION ( 'NONE',  ( 0.000000000000000000, 0.000000000000000000, 1.000000000000000000 ) ) ;
#70758 = CARTESIAN_POINT ( 'NONE',  ( 11.32296221242833667, -17.63459971646239310, 11.49999999999999645 ) ) ;
#70759 = ORIENTED_EDGE ( 'NONE', *, *, #83388, .T. ) ;
#70760 = AXIS2_PLACEMENT_3D ( 'NONE', #35758, #43865, #74795 ) ;
#70761 = DIRECTION ( 'NONE',  ( 0.000000000000000000, -1.000000000000000000, 0.000000000000000000 ) ) ;
#70762 = DIRECTION ( 'NONE',  ( 0.000000000000000000, -1.000000000000000000, 0.000000000000000000 ) ) ;
#70763 = CARTESIAN_POINT ( 'NONE',  ( -21.70078857174656761, -3.768841730229552045, -1.500000000000002220 ) ) ;
#70764 = EDGE_CURVE ( 'NONE', #67184, #86369, #42713, .T. ) ;
#70765 = LINE ( 'NONE', #63674, #4164 ) ;
#70766 = VERTEX_POINT ( 'NONE', #18851 ) ;
#70767 = CARTESIAN_POINT ( 'NONE',  ( -49.79812375574695693, -25.18440137848927307, 3.459241766176638144 ) ) ;
#70768 = CARTESIAN_POINT ( 'NONE',  ( -43.52287095715006160, -23.48786465467240347, 11.44779295918255180 ) ) ;
#70769 = ORIENTED_EDGE ( 'NONE', *, *, #16911, .F. ) ;
#70770 = CARTESIAN_POINT ( 'NONE',  ( 2.650685085285006348, -6.376774720514410077, 19.28073557658628445 ) ) ;
#70771 = EDGE_LOOP ( 'NONE', ( #4556, #54424, #8419, #3987 ) ) ;
#70772 = VERTEX_POINT ( 'NONE', #89866 ) ;
#70773 = CARTESIAN_POINT ( 'NONE',  ( -101.5084176993576648, -25.26303730729093644, 3.986250639247583827 ) ) ;
#70774 = CARTESIAN_POINT ( 'NONE',  ( -101.0021142486707646, -25.10935827596331649, 2.948027515349565419 ) ) ;
#70775 = CARTESIAN_POINT ( 'NONE',  ( -4.141025641025641413, -5.876774720514419847, 20.67377804487180271 ) ) ;
#70776 = CARTESIAN_POINT ( 'NONE',  ( 1.945971545120378288, -20.36639758168144709, -1.500000000000002220 ) ) ;
#70777 = ADVANCED_FACE ( 'NONE', ( #20336 ), #51308, .F. ) ;
#70778 = ORIENTED_EDGE ( 'NONE', *, *, #19087, .F. ) ;
#70779 = CARTESIAN_POINT ( 'NONE',  ( -79.52287095715006160, -24.50216790748204687, 0.6166512839542530600 ) ) ;
#70780 = FACE_OUTER_BOUND ( 'NONE', #76725, .T. ) ;
#70781 = DIRECTION ( 'NONE',  ( 0.000000000000000000, 0.000000000000000000, -1.000000000000000000 ) ) ;
#70782 = CARTESIAN_POINT ( 'NONE',  ( 22.20884612314100792, -2.053178116692622623, 11.49999999999998934 ) ) ;
#70783 = VECTOR ( 'NONE', #91050, 1000.000000000000000 ) ;
#70784 = EDGE_CURVE ( 'NONE', #42731, #41980, #24950, .T. ) ;
#70785 = CARTESIAN_POINT ( 'NONE',  ( -32.62287095715004881, -24.64965695001467694, 8.947790433994189385 ) ) ;
#70786 = PLANE ( 'NONE',  #82031 ) ;
#70787 = ORIENTED_EDGE ( 'NONE', *, *, #36492, .T. ) ;
#70788 = EDGE_CURVE ( 'NONE', #37472, #72942, #17589, .T. ) ;
#70789 = CARTESIAN_POINT ( 'NONE',  ( -29.76961320961419588, -25.20477499778818498, 4.020760705257079515 ) ) ;
#70790 = B_SPLINE_CURVE_WITH_KNOTS ( 'NONE', 3,
 ( #52724, #45121, #76040, #53230 ),
 .UNSPECIFIED., .F., .F.,
 ( 4, 4 ),
 ( 0.1098643759392575470, 0.1188708072113730391 ),
 .UNSPECIFIED. ) ;
#70791 = FACE_OUTER_BOUND ( 'NONE', #38818, .T. ) ;
#70792 = CARTESIAN_POINT ( 'NONE',  ( -10.15938669249390180, 18.18672505111813464, -1.500000000000002220 ) ) ;
#70793 = ORIENTED_EDGE ( 'NONE', *, *, #95620, .F. ) ;
#70795 = VERTEX_POINT ( 'NONE', #45199 ) ;
#70794 = CARTESIAN_POINT ( 'NONE',  ( -52.52287095715006870, -24.65952944569303895, 1.056160979905693686 ) ) ;
#70796 = AXIS2_PLACEMENT_3D ( 'NONE', #96227, #81500, #42452 ) ;
#70797 = ORIENTED_EDGE ( 'NONE', *, *, #77957, .T. ) ;
#70799 = EDGE_CURVE ( 'NONE', #8977, #29704, #20838, .T. ) ;
#70798 = CARTESIAN_POINT ( 'NONE',  ( -118.6228709571500701, -23.47596703998600631, 11.44779298504227683 ) ) ;
#70800 = CARTESIAN_POINT ( 'NONE',  ( -19.96636262075925927, 6.592627302904066511, -1.500000000000002220 ) ) ;
#70801 = ORIENTED_EDGE ( 'NONE', *, *, #70625, .T. ) ;
#70802 = VECTOR ( 'NONE', #91136, 1000.000000000000114 ) ;
#70803 = CARTESIAN_POINT ( 'NONE',  ( -118.5228709571500474, -23.95044443724993144, 10.65354141964648882 ) ) ;
#70804 = CARTESIAN_POINT ( 'NONE',  ( 8.160000000000000142, -10.65233964170348635, -1.621096496867198589 ) ) ;
#70805 = CARTESIAN_POINT ( 'NONE',  ( 8.309867465290103894, -5.356774720514426491, -25.05695269341429920 ) ) ;
#70806 = AXIS2_PLACEMENT_3D ( 'NONE', #32103, #61077, #24491 ) ;
#70807 = CARTESIAN_POINT ( 'NONE',  ( -86.54256729674141013, -24.66019654487200086, 8.947790411086117501 ) ) ;
#70808 = DIRECTION ( 'NONE',  ( 1.000000000000000000, 3.773278334444166432E-23, 8.201307841325785021E-29 ) ) ;
#70809 = DIRECTION ( 'NONE',  ( 0.000000000000000000, 0.000000000000000000, 1.000000000000000000 ) ) ;
#70811 = ORIENTED_EDGE ( 'NONE', *, *, #77135, .T. ) ;
#70810 = CARTESIAN_POINT ( 'NONE',  ( -20.56814720681451902, 8.302189128749821734, 11.49999999999999645 ) ) ;
#70812 = LINE ( 'NONE', #17010, #27540 ) ;
#70813 = CARTESIAN_POINT ( 'NONE',  ( -90.30662536647538730, -25.32594422361629327, 4.020877017707874757 ) ) ;
#70814 = ORIENTED_EDGE ( 'NONE', *, *, #47375, .T. ) ;
#70815 = CARTESIAN_POINT ( 'NONE',  ( -21.72567761722203628, 6.514095075961352954, 11.49999999999998934 ) ) ;
#70816 = VECTOR ( 'NONE', #84280, 1000.000000000000000 ) ;
#70818 = ORIENTED_EDGE ( 'NONE', *, *, #92369, .F. ) ;
#70817 = CARTESIAN_POINT ( 'NONE',  ( -76.62287095715005592, -23.94994826722514958, -0.6494450866351715312 ) ) ;
#70819 = EDGE_LOOP ( 'NONE', ( #7782, #69895, #87675, #32594 ) ) ;
#70820 = DIRECTION ( 'NONE',  ( -0.000000000000000000, 1.000000000000000000, -0.000000000000000000 ) ) ;
#70821 = CARTESIAN_POINT ( 'NONE',  ( 17.50376878386636292, -9.983289808088789741, 11.49999999999998934 ) ) ;
#70822 = CARTESIAN_POINT ( 'NONE',  ( -80.62287095715007013, -24.52232992886361984, 0.6492154411906119194 ) ) ;
#70823 = ORIENTED_EDGE ( 'NONE', *, *, #78088, .F. ) ;
#70824 = DIRECTION ( 'NONE',  ( -3.773278334453080206E-23, 0.9999999999976377785, 2.173523156925979975E-06 ) ) ;
#70825 = CARTESIAN_POINT ( 'NONE',  ( -17.72129891523481149, -13.73837202384828515, -1.500000000000002220 ) ) ;
#70826 = B_SPLINE_CURVE_WITH_KNOTS ( 'NONE', 3,
 ( #62776, #23168, #78462, #54158 ),
 .UNSPECIFIED., .F., .F.,
 ( 4, 4 ),
 ( 0.5291485173198170466, 0.5301492643605828503 ),
 .UNSPECIFIED. ) ;
#70827 = EDGE_LOOP ( 'NONE', ( #77403, #56214, #71694, #79769 ) ) ;
#70828 = ORIENTED_EDGE ( 'NONE', *, *, #41819, .T. ) ;
#70829 = LINE ( 'NONE', #42886, #33626 ) ;
#70830 = CARTESIAN_POINT ( 'NONE',  ( -94.63061136128430917, -24.15620529776628089, 10.23563542870660470 ) ) ;
#70831 = CARTESIAN_POINT ( 'NONE',  ( -115.5228709571500616, -24.99156044556202616, 7.747789690856173195 ) ) ;
#70832 = VECTOR ( 'NONE', #91628, 1000.000000000000000 ) ;
#70833 = CARTESIAN_POINT ( 'NONE',  ( -106.5228709571500758, -29.50248528299804818, 1.056150453629043584 ) ) ;
#70834 = FACE_BOUND ( 'NONE', #52795, .T. ) ;
#70835 = CARTESIAN_POINT ( 'NONE',  ( -12.82114019720147802, -14.77593736753402709, -1.500000000000002220 ) ) ;
#70836 = PLANE ( 'NONE',  #96009 ) ;
#70837 = VERTEX_POINT ( 'NONE', #22331 ) ;
#70838 = CARTESIAN_POINT ( 'NONE',  ( 7.367719877546908158, -20.20905560389912026, 11.49999999999998934 ) ) ;
#70839 = VECTOR ( 'NONE', #3339, 1000.000000000000000 ) ;
#70840 = CARTESIAN_POINT ( 'NONE',  ( -128.6238584515385242, -24.15543982623908548, -0.2315651400026392803 ) ) ;
#70841 = CARTESIAN_POINT ( 'NONE',  ( -54.62287095715004170, -23.47596703998600631, 11.44779298504227505 ) ) ;
#70842 = CARTESIAN_POINT ( 'NONE',  ( -113.5228709571500758, -23.96177878511310055, 10.65340807706329151 ) ) ;
#70843 = CARTESIAN_POINT ( 'NONE',  ( -2.499999999999993339, 4.999999999999997335, 2.100000000000000089 ) ) ;
#70844 = CARTESIAN_POINT ( 'NONE',  ( 21.75294195941402364, -7.338126679257295670, -1.500000000000002220 ) ) ;
#70845 = EDGE_CURVE ( 'NONE', #52051, #76238, #37003, .T. ) ;
#70846 = PERSON_AND_ORGANIZATION_ROLE ( 'design_owner' ) ;
#70847 = PLANE ( 'NONE',  #19132 ) ;
#70848 = CARTESIAN_POINT ( 'NONE',  ( -71.27691565640060389, -25.27723027174688042, 5.969665484188881877 ) ) ;
#70849 = CARTESIAN_POINT ( 'NONE',  ( -3.121018476474317183, -19.76494895549465980, 11.49999999999999645 ) ) ;
#70850 = CARTESIAN_POINT ( 'NONE',  ( -78.94637683104262749, -25.26612659742505329, 5.821637768010305081 ) ) ;
#70851 = CARTESIAN_POINT ( 'NONE',  ( 30.53060340732035982, 5.115583282868248816, -0.7333795357140852067 ) ) ;
#70852 = EDGE_CURVE ( 'NONE', #38855, #89848, #69717, .T. ) ;
#70853 = EDGE_CURVE ( 'NONE', #32034, #61298, #84260, .T. ) ;
#70854 = CARTESIAN_POINT ( 'NONE',  ( 4.912344403463128728, -5.876774720514409189, 19.26008510998990886 ) ) ;
#70855 = DIRECTION ( 'NONE',  ( 1.000000000000000000, 0.000000000000000000, 0.000000000000000000 ) ) ;
#70856 = ORIENTED_EDGE ( 'NONE', *, *, #7495, .F. ) ;
#70857 = CARTESIAN_POINT ( 'NONE',  ( 32.73857899460460175, -1.684774720514424118, -13.20677013500359820 ) ) ;
#70858 = EDGE_CURVE ( 'NONE', #33481, #37811, #50308, .T. ) ;
#70859 = CARTESIAN_POINT ( 'NONE',  ( 15.29254711327534899, -15.47666941828629739, -1.500000000000002220 ) ) ;
#70860 = DIRECTION ( 'NONE',  ( -1.000000000000000000, -3.773278334444166432E-23, -8.201307841325785021E-29 ) ) ;
#70861 = CARTESIAN_POINT ( 'NONE',  ( 9.421224358276909072, -17.24829524558457194, -1.500000000000002220 ) ) ;
#70862 = ADVANCED_FACE ( 'NONE', ( #32466 ), #58772, .T. ) ;
#70863 = CIRCLE ( 'NONE', #93506, 1.000000000000000444 ) ;
#70864 = CARTESIAN_POINT ( 'NONE',  ( -122.6228709571500559, -24.65952944569305316, 1.056160979905706343 ) ) ;
#70865 = EDGE_CURVE ( 'NONE', #48435, #18228, #90694, .T. ) ;
#70866 = CYLINDRICAL_SURFACE ( 'NONE', #88844, 1.000000000000000444 ) ;
#70867 = DATE_AND_TIME ( #78451, #44266 ) ;
#70868 = CARTESIAN_POINT ( 'NONE',  ( -38.52287095715006870, -23.47596703998600631, 11.44779298504229281 ) ) ;
#70869 = CARTESIAN_POINT ( 'NONE',  ( 2.591664760199015927, -6.376774720514417183, 20.15921530338947321 ) ) ;
#70870 = CARTESIAN_POINT ( 'NONE',  ( -20.44794078217315558, 2.270689272194197805, 11.49999999999999645 ) ) ;
#70871 = CARTESIAN_POINT ( 'NONE',  ( 4.518955212990007908, -6.376774720514422512, 20.94857968174986951 ) ) ;
#70872 = VECTOR ( 'NONE', #89979, 1000.000000000000114 ) ;
#70873 = CARTESIAN_POINT ( 'NONE',  ( -120.5892038963322079, -24.63355581998386157, 0.9682620441943888823 ) ) ;
#70874 = CARTESIAN_POINT ( 'NONE',  ( -21.91535228782390732, -5.629186751109307885, 11.49999999999999645 ) ) ;
#70875 = EDGE_LOOP ( 'NONE', ( #92586, #80587, #1479, #22718, #89406, #30010, #95143, #26215, #65726 ) ) ;
#70876 = CARTESIAN_POINT ( 'NONE',  ( -80.64675904551154417, -25.21083105912962807, 3.409327675794629808 ) ) ;
#70877 = DIRECTION ( 'NONE',  ( -3.773278334453079618E-23, 0.9999999999976377785, 2.173523156925979975E-06 ) ) ;
#70878 = CARTESIAN_POINT ( 'NONE',  ( -74.52287095715006160, -24.33927499327854349, 9.819080762295802955 ) ) ;
#70879 = CARTESIAN_POINT ( 'NONE',  ( 22.02124265030973760, -4.543225279485573864, 16.20402280011862217 ) ) ;
#70880 = AXIS2_PLACEMENT_3D ( 'NONE', #49123, #20021, #78532 ) ;
#70881 = ADVANCED_FACE ( 'NONE', ( #32976, #31968 ), #97659, .T. ) ;
#70882 = CARTESIAN_POINT ( 'NONE',  ( -25.96779814532654385, -24.93063398007822684, 7.161765927771289064 ) ) ;
#70883 = DIRECTION ( 'NONE',  ( -3.773278334444166432E-23, 1.000000000000000000, 0.000000000000000000 ) ) ;
#70884 = EDGE_LOOP ( 'NONE', ( #54935, #58880, #48112, #26702 ) ) ;
#70885 = EDGE_CURVE ( 'NONE', #53709, #15278, #28544, .T. ) ;
#70886 = CARTESIAN_POINT ( 'NONE',  ( -79.34687923781920915, -25.26750092165967132, 5.960409283396633562 ) ) ;
#70887 = CARTESIAN_POINT ( 'NONE',  ( 7.824713763024562674, 21.46283361357968289, 11.49999999999998934 ) ) ;
#70888 = CARTESIAN_POINT ( 'NONE',  ( -104.5228709571501184, -23.94994826722565762, -0.6494450866342743600 ) ) ;
#70889 = CARTESIAN_POINT ( 'NONE',  ( -96.59382161140817402, -23.96119346886881019, -0.6495511937832062488 ) ) ;
#70890 = CARTESIAN_POINT ( 'NONE',  ( -63.53555138627451981, -24.66019654487200086, 8.947790411086119278 ) ) ;
#70891 = CARTESIAN_POINT ( 'NONE',  ( 15.63351008929417318, -16.12541905121107177, 11.49999999999999645 ) ) ;
#70892 = ORIENTED_EDGE ( 'NONE', *, *, #88853, .T. ) ;
#70893 = CARTESIAN_POINT ( 'NONE',  ( -34.62287095715006302, -23.72773821059535493, 11.05748984161097681 ) ) ;
#70894 = CARTESIAN_POINT ( 'NONE',  ( -21.90371867972833542, 1.011951690471867060, -1.500000000000002220 ) ) ;
#70895 = CARTESIAN_POINT ( 'NONE',  ( -5.378122165843598701, -5.876774720514410077, 19.21968329462762526 ) ) ;
#70896 = CARTESIAN_POINT ( 'NONE',  ( -44.54009632154533449, -24.35071581493543036, 9.817618358456025263 ) ) ;
#70897 = CARTESIAN_POINT ( 'NONE',  ( -69.11640284054173833, -25.15929664862683879, 6.884326848992852632 ) ) ;
#70898 = ORIENTED_EDGE ( 'NONE', *, *, #55967, .T. ) ;
#70899 = CARTESIAN_POINT ( 'NONE',  ( -48.60674490981843121, -23.73791477778911840, 11.05961554403170766 ) ) ;
#70900 = CARTESIAN_POINT ( 'NONE',  ( -89.40841769935767047, -29.50249591506787894, 5.947779886229223045 ) ) ;
#70901 = ORIENTED_EDGE ( 'NONE', *, *, #61355, .F. ) ;
#70902 = CARTESIAN_POINT ( 'NONE',  ( -20.16212974941129588, 3.559051167911782887, 11.49999999999998934 ) ) ;
#70903 = ORIENTED_EDGE ( 'NONE', *, *, #49631, .F. ) ;
#70904 = ORIENTED_EDGE ( 'NONE', *, *, #44919, .T. ) ;
#70905 = VERTEX_POINT ( 'NONE', #33969 ) ;
#70906 = ORIENTED_EDGE ( 'NONE', *, *, #81323, .T. ) ;
#70907 = CARTESIAN_POINT ( 'NONE',  ( -13.16640216892762894, -18.94680327863774849, 11.49999999999998934 ) ) ;
#70908 = CARTESIAN_POINT ( 'NONE',  ( 10.75273025779354263, -6.376774720514426953, 16.96478738960562893 ) ) ;
#70909 = CARTESIAN_POINT ( 'NONE',  ( -20.32193514540556123, 0.06534614623005505218, -1.500000000000002220 ) ) ;
#70910 = EDGE_LOOP ( 'NONE', ( #10878, #34752, #8109 ) ) ;
#70911 = VECTOR ( 'NONE', #91268, 1000.000000000000000 ) ;
#70912 = LINE ( 'NONE', #891, #21753 ) ;
#70913 = CARTESIAN_POINT ( 'NONE',  ( -92.50481889294847804, -24.65952944569304961, 1.056160979905703901 ) ) ;
#70914 = EDGE_CURVE ( 'NONE', #46454, #81148, #43585, .T. ) ;
#70915 = DIRECTION ( 'NONE',  ( -0.000000000000000000, 2.173523156925979552E-06, -0.9999999999976378895 ) ) ;
#70916 = CARTESIAN_POINT ( 'NONE',  ( 4.647383884978952828, -5.876774720514412742, 19.72975307774251164 ) ) ;
#70918 = ORIENTED_EDGE ( 'NONE', *, *, #48369, .F. ) ;
#70917 = CARTESIAN_POINT ( 'NONE',  ( -20.86232423683148340, -5.086641213604358391, 11.49999999999999645 ) ) ;
#70919 = DIRECTION ( 'NONE',  ( -0.000000000000000000, -0.000000000000000000, -1.000000000000000000 ) ) ;
#70920 = CARTESIAN_POINT ( 'NONE',  ( -104.6228709571500559, -23.72747288104442021, -1.053458166803661999 ) ) ;
#70921 = VERTEX_POINT ( 'NONE', #95865 ) ;
#70922 = AXIS2_PLACEMENT_3D ( 'NONE', #75190, #5684, #50380 ) ;
#70923 = CARTESIAN_POINT ( 'NONE',  ( 19.40724743217988291, -7.346346906864608783, -1.500000000000002220 ) ) ;
#70924 = EDGE_CURVE ( 'NONE', #80790, #86594, #89258, .T. ) ;
#70925 = ORIENTED_EDGE ( 'NONE', *, *, #35012, .T. ) ;
#70927 = ORIENTED_EDGE ( 'NONE', *, *, #4999, .F. ) ;
#70926 = CARTESIAN_POINT ( 'NONE',  ( -78.52287095715006160, -29.50247984919015209, -1.443849546365053582 ) ) ;
#70928 = B_SPLINE_SURFACE_WITH_KNOTS ( 'NONE', 3, 1, ( 
 ( #12348, #2763 ),
 ( #74258, #96105 ),
 ( #4750, #35703 ),
 ( #57056, #18470 ),
 ( #64680, #11855 ),
 ( #96591, #28089 ),
 ( #95597, #26084 ),
 ( #87991, #66678 ),
 ( #27089, #10865 ),
 ( #34209, #88991 ),
 ( #41830, #88492 ),
 ( #58057, #80876 ),
 ( #18969, #49946 ),
 ( #35205, #66176 ),
 ( #27593, #58544 ),
 ( #89483, #19961 ),
 ( #91969, #37190 ),
 ( #82856, #5738 ),
 ( #74745, #44319 ) ),
 .UNSPECIFIED., .F., .F., .F.,
 ( 4, 1, 1, 1, 1, 1, 1, 1, 1, 1, 1, 1, 1, 1, 1, 1, 4 ),
 ( 2, 2 ),
 ( 0.000000000000000000, 0.07271299661694095862, 0.1415474849795007595, 0.2083625229559549763, 0.2724615839557062436, 0.3353899614876877933, 0.3977112986796186300, 0.4593833749474410810, 0.5220981738873415878, 0.5843147667471931817, 0.6443919352300537806, 0.7033450132947852707, 0.7615088749701885984, 0.8200304749172312446, 0.8785170367552999071, 0.9382645014876742628, 1.000000000000000000 ),
 ( 0.000000000000000000, 1.000000000000000000 ),
 .UNSPECIFIED. ) ;
#70929 = CARTESIAN_POINT ( 'NONE',  ( -111.5570161281370076, -23.73791477778912551, 11.05961554403170055 ) ) ;
#70930 = CARTESIAN_POINT ( 'NONE',  ( -102.6228709571500559, -29.50248528299804818, 1.056150453629042030 ) ) ;
#70931 = ORIENTED_EDGE ( 'NONE', *, *, #66868, .T. ) ;
#70932 = ORIENTED_EDGE ( 'NONE', *, *, #64240, .F. ) ;
#70933 = DIRECTION ( 'NONE',  ( -0.4560907909095458512, 0.000000000000000000, 0.8899332505573128715 ) ) ;
#70934 = CARTESIAN_POINT ( 'NONE',  ( -42.56929197859121672, -23.48786465467240347, 11.44779295918255535 ) ) ;
#70935 = CARTESIAN_POINT ( 'NONE',  ( -43.58150547404529362, -24.51419770103157347, 9.386484678747178734 ) ) ;
#70936 = CARTESIAN_POINT ( 'NONE',  ( 19.14557405504459453, -10.84957060938160289, 11.49999999999999645 ) ) ;
#70937 = DIRECTION ( 'NONE',  ( -0.000000000000000000, 1.000000000000000000, -0.000000000000000000 ) ) ;
#70938 = CARTESIAN_POINT ( 'NONE',  ( -4.885077187424587741, 22.05487924249641551, -1.500000000000002220 ) ) ;
#70939 = AXIS2_PLACEMENT_3D ( 'NONE', #94415, #55369, #85296 ) ;
#70940 = CARTESIAN_POINT ( 'NONE',  ( -5.787726610425443674, -20.20099407548119075, 11.49999999999998934 ) ) ;
#70942 = ORIENTED_EDGE ( 'NONE', *, *, #43721, .F. ) ;
#70941 = CARTESIAN_POINT ( 'NONE',  ( -70.62287095715008434, -23.84047902841601285, -0.8780736468305809783 ) ) ;
#70943 = VERTEX_POINT ( 'NONE', #80144 ) ;
#70944 = CARTESIAN_POINT ( 'NONE',  ( 31.82032313667048484, 5.965225279485572685, 9.148483289431936782 ) ) ;
#70945 = AXIS2_PLACEMENT_3D ( 'NONE', #82870, #76251, #52941 ) ;
#70946 = CARTESIAN_POINT ( 'NONE',  ( -113.6228709571500417, -23.47596703998600631, 11.44779298504227860 ) ) ;
#70947 = ORIENTED_EDGE ( 'NONE', *, *, #81727, .F. ) ;
#70948 = CARTESIAN_POINT ( 'NONE',  ( 21.03498508994548999, -2.205306954651367946, 11.49999999999998934 ) ) ;
#70949 = CARTESIAN_POINT ( 'NONE',  ( -117.5895376238167245, -23.47593901973091235, -1.443836447538997536 ) ) ;
#70950 = CARTESIAN_POINT ( 'NONE',  ( -51.54603119510975517, -25.03148648216341954, 7.131526314890322737 ) ) ;
#70951 = CARTESIAN_POINT ( 'NONE',  ( -49.54496353273913201, -25.27887345932698082, 4.195367252302923511 ) ) ;
#70952 = VECTOR ( 'NONE', #88188, 1000.000000000000000 ) ;
#70953 = CARTESIAN_POINT ( 'NONE',  ( -79.58953762381672448, -24.64898659630528854, 1.056161002820827699 ) ) ;
#70954 = CARTESIAN_POINT ( 'NONE',  ( 3.180076745125955284, -6.376774720514426953, -28.87659520466658236 ) ) ;
#70955 = CARTESIAN_POINT ( 'NONE',  ( 16.16129659511371131, 15.28805624652528472, -1.500000000000002220 ) ) ;
#70956 = CARTESIAN_POINT ( 'NONE',  ( -49.57708068730813267, -25.03220865545371154, 7.373516867294396704 ) ) ;
#70957 = ORIENTED_EDGE ( 'NONE', *, *, #88725, .T. ) ;
#70958 = FACE_BOUND ( 'NONE', #67448, .T. ) ;
#70959 = CARTESIAN_POINT ( 'NONE',  ( -48.62287095715004881, -24.50216790748097395, 0.6166512839513694777 ) ) ;
#70960 = LINE ( 'NONE', #79054, #16070 ) ;
#70961 = FACE_OUTER_BOUND ( 'NONE', #52094, .T. ) ;
#70962 = LINE ( 'NONE', #85171, #82630 ) ;
#70963 = CARTESIAN_POINT ( 'NONE',  ( -19.06185424839875964, 3.971334347869299286, -1.500000000000002220 ) ) ;
#70964 = CARTESIAN_POINT ( 'NONE',  ( 4.431377227695222132, -20.94745169971119481, 11.49999999999998934 ) ) ;
#70965 = LINE ( 'NONE', #63371, #9361 ) ;
#70966 = CARTESIAN_POINT ( 'NONE',  ( -60.48283693452195564, -24.92592662360294042, 8.075495902990192931 ) ) ;
#70967 = CARTESIAN_POINT ( 'NONE',  ( -51.55336426161518659, -23.96119346886880663, -0.6495511937832119109 ) ) ;
#70968 = CARTESIAN_POINT ( 'NONE',  ( -121.6228709571500417, -29.50248528299804818, 1.056150453629045360 ) ) ;
#70969 = CARTESIAN_POINT ( 'NONE',  ( 6.262736145392394427, -21.83385498489561272, -1.500000000000002220 ) ) ;
#70970 = EDGE_CURVE ( 'NONE', #75118, #84956, #57332, .T. ) ;
#70971 = CARTESIAN_POINT ( 'NONE',  ( -98.56082856698625960, -23.48783264082476663, -1.443836473390090136 ) ) ;
#70972 = CARTESIAN_POINT ( 'NONE',  ( -0.02075734969026423599, 3.316774720514426456, -29.05397719988137339 ) ) ;
#70973 = CARTESIAN_POINT ( 'NONE',  ( -13.56193660873917395, -14.51407242162769151, 11.49999999999999645 ) ) ;
#70974 = CARTESIAN_POINT ( 'NONE',  ( -84.52287095715001897, -23.73907113216987952, -1.053371485793251461 ) ) ;
#70975 = EDGE_CURVE ( 'NONE', #55815, #64204, #50698, .T. ) ;
#70976 = CARTESIAN_POINT ( 'NONE',  ( 8.940588884021771321, 1.075525492964989691E-15, 3.692441190372578674 ) ) ;
#70977 = DIRECTION ( 'NONE',  ( -3.773278334453079030E-23, 0.9999999999976377785, 2.173523156925979128E-06 ) ) ;
#70978 = ORIENTED_EDGE ( 'NONE', *, *, #47678, .T. ) ;
#70979 = LINE ( 'NONE', #31406, #10505 ) ;
#70980 = CARTESIAN_POINT ( 'NONE',  ( -6.720452724358975338, -6.376774720514411854, 19.46153846153846700 ) ) ;
#70981 = EDGE_CURVE ( 'NONE', #85384, #17017, #10634, .T. ) ;
#70982 = CARTESIAN_POINT ( 'NONE',  ( -71.52287095715007581, -24.50321055353805733, 9.387540953477515160 ) ) ;
#70983 = CARTESIAN_POINT ( 'NONE',  ( -6.031157642910047301, -20.80930661755759203, 11.49999999999998934 ) ) ;
#70984 = VECTOR ( 'NONE', #51101, 1000.000000000000000 ) ;
#70985 = CARTESIAN_POINT ( 'NONE',  ( -12.65407072091356433, -5.965225279485572685, -26.15404995688568590 ) ) ;
#70986 = CARTESIAN_POINT ( 'NONE',  ( 2.628080361126900133, -19.32819128710564272, -1.500000000000002220 ) ) ;
#70987 = EDGE_CURVE ( 'NONE', #75990, #57247, #73046, .T. ) ;
#70988 = CARTESIAN_POINT ( 'NONE',  ( -55.48558124947912518, -24.73531770709095312, 8.716586749053510275 ) ) ;
#70989 = ORIENTED_EDGE ( 'NONE', *, *, #41828, .T. ) ;
#70990 = ADVANCED_FACE ( 'NONE', ( #74035 ), #34474, .T. ) ;
#70991 = CARTESIAN_POINT ( 'NONE',  ( 8.549789220347504326, 18.50885834720105905, 11.49999999999999645 ) ) ;
#70992 = FACE_OUTER_BOUND ( 'NONE', #7484, .T. ) ;
#70993 = EDGE_CURVE ( 'NONE', #82766, #2872, #15251, .T. ) ;
#70994 = CARTESIAN_POINT ( 'NONE',  ( 13.74975846015576586, 6.475225279485573360, -27.72022515045486557 ) ) ;
#70995 = VERTEX_POINT ( 'NONE', #65450 ) ;
#70996 = CARTESIAN_POINT ( 'NONE',  ( -34.52287095715006160, -29.50250786944525672, 11.44777988621624409 ) ) ;
#70997 = PLANE ( 'NONE',  #60670 ) ;
#70998 = CARTESIAN_POINT ( 'NONE',  ( -75.58953762381673869, -23.47596703998600276, 11.44779298504227683 ) ) ;
#70999 = DIRECTION ( 'NONE',  ( 0.000000000000000000, -0.000000000000000000, -1.000000000000000000 ) ) ;
#71000 = DIRECTION ( 'NONE',  ( -3.773278334444167608E-23, 1.000000000000000000, 0.000000000000000000 ) ) ;
#71001 = CARTESIAN_POINT ( 'NONE',  ( 14.11618873683251252, 14.29484301466228047, 11.49999999999998934 ) ) ;
#71002 = B_SPLINE_CURVE_WITH_KNOTS ( 'NONE', 3,
 ( #33175, #16950, #95080, #71752 ),
 .UNSPECIFIED., .F., .F.,
 ( 4, 4 ),
 ( 0.1806289827352041688, 0.1896354140073194250 ),
 .UNSPECIFIED. ) ;
#71003 = CARTESIAN_POINT ( 'NONE',  ( -57.52287095715008292, -23.47593901973090524, -1.443836447538997092 ) ) ;
#71004 = ORIENTED_EDGE ( 'NONE', *, *, #90712, .F. ) ;
#71005 = CARTESIAN_POINT ( 'NONE',  ( 10.86264265030973952, 0.3587747205144257157, -28.64597719988137570 ) ) ;
#71006 = VECTOR ( 'NONE', #64258, 1000.000000000000000 ) ;
#71007 = CARTESIAN_POINT ( 'NONE',  ( -14.98413761715186077, 17.36544542080599740, 11.49999999999999645 ) ) ;
#71008 = CARTESIAN_POINT ( 'NONE',  ( -0.6305239314742796530, -22.70799625201654592, 11.49999999999998934 ) ) ;
#71009 = ORIENTED_EDGE ( 'NONE', *, *, #87243, .F. ) ;
#71010 = PLANE ( 'NONE',  #35656 ) ;
#71011 = DIRECTION ( 'NONE',  ( 0.000000000000000000, 0.000000000000000000, 1.000000000000000000 ) ) ;
#71012 = CARTESIAN_POINT ( 'NONE',  ( -38.64869433578421365, -23.96169478059712432, 10.65365249895718591 ) ) ;
#71013 = CARTESIAN_POINT ( 'NONE',  ( -49.52287095715006160, -24.65952944569304606, 1.056160979905693686 ) ) ;
#71014 = TOROIDAL_SURFACE ( 'NONE', #22375, 25.90800000000000125, 2.040000000000000036 ) ;
#71015 = CARTESIAN_POINT ( 'NONE',  ( -4.209565145052936330, 8.865772972990910716, -1.700000000000008837 ) ) ;
#71016 = CARTESIAN_POINT ( 'NONE',  ( -49.20471335217622055, -25.31215404449747908, 5.309145496855610880 ) ) ;
#71017 = CARTESIAN_POINT ( 'NONE',  ( -76.62287095715007013, -23.73934037231757443, 11.05740245334329153 ) ) ;
#71018 = CARTESIAN_POINT ( 'NONE',  ( -98.90869474253671001, -25.25460678994682340, 5.895134505904293221 ) ) ;
#71019 = ORIENTED_EDGE ( 'NONE', *, *, #30298, .F. ) ;
#71020 = AXIS2_PLACEMENT_3D ( 'NONE', #339, #54640, #86076 ) ;
#71021 = CARTESIAN_POINT ( 'NONE',  ( -10.90597124047809530, 17.21661415904998904, -1.500000000000002220 ) ) ;
#71022 = ORIENTED_EDGE ( 'NONE', *, *, #76619, .T. ) ;
#71023 = CARTESIAN_POINT ( 'NONE',  ( -12.88233675513024856, -19.01995677650982230, -1.500000000000002220 ) ) ;
#71024 = CARTESIAN_POINT ( 'NONE',  ( -7.188523146553190912, -5.876774720514413630, 19.66116880005639800 ) ) ;
#71025 = ORIENTED_EDGE ( 'NONE', *, *, #38769, .F. ) ;
#71026 = CARTESIAN_POINT ( 'NONE',  ( -114.5228709571500190, -24.66019654487200441, 8.947790411086110396 ) ) ;
#71027 = CARTESIAN_POINT ( 'NONE',  ( -101.5228709571500758, -23.47593901973090524, -1.443836447538996426 ) ) ;
#71028 = DIRECTION ( 'NONE',  ( 2.338552693767719605E-15, 0.000000000000000000, 1.000000000000000000 ) ) ;
#71029 = AXIS2_PLACEMENT_3D ( 'NONE', #90826, #21300, #12193 ) ;
#71031 = EDGE_LOOP ( 'NONE', ( #12457, #1494, #96480, #97532 ) ) ;
#71030 = CARTESIAN_POINT ( 'NONE',  ( -1.825377252022436281, -21.23478267787193730, 11.49999999999999645 ) ) ;
#71032 = ORIENTED_EDGE ( 'NONE', *, *, #73194, .T. ) ;
#71033 = CARTESIAN_POINT ( 'NONE',  ( -19.03210976516136554, 11.49075778266564107, -1.500000000000002220 ) ) ;
#71034 = CARTESIAN_POINT ( 'NONE',  ( -14.43086120294938368, -14.79396848081076854, -1.500000000000002220 ) ) ;
#71035 = EDGE_CURVE ( 'NONE', #95160, #12369, #13614, .T. ) ;
#71036 = EDGE_LOOP ( 'NONE', ( #43218, #17217, #91514, #21826 ) ) ;
#71037 = CARTESIAN_POINT ( 'NONE',  ( -6.265203266387573855, -5.876774720514408301, 19.29154511076646017 ) ) ;
#71038 = EDGE_CURVE ( 'NONE', #43355, #8583, #5549, .T. ) ;
#71039 = CARTESIAN_POINT ( 'NONE',  ( -95.54220200439495159, -25.00182538069147142, 7.747789668545043362 ) ) ;
#71040 = ORIENTED_EDGE ( 'NONE', *, *, #20328, .F. ) ;
#71041 = CARTESIAN_POINT ( 'NONE',  ( -79.62287095715005592, -23.48786465467241058, 11.44779295918254469 ) ) ;
#71042 = ORIENTED_EDGE ( 'NONE', *, *, #68220, .T. ) ;
#71043 = CARTESIAN_POINT ( 'NONE',  ( 8.026968004785691946, -3.316774720514427344, -28.15626605682496830 ) ) ;
#71044 = CARTESIAN_POINT ( 'NONE',  ( -70.62963902551980766, -25.12997664719427959, 7.061473379948721707 ) ) ;
#71045 = CARTESIAN_POINT ( 'NONE',  ( 19.40856703110355852, -7.758221025823637262, -1.500000000000002220 ) ) ;
#71046 = CARTESIAN_POINT ( 'NONE',  ( -1.678574117887026373, -21.80011532881206548, 11.49999999999999645 ) ) ;
#71047 = CARTESIAN_POINT ( 'NONE',  ( 25.72842579859213430, -5.175431684531299759, -7.741149173772083003 ) ) ;
#71048 = FACE_OUTER_BOUND ( 'NONE', #78858, .T. ) ;
#71049 = CARTESIAN_POINT ( 'NONE',  ( 14.32739804834607256, 17.34395043298086847, -1.500000000000002220 ) ) ;
#71050 = CARTESIAN_POINT ( 'NONE',  ( -118.5546831409418616, -24.15620529776628800, 10.23563542870659759 ) ) ;
#71051 = B_SPLINE_CURVE_WITH_KNOTS ( 'NONE', 3,
 ( #10688, #71594, #32016, #94416 ),
 .UNSPECIFIED., .F., .F.,
 ( 4, 4 ),
 ( 0.3700501682448147367, 0.3790565995169303259 ),
 .UNSPECIFIED. ) ;
#71052 = CARTESIAN_POINT ( 'NONE',  ( -57.62287095715004881, -24.64898659630367916, 1.056161002820822592 ) ) ;
#71053 = CARTESIAN_POINT ( 'NONE',  ( -78.52287095715004739, -23.48783264082476308, -1.443836473390091468 ) ) ;
#71054 = VERTEX_POINT ( 'NONE', #52198 ) ;
#71055 = B_SPLINE_SURFACE_WITH_KNOTS ( 'NONE', 3, 3, ( 
 ( #42785, #51889, #73717, #27555 ),
 ( #75206, #4212, #51384, #82816 ),
 ( #82325, #29527, #67616, #6694 ),
 ( #60008, #37648, #91931, #84315 ),
 ( #46769, #99031, #83315, #13798 ),
 ( #100018, #98534, #14797, #76198 ),
 ( #30025, #54384, #91423, #68603 ),
 ( #45763, #45271, #36651, #23398 ),
 ( #29030, #85313, #99527, #76686 ),
 ( #21406, #52382, #15300, #31030 ) ),
 .UNSPECIFIED., .F., .F., .F.,
 ( 4, 3, 3, 4 ),
 ( 4, 4 ),
 ( 0.0004766839783813280377, 0.1491231665100169190, 0.2234464077758346878, 0.2977696490416524844 ),
 ( 0.7495845312173156083, 0.7510439293833934826 ),
 .UNSPECIFIED. ) ;
#71056 = ORIENTED_EDGE ( 'NONE', *, *, #59514, .T. ) ;
#71057 = ORIENTED_EDGE ( 'NONE', *, *, #42014, .F. ) ;
#71058 = CARTESIAN_POINT ( 'NONE',  ( 30.53060340732036337, -5.297812262124697469, 1.539714685317310483 ) ) ;
#71060 = EDGE_CURVE ( 'NONE', #10358, #80526, #44584, .T. ) ;
#71059 = CC_DESIGN_DATE_AND_TIME_ASSIGNMENT ( #29793, #82088, ( #78282 ) ) ;
#71061 = VERTEX_POINT ( 'NONE', #6011 ) ;
#71062 = CARTESIAN_POINT ( 'NONE',  ( -7.638042729800005759, 19.97414216180626667, -1.500000000000002220 ) ) ;
#71063 = CARTESIAN_POINT ( 'NONE',  ( 21.65046080595755740, -5.567969076317650590, 11.49999999999999645 ) ) ;
#71064 = ORIENTED_EDGE ( 'NONE', *, *, #6793, .T. ) ;
#71065 = DIRECTION ( 'NONE',  ( -3.773278334444167608E-23, 1.000000000000000000, 0.000000000000000000 ) ) ;
#71066 = CARTESIAN_POINT ( 'NONE',  ( -1.165634184549018126, -21.02984315360824752, -1.500000000000002220 ) ) ;
#71067 = CARTESIAN_POINT ( 'NONE',  ( -30.54633378701636559, -24.57840743580478104, 9.174392229302920754 ) ) ;
#71068 = CARTESIAN_POINT ( 'NONE',  ( -19.95764006394758638, 0.7380318605572177004, -1.500000000000002220 ) ) ;
#71069 = CARTESIAN_POINT ( 'NONE',  ( -114.6228709571500417, -23.48786465467241769, 11.44779295918253936 ) ) ;
#71070 = CARTESIAN_POINT ( 'NONE',  ( 2.955024617976266033, -6.376774720514415407, 20.58370193283586858 ) ) ;
#71071 = CARTESIAN_POINT ( 'NONE',  ( -14.32918165687622825, -16.72005635474405949, -1.500000000000002220 ) ) ;
#71072 = FACE_OUTER_BOUND ( 'NONE', #5391, .T. ) ;
#71073 = ORIENTED_EDGE ( 'NONE', *, *, #26054, .F. ) ;
#71074 = CARTESIAN_POINT ( 'NONE',  ( -65.53038835011091123, -25.00182538069146432, 7.747789668545041586 ) ) ;
#71075 = CARTESIAN_POINT ( 'NONE',  ( 32.16024265030974050, -5.965225279485572685, 16.27760796525321751 ) ) ;
#71076 = CARTESIAN_POINT ( 'NONE',  ( 12.78316523911058944, -16.47895720935621711, 11.49999999999999645 ) ) ;
#71077 = VECTOR ( 'NONE', #42050, 1000.000000000000114 ) ;
#71078 = CARTESIAN_POINT ( 'NONE',  ( -74.55620429048340725, -24.65952944569304606, 1.056160979905698571 ) ) ;
#71079 = CARTESIAN_POINT ( 'NONE',  ( -108.6228709571500559, -23.73934037231757799, 11.05740245334328087 ) ) ;
#71080 = FACE_OUTER_BOUND ( 'NONE', #94017, .T. ) ;
#71081 = CARTESIAN_POINT ( 'NONE',  ( -10.68834330497911189, 18.46263264838738039, -1.500000000000002220 ) ) ;
#71082 = CARTESIAN_POINT ( 'NONE',  ( -10.34999999999999254, 4.999999999999999112, 2.100000000000000089 ) ) ;
#71083 = CARTESIAN_POINT ( 'NONE',  ( -50.66585102988210565, -25.19861947315626693, 3.319393630720075095 ) ) ;
#71084 = CARTESIAN_POINT ( 'NONE',  ( -0.4362980769230789257, -5.876774720514411854, 19.46153846153846345 ) ) ;
#71085 = CARTESIAN_POINT ( 'NONE',  ( -24.90875734969025501, 5.965225279485572685, 30.51402280011862089 ) ) ;
#71086 = CARTESIAN_POINT ( 'NONE',  ( 16.80569330386292748, 14.95695114220347932, -1.500000000000002220 ) ) ;
#71088 = DIRECTION ( 'NONE',  ( 0.000000000000000000, 0.000000000000000000, 1.000000000000000000 ) ) ;
#71087 = B_SPLINE_CURVE_WITH_KNOTS ( 'NONE', 3,
 ( #58350, #12650, #89285, #96395, #50728, #35990 ),
 .UNSPECIFIED., .F., .F.,
 ( 4, 2, 4 ),
 ( 1.570755371633836552E-05, 0.001396183895866086018, 0.002776660238015833410 ),
 .UNSPECIFIED. ) ;
#71089 = EDGE_LOOP ( 'NONE', ( #63808, #87948, #8532, #51477 ) ) ;
#71090 = PLANE ( 'NONE',  #96854 ) ;
#71091 = CARTESIAN_POINT ( 'NONE',  ( 8.063330319165388005, -10.15233964170352898, 1.310587897985993955 ) ) ;
#71092 = CARTESIAN_POINT ( 'NONE',  ( 5.239555828037883778, -18.94419173073049478, 11.49999999999999645 ) ) ;
#71093 = PLANE ( 'NONE',  #52095 ) ;
#71094 = B_SPLINE_CURVE_WITH_KNOTS ( 'NONE', 3,
 ( #87845, #27941, #88854, #72132, #18330, #19319 ),
 .UNSPECIFIED., .F., .F.,
 ( 4, 2, 4 ),
 ( 0.000000000000000000, 0.001380901958385385509, 0.002761803916770771018 ),
 .UNSPECIFIED. ) ;
#71095 = VECTOR ( 'NONE', #86711, 1000.000000000000227 ) ;
#71096 = CARTESIAN_POINT ( 'NONE',  ( -119.5228709571500900, -23.72773821059536914, 11.05748984161097326 ) ) ;
#71097 = EDGE_LOOP ( 'NONE', ( #12641, #99462, #10110, #43456 ) ) ;
#71098 = CARTESIAN_POINT ( 'NONE',  ( -99.50979288673286760, -24.51314013834316796, 0.6176544820404243907 ) ) ;
#71099 = CARTESIAN_POINT ( 'NONE',  ( -99.58953762381672448, -24.66019654487198665, 8.947790411086137041 ) ) ;
#71100 = EDGE_CURVE ( 'NONE', #13448, #56620, #75013, .T. ) ;
#71101 = CARTESIAN_POINT ( 'NONE',  ( -105.5228709571500758, -25.00182538069145366, 7.747789668545101094 ) ) ;
#71102 = DIRECTION ( 'NONE',  ( -1.000000000000000000, 0.000000000000000000, -0.000000000000000000 ) ) ;
#71103 = CARTESIAN_POINT ( 'NONE',  ( -5.448126336921106372, -18.99418723138115084, -1.500000000000002220 ) ) ;
#71104 = VERTEX_POINT ( 'NONE', #75512 ) ;
#71105 = EDGE_CURVE ( 'NONE', #58964, #92752, #99353, .T. ) ;
#71106 = CARTESIAN_POINT ( 'NONE',  ( 4.066846734877469949, -19.79409818376439389, 11.49999999999999645 ) ) ;
#71107 = CARTESIAN_POINT ( 'NONE',  ( 5.993553214355093139, -5.876774720514417183, 20.20316077874593930 ) ) ;
#71108 = ADVANCED_FACE ( 'NONE', ( #36965 ), #82272, .T. ) ;
#71109 = ORIENTED_EDGE ( 'NONE', *, *, #20213, .T. ) ;
#71110 = CARTESIAN_POINT ( 'NONE',  ( -48.62287095715007723, -23.95044443724991012, 10.65354141964650125 ) ) ;
#71111 = DIRECTION ( 'NONE',  ( -0.000000000000000000, 0.000000000000000000, -1.000000000000000000 ) ) ;
#71112 = CARTESIAN_POINT ( 'NONE',  ( -50.37830952628070946, -25.30401792888237367, 5.197789011716579033 ) ) ;
#71113 = CARTESIAN_POINT ( 'NONE',  ( 32.06540688909004189, -1.682774720514426114, -12.44045471929205249 ) ) ;
#71114 = CARTESIAN_POINT ( 'NONE',  ( -129.6228709571500417, -29.50248528299804818, 1.056150453629047137 ) ) ;
#71115 = CARTESIAN_POINT ( 'NONE',  ( -107.5489772126510530, -24.65952944569305316, 1.056160979905704789 ) ) ;
#71116 = CARTESIAN_POINT ( 'NONE',  ( -19.89792590360708147, -2.209704250470923892, -1.500000000000002220 ) ) ;
#71117 = EDGE_CURVE ( 'NONE', #50685, #17220, #64900, .T. ) ;
#71118 = CARTESIAN_POINT ( 'NONE',  ( -99.29064586046420970, -25.10935166775642813, 3.426411013435906039 ) ) ;
#71119 = CARTESIAN_POINT ( 'NONE',  ( -116.5525123351993955, -24.51419770103160189, 9.386484678747169852 ) ) ;
#71120 = EDGE_LOOP ( 'NONE', ( #82613, #28256, #98324, #81586 ) ) ;
#71121 = CARTESIAN_POINT ( 'NONE',  ( -79.60031018295994443, -23.73791477778911840, 11.05961554403170943 ) ) ;
#71122 = CARTESIAN_POINT ( 'NONE',  ( -109.6405337342305302, -25.29012783774154016, 3.562353256831511494 ) ) ;
#71123 = CARTESIAN_POINT ( 'NONE',  ( -35.47208223784672754, -24.83618233451450052, 1.606449574219543708 ) ) ;
#71124 = CARTESIAN_POINT ( 'NONE',  ( -48.62287095715004881, -24.64965695001467694, 8.947790433994185832 ) ) ;
#71125 = LINE ( 'NONE', #55407, #17261 ) ;
#71126 = CARTESIAN_POINT ( 'NONE',  ( -83.56309348553224936, -23.48783264082477018, -1.443836473390093689 ) ) ;
#71127 = CARTESIAN_POINT ( 'NONE',  ( -2.948852648430471124, -14.44618168209107445, 0.000000000000000000 ) ) ;
#71128 = CARTESIAN_POINT ( 'NONE',  ( -50.19347037116831700, -25.18630682891961214, 3.303495449920700544 ) ) ;
#71129 = ORIENTED_EDGE ( 'NONE', *, *, #48332, .T. ) ;
#71130 = VECTOR ( 'NONE', #27453, 1000.000000000000000 ) ;
#71131 = VECTOR ( 'NONE', #72275, 1000.000000000000114 ) ;
#71132 = CARTESIAN_POINT ( 'NONE',  ( 13.48481281434462531, 15.16087405922196041, -1.500000000000002220 ) ) ;
#71133 = DIRECTION ( 'NONE',  ( 0.000000000000000000, 0.000000000000000000, -1.000000000000000000 ) ) ;
#71134 = CARTESIAN_POINT ( 'NONE',  ( -34.58677685350260589, -24.34968618360933590, 0.1864209137778841396 ) ) ;
#71135 = VECTOR ( 'NONE', #76383, 1000.000000000000000 ) ;
#71136 = CARTESIAN_POINT ( 'NONE',  ( -59.62366543129058982, -24.66019654487199730, 8.947790411086124607 ) ) ;
#71137 = ORIENTED_EDGE ( 'NONE', *, *, #88395, .T. ) ;
#71139 = EDGE_CURVE ( 'NONE', #12619, #36399, #28856, .T. ) ;
#71138 = LINE ( 'NONE', #79235, #95538 ) ;
#71140 = CARTESIAN_POINT ( 'NONE',  ( -5.623992922573770592, 19.38241096367466199, -1.500000000000002220 ) ) ;
#71141 = CARTESIAN_POINT ( 'NONE',  ( -18.69274626484788371, 9.848020819832786543, 11.49999999999999645 ) ) ;
#71142 = VECTOR ( 'NONE', #57038, 1000.000000000000114 ) ;
#71143 = CARTESIAN_POINT ( 'NONE',  ( -13.50798789833325664, 17.53495777034937220, 11.49999999999998934 ) ) ;
#71144 = EDGE_CURVE ( 'NONE', #51587, #83112, #41879, .T. ) ;
#71145 = CARTESIAN_POINT ( 'NONE',  ( -20.42507745660439156, -2.452541965221147535, -1.500000000000002220 ) ) ;
#71146 = CARTESIAN_POINT ( 'NONE',  ( -44.62287095715004881, -29.50250243563736774, 8.947779886222148704 ) ) ;
#71147 = ORIENTED_EDGE ( 'NONE', *, *, #41956, .F. ) ;
#71148 = PLANE ( 'NONE',  #62277 ) ;
#71149 = ORIENTED_EDGE ( 'NONE', *, *, #97881, .F. ) ;
#71150 = CARTESIAN_POINT ( 'NONE',  ( 0.000000000000000000, -2.056774720514426669, 3.500000000000000000 ) ) ;
#71151 = CARTESIAN_POINT ( 'NONE',  ( -61.62287095715004881, -23.48786465467240347, 11.44779295918254824 ) ) ;
#71152 = VERTEX_POINT ( 'NONE', #84133 ) ;
#71153 = ORIENTED_EDGE ( 'NONE', *, *, #51906, .T. ) ;
#71154 = VECTOR ( 'NONE', #30317, 1000.000000000000114 ) ;
#71155 = ORIENTED_EDGE ( 'NONE', *, *, #56177, .F. ) ;
#71156 = CARTESIAN_POINT ( 'NONE',  ( -47.52287095715006160, -23.47596703998600631, 11.44779298504229104 ) ) ;
#71157 = CARTESIAN_POINT ( 'NONE',  ( 7.087697398486194622, -6.376774720514418959, 20.45710073441444621 ) ) ;
#71158 = CARTESIAN_POINT ( 'NONE',  ( 5.344006250707635353, -6.376774720514418959, 20.55781796641452885 ) ) ;
#71159 = CARTESIAN_POINT ( 'NONE',  ( 16.58470376584361361, 12.37529123428901556, -1.500000000000002220 ) ) ;
#71160 = CARTESIAN_POINT ( 'NONE',  ( 16.85579979752674618, 13.57973486276658903, 11.49999999999999645 ) ) ;
#71161 = ORIENTED_EDGE ( 'NONE', *, *, #3086, .F. ) ;
#71162 = CARTESIAN_POINT ( 'NONE',  ( -99.16166289166535819, -25.30166215957521914, 5.311370747606397380 ) ) ;
#71163 = CARTESIAN_POINT ( 'NONE',  ( -110.3139465455115129, -25.11033443737754212, 2.832404817301930056 ) ) ;
#71164 = CARTESIAN_POINT ( 'NONE',  ( 20.53814608839396527, -8.957171556794316203, 11.49999999999998934 ) ) ;
#71165 = CARTESIAN_POINT ( 'NONE',  ( -79.36551648466291908, -25.27874893558202984, 6.194053881209717893 ) ) ;
#71166 = CARTESIAN_POINT ( 'NONE',  ( -53.52287095715006160, -24.50216790748205042, 0.6166512839542438451 ) ) ;
#71167 = ORIENTED_EDGE ( 'NONE', *, *, #78387, .T. ) ;
#71168 = CARTESIAN_POINT ( 'NONE',  ( 29.62646972375975096, 5.339663449004302009, 28.46301402826327731 ) ) ;
#71169 = CARTESIAN_POINT ( 'NONE',  ( -76.62287095715007013, -23.72773821059535848, 11.05748984161097681 ) ) ;
#71170 = B_SPLINE_CURVE_WITH_KNOTS ( 'NONE', 3,
 ( #39168, #40685, #78711, #609 ),
 .UNSPECIFIED., .F., .F.,
 ( 4, 4 ),
 ( 0.8403860235663986877, 0.8493924548385139994 ),
 .UNSPECIFIED. ) ;
#71171 = ORIENTED_EDGE ( 'NONE', *, *, #82475, .F. ) ;
#71172 = VERTEX_POINT ( 'NONE', #99841 ) ;
#71173 = CARTESIAN_POINT ( 'NONE',  ( -70.58953762381671027, -23.48783264082478084, -1.443836473390067265 ) ) ;
#71174 = CC_DESIGN_PERSON_AND_ORGANIZATION_ASSIGNMENT ( #96672, #27172, ( #48909 ) ) ;
#71175 = ORIENTED_EDGE ( 'NONE', *, *, #10843, .F. ) ;
#71176 = AXIS2_PLACEMENT_3D ( 'NONE', #47012, #85561, #16044 ) ;
#71177 = CARTESIAN_POINT ( 'NONE',  ( -108.2228709571500644, -23.47593901973090169, -1.443836447538996648 ) ) ;
#71178 = CARTESIAN_POINT ( 'NONE',  ( 17.84191302092929021, 11.53353326677314961, -1.500000000000002220 ) ) ;
#71179 = ORIENTED_EDGE ( 'NONE', *, *, #28565, .T. ) ;
#71180 = DIRECTION ( 'NONE',  ( -3.773278334453079030E-23, 0.9999999999976377785, 2.173523156925979128E-06 ) ) ;
#71181 = CARTESIAN_POINT ( 'NONE',  ( -1.534710021792092594, -21.76038796025502009, -1.500000000000002220 ) ) ;
#71182 = CARTESIAN_POINT ( 'NONE',  ( -52.63305254789141685, -24.35071581493542681, 9.817618358456035921 ) ) ;
#71183 = CARTESIAN_POINT ( 'NONE',  ( -63.62287095715004881, -29.50250786944525672, 11.44777988621623876 ) ) ;
#71184 = FACE_OUTER_BOUND ( 'NONE', #71774, .T. ) ;
#71185 = CARTESIAN_POINT ( 'NONE',  ( 10.97640485992876691, 18.82695874702771377, -1.500000000000002220 ) ) ;
#71186 = CARTESIAN_POINT ( 'NONE',  ( -95.52287095715001897, -23.85196035786900026, -0.8779234886475105748 ) ) ;
#71187 = VERTEX_POINT ( 'NONE', #24733 ) ;
#71188 = CARTESIAN_POINT ( 'NONE',  ( -63.62287095715004881, -24.64898659630528499, 1.056161002820822592 ) ) ;
#71189 = CARTESIAN_POINT ( 'NONE',  ( -48.87479414115020404, -25.12782512515361333, 6.180417935526588025 ) ) ;
#71190 = VERTEX_POINT ( 'NONE', #47594 ) ;
#71191 = EDGE_CURVE ( 'NONE', #21474, #29757, #100336, .T. ) ;
#71192 = VERTEX_POINT ( 'NONE', #87141 ) ;
#71193 = ORIENTED_EDGE ( 'NONE', *, *, #41778, .F. ) ;
#71194 = CARTESIAN_POINT ( 'NONE',  ( -47.62287095715004881, -29.50250786944525672, 11.44777988621624054 ) ) ;
#71195 = CARTESIAN_POINT ( 'NONE',  ( -82.50601559517893691, -24.34968618360933945, 0.1864209137778926328 ) ) ;
#71196 = CARTESIAN_POINT ( 'NONE',  ( 14.73992482348874411, 15.29747818672187165, 11.49999999999998934 ) ) ;
#71197 = CARTESIAN_POINT ( 'NONE',  ( -94.56143254526521957, -23.48783264082477018, -1.443836473390086805 ) ) ;
#71198 = CARTESIAN_POINT ( 'NONE',  ( -130.5728709571500588, -24.45056191361607389, 9.787827635114014768 ) ) ;
#71199 = CARTESIAN_POINT ( 'NONE',  ( -41.62287095715006302, -23.47593901973091235, -1.443836447539011525 ) ) ;
#71200 = CARTESIAN_POINT ( 'NONE',  ( -99.52287095715004739, -24.50216790748204687, 0.6166512839542553914 ) ) ;
#71201 = CARTESIAN_POINT ( 'NONE',  ( -1.608633542659107629, -19.34071428503001755, 11.49999999999998934 ) ) ;
#71202 = CARTESIAN_POINT ( 'NONE',  ( -107.6228709571500701, -24.65952944569304961, 1.056160979905703901 ) ) ;
#71203 = ORIENTED_EDGE ( 'NONE', *, *, #30299, .F. ) ;
#71204 = CARTESIAN_POINT ( 'NONE',  ( 15.68791110202092476, 11.56419973807686219, 11.49999999999999645 ) ) ;
#71205 = CARTESIAN_POINT ( 'NONE',  ( -5.574014511416001127, -6.376774720514415407, 20.24089781925592391 ) ) ;
#71206 = AXIS2_PLACEMENT_3D ( 'NONE', #48125, #39999, #9547 ) ;
#71207 = EDGE_CURVE ( 'NONE', #49492, #49812, #69917, .T. ) ;
#71208 = CARTESIAN_POINT ( 'NONE',  ( 31.04236049493789906, 6.475225279485573360, 19.84760796525321780 ) ) ;
#71209 = ORIENTED_EDGE ( 'NONE', *, *, #54991, .F. ) ;
#71210 = CARTESIAN_POINT ( 'NONE',  ( 4.967948717948723392, -5.876774720514415407, 20.00140224358974095 ) ) ;
#71211 = CARTESIAN_POINT ( 'NONE',  ( -89.50838371253736625, -24.34968618360934300, 0.1864209137778942982 ) ) ;
#71212 = AXIS2_PLACEMENT_3D ( 'NONE', #25097, #96612, #79388 ) ;
#71213 = CARTESIAN_POINT ( 'NONE',  ( -91.62287095715004170, -24.50321055353805733, 9.387540953477524042 ) ) ;
#71214 = CARTESIAN_POINT ( 'NONE',  ( -101.0590973978295466, -25.21362872155826551, 3.509685239648734800 ) ) ;
#71215 = CARTESIAN_POINT ( 'NONE',  ( -19.67010641940559168, 0.002901314006966619011, -1.500000000000002220 ) ) ;
#71216 = AXIS2_PLACEMENT_3D ( 'NONE', #67642, #98564, #38668 ) ;
#71217 = ORIENTED_EDGE ( 'NONE', *, *, #17399, .T. ) ;
#71218 = CARTESIAN_POINT ( 'NONE',  ( -4.019545577234938882, 21.20919285897865336, 11.49999999999998934 ) ) ;
#71219 = EDGE_CURVE ( 'NONE', #62056, #61220, #42119, .T. ) ;
#71220 = AXIS2_PLACEMENT_3D ( 'NONE', #13706, #84724, #6103 ) ;
#71221 = CARTESIAN_POINT ( 'NONE',  ( -65.62287095715005592, -25.00182538069145721, 7.747789668545100206 ) ) ;
#71222 = CARTESIAN_POINT ( 'NONE',  ( 22.95697726795019378, -2.620641032420567118, -1.500000000000002220 ) ) ;
#71223 = EDGE_CURVE ( 'NONE', #12270, #87638, #46588, .T. ) ;
#71224 = VECTOR ( 'NONE', #21610, 1000.000000000000114 ) ;
#71225 = APPROVAL_ROLE ( '' ) ;
#71226 = CARTESIAN_POINT ( 'NONE',  ( 3.165726958143470160, -6.376774720514422512, 21.14296526391294506 ) ) ;
#71227 = CARTESIAN_POINT ( 'NONE',  ( 4.127208352283176396, -6.376774720514424288, 21.39624840817692686 ) ) ;
#71228 = CARTESIAN_POINT ( 'NONE',  ( -29.52287095715007581, -24.25489487036892200, 9.819270455405353815 ) ) ;
#71229 = CARTESIAN_POINT ( 'NONE',  ( -128.6228709571500417, -23.47596703998600631, 11.44779298504227860 ) ) ;
#71230 = LINE ( 'NONE', #79327, #99195 ) ;
#71231 = CARTESIAN_POINT ( 'NONE',  ( -129.5900271110918709, -23.48783264082478084, -1.443836473390078590 ) ) ;
#71232 = CARTESIAN_POINT ( 'NONE',  ( -99.25286268653823640, -25.31566011607329258, 4.527133398161728550 ) ) ;
#71233 = CARTESIAN_POINT ( 'NONE',  ( -14.97016004668225264, 13.15154794113874637, -1.500000000000002220 ) ) ;
#71234 = ADVANCED_FACE ( 'NONE', ( #78511 ), #62318, .T. ) ;
#71235 = CARTESIAN_POINT ( 'NONE',  ( -75.53432623487223907, -25.00182538069146787, 7.747789668545045139 ) ) ;
#71236 = CARTESIAN_POINT ( 'NONE',  ( 13.50462702941046977, 14.53317887778067252, -1.500000000000002220 ) ) ;
#71237 = ORIENTED_EDGE ( 'NONE', *, *, #25480, .T. ) ;
#71238 = FACE_OUTER_BOUND ( 'NONE', #49394, .T. ) ;
#71239 = B_SPLINE_CURVE_WITH_KNOTS ( 'NONE', 3,
 ( #26566, #2735, #96560, #80849 ),
 .UNSPECIFIED., .F., .F.,
 ( 4, 4 ),
 ( 0.000000000000000000, 9.999999999997510880E-05 ),
 .UNSPECIFIED. ) ;
#71240 = CARTESIAN_POINT ( 'NONE',  ( -51.39797819248544641, -25.20552468222252074, 6.636430008107547351 ) ) ;
#71241 = FACE_OUTER_BOUND ( 'NONE', #7864, .T. ) ;
#71242 = CARTESIAN_POINT ( 'NONE',  ( -9.565632364391108311, -18.43008791299702764, 11.49999999999999645 ) ) ;
#71243 = DIRECTION ( 'NONE',  ( 1.240248834241861717E-14, 0.000000000000000000, -1.000000000000000000 ) ) ;
#71244 = CARTESIAN_POINT ( 'NONE',  ( -78.52287095715006160, -24.64965694238408034, 8.947790433994198267 ) ) ;
#71245 = CARTESIAN_POINT ( 'NONE',  ( -0.9122204482399535186, 22.77315974801211240, 11.49999999999999645 ) ) ;
#71246 = VERTEX_POINT ( 'NONE', #16122 ) ;
#71247 = CARTESIAN_POINT ( 'NONE',  ( -69.52210430107112415, -23.48783264082476308, -1.443836473390097908 ) ) ;
#71248 = DIRECTION ( 'NONE',  ( 0.000000000000000000, -2.173523156925980399E-06, 0.9999999999976378895 ) ) ;
#71249 = ORIENTED_EDGE ( 'NONE', *, *, #4542, .T. ) ;
#71250 = CARTESIAN_POINT ( 'NONE',  ( -9.470923242388245455, -17.85692771776473364, 11.49999999999998934 ) ) ;
#71251 = CARTESIAN_POINT ( 'NONE',  ( 0.000000000000000000, 0.3850000000000053935, -1.529999999999998916 ) ) ;
#71252 = CARTESIAN_POINT ( 'NONE',  ( -108.6228709571500417, -24.66019654487199730, 8.947790411086124607 ) ) ;
#71253 = EDGE_LOOP ( 'NONE', ( #79667, #81921, #97620, #5275 ) ) ;
#71254 = FACE_OUTER_BOUND ( 'NONE', #84030, .T. ) ;
#71255 = CARTESIAN_POINT ( 'NONE',  ( -10.62949710387652758, 20.32685691788189075, 11.49999999999998934 ) ) ;
#71256 = DIRECTION ( 'NONE',  ( 0.000000000000000000, -1.000000000000000000, 0.000000000000000000 ) ) ;
#71257 = CARTESIAN_POINT ( 'NONE',  ( -19.26508835251014773, 5.270845654819066084, -1.500000000000002220 ) ) ;
#71258 = CARTESIAN_POINT ( 'NONE',  ( 282.9764569301858046, -6.376774720514426953, 20.79159422840526616 ) ) ;
#71259 = CARTESIAN_POINT ( 'NONE',  ( 10.18035917307295435, 18.35650967997132099, 11.49999999999999645 ) ) ;
#71260 = CARTESIAN_POINT ( 'NONE',  ( -29.81175120719462512, -25.25636103033882307, 4.942810967025194735 ) ) ;
#71261 = CARTESIAN_POINT ( 'NONE',  ( -15.87499999999997868, 0.000000000000000000, 0.000000000000000000 ) ) ;
#71262 = CARTESIAN_POINT ( 'NONE',  ( -3.902479932019291553, -21.71820464621639246, 11.49999999999998934 ) ) ;
#71263 = CIRCLE ( 'NONE', #33966, 6.119803529381342422 ) ;
#71264 = DIRECTION ( 'NONE',  ( -1.000000000000000000, -0.000000000000000000, -0.000000000000000000 ) ) ;
#71266 = ORIENTED_EDGE ( 'NONE', *, *, #5921, .F. ) ;
#71265 = EDGE_CURVE ( 'NONE', #28831, #97694, #91434, .T. ) ;
#71267 = CARTESIAN_POINT ( 'NONE',  ( -127.5562042904833646, -23.48786465467242124, 11.44779295918252870 ) ) ;
#71268 = CARTESIAN_POINT ( 'NONE',  ( -49.50841769935764347, -25.27344909660374839, 3.984447732001930920 ) ) ;
#71269 = CARTESIAN_POINT ( 'NONE',  ( -102.6228709571500701, -24.66019654487199730, 8.947790411086121054 ) ) ;
#71270 = ORIENTED_EDGE ( 'NONE', *, *, #88021, .F. ) ;
#71271 = CARTESIAN_POINT ( 'NONE',  ( -123.6228709571500417, -24.50321055353804667, 9.387540953477525818 ) ) ;
#71272 = VERTEX_POINT ( 'NONE', #24238 ) ;
#71273 = AXIS2_PLACEMENT_3D ( 'NONE', #8869, #1270, #48444 ) ;
#71274 = B_SPLINE_CURVE_WITH_KNOTS ( 'NONE', 3,
 ( #63942, #2522, #86740, #38678 ),
 .UNSPECIFIED., .F., .F.,
 ( 4, 4 ),
 ( 0.000000000000000000, 0.0001000000000000028644 ),
 .UNSPECIFIED. ) ;
#71275 = ORIENTED_EDGE ( 'NONE', *, *, #70640, .F. ) ;
#71276 = DIRECTION ( 'NONE',  ( -3.773278334453079618E-23, 0.9999999999976377785, 2.173523156925978705E-06 ) ) ;
#71277 = CARTESIAN_POINT ( 'NONE',  ( -43.52287095715006160, -29.50248528299804818, 1.056150453629031594 ) ) ;
#71278 = CARTESIAN_POINT ( 'NONE',  ( -94.62287095715005592, -24.50321055353806798, 9.387540953477534700 ) ) ;
#71279 = CARTESIAN_POINT ( 'NONE',  ( 11.93631617611541351, -16.73449621718459923, -1.500000000000002220 ) ) ;
#71280 = ORIENTED_EDGE ( 'NONE', *, *, #74633, .F. ) ;
#71281 = CARTESIAN_POINT ( 'NONE',  ( -63.52287095715006160, -24.66019654487199375, 8.947790411086122830 ) ) ;
#71282 = AXIS2_PLACEMENT_3D ( 'NONE', #86266, #78631, #87264 ) ;
#71283 = CARTESIAN_POINT ( 'NONE',  ( -44.55313127954051566, -23.96119346886879953, -0.6495511937832129101 ) ) ;
#71284 = DIRECTION ( 'NONE',  ( 0.8264557562326034779, 0.000000000000000000, 0.5630016722799281448 ) ) ;
#71285 = CARTESIAN_POINT ( 'NONE',  ( -21.62769966018443313, 5.350386031573528989, -1.500000000000002220 ) ) ;
#71286 = CARTESIAN_POINT ( 'NONE',  ( -0.1051205485391841221, -21.68913189117569473, 10.47594215909544246 ) ) ;
#71287 = DIRECTION ( 'NONE',  ( 0.000000000000000000, 0.000000000000000000, 1.000000000000000000 ) ) ;
#71288 = VERTEX_POINT ( 'NONE', #86640 ) ;
#71289 = CARTESIAN_POINT ( 'NONE',  ( -96.62287095715004170, -23.73907113216991860, -1.053371485793224149 ) ) ;
#71290 = VECTOR ( 'NONE', #52553, 1000.000000000000114 ) ;
#71291 = CARTESIAN_POINT ( 'NONE',  ( 0.03625801282051022839, -6.376774720514410077, 19.27714342948718240 ) ) ;
#71292 = AXIS2_PLACEMENT_3D ( 'NONE', #79216, #9718, #32048 ) ;
#71293 = CARTESIAN_POINT ( 'NONE',  ( -10.15938669249390180, 18.18672505111813464, 11.49999999999998934 ) ) ;
#71294 = VERTEX_POINT ( 'NONE', #31353 ) ;
#71296 = ORIENTED_EDGE ( 'NONE', *, *, #3147, .T. ) ;
#71295 = CARTESIAN_POINT ( 'NONE',  ( -116.5228709571500616, -24.65952944569305316, 1.056160979905705899 ) ) ;
#71297 = EDGE_CURVE ( 'NONE', #100201, #92001, #11313, .T. ) ;
#71298 = ORIENTED_EDGE ( 'NONE', *, *, #41309, .T. ) ;
#71299 = AXIS2_PLACEMENT_3D ( 'NONE', #97029, #57990, #51360 ) ;
#71300 = CARTESIAN_POINT ( 'NONE',  ( -68.93918693012690824, -25.03149073271524117, 6.184868930986158198 ) ) ;
#71301 = CARTESIAN_POINT ( 'NONE',  ( -10.24336464640716216, -18.35016636821181280, -1.500000000000002220 ) ) ;
#71302 = ORIENTED_EDGE ( 'NONE', *, *, #58491, .T. ) ;
#71303 = CARTESIAN_POINT ( 'NONE',  ( -110.6228709571500701, -24.82558206586150717, 1.605769216559632895 ) ) ;
#71304 = CARTESIAN_POINT ( 'NONE',  ( -49.68570927577133745, -25.30558383668931910, 4.971112481134402294 ) ) ;
#71305 = DIRECTION ( 'NONE',  ( 0.000000000000000000, 0.000000000000000000, -1.000000000000000000 ) ) ;
#71306 = ADVANCED_FACE ( 'NONE', ( #8013 ), #79019, .T. ) ;
#71307 = CARTESIAN_POINT ( 'NONE',  ( -101.7635726060833434, -25.25419390327883562, 6.809096110917860933 ) ) ;
#71308 = CARTESIAN_POINT ( 'NONE',  ( -59.58303446354969424, -24.51314013834316441, 0.6176544820404136216 ) ) ;
#71309 = LINE ( 'NONE', #53717, #54502 ) ;
#71310 = DIRECTION ( 'NONE',  ( 0.000000000000000000, 0.9999999999976377785, 2.173523156925979975E-06 ) ) ;
#71312 = ORIENTED_EDGE ( 'NONE', *, *, #40541, .F. ) ;
#71311 = CARTESIAN_POINT ( 'NONE',  ( -22.15176777451872425, 1.842445310382735624, 11.49999999999999645 ) ) ;
#71313 = CARTESIAN_POINT ( 'NONE',  ( -1.382686142301752019, 8.868309232919825646, 0.000000000000000000 ) ) ;
#71314 = PLANE ( 'NONE',  #52123 ) ;
#71315 = ORIENTED_EDGE ( 'NONE', *, *, #58676, .F. ) ;
#71316 = CARTESIAN_POINT ( 'NONE',  ( 9.629844747126790949, -20.51516216672183290, -1.500000000000002220 ) ) ;
#71317 = EDGE_CURVE ( 'NONE', #16487, #76018, #90767, .T. ) ;
#71318 = EDGE_CURVE ( 'NONE', #50557, #16956, #47025, .T. ) ;
#71320 = ORIENTED_EDGE ( 'NONE', *, *, #10524, .F. ) ;
#71319 = FACE_OUTER_BOUND ( 'NONE', #23462, .T. ) ;
#71321 = EDGE_LOOP ( 'NONE', ( #69305, #86982, #50679, #45853 ) ) ;
#71322 = EDGE_CURVE ( 'NONE', #37450, #62739, #86140, .T. ) ;
#71323 = CARTESIAN_POINT ( 'NONE',  ( -47.62287095715004881, -24.64965695001467694, 8.947790433994185832 ) ) ;
#71324 = B_SPLINE_CURVE_WITH_KNOTS ( 'NONE', 3,
 ( #94539, #24021, #39747, #47878 ),
 .UNSPECIFIED., .F., .F.,
 ( 4, 4 ),
 ( 0.000000000000000000, 1.000000000000000000 ),
 .UNSPECIFIED. ) ;
#71325 = CARTESIAN_POINT ( 'NONE',  ( 14.24339680280927567, 14.23919408161895284, -1.500000000000002220 ) ) ;
#71326 = DIRECTION ( 'NONE',  ( -3.773278334453079618E-23, 0.9999999999976377785, 2.173523156925979975E-06 ) ) ;
#71327 = ORIENTED_EDGE ( 'NONE', *, *, #12649, .F. ) ;
#71328 = PLANE ( 'NONE',  #63343 ) ;
#71329 = CARTESIAN_POINT ( 'NONE',  ( -18.60458529277170214, -12.42720982490441095, -1.500000000000002220 ) ) ;
#71330 = EDGE_CURVE ( 'NONE', #36098, #14495, #77009, .T. ) ;
#71331 = ORIENTED_EDGE ( 'NONE', *, *, #36622, .T. ) ;
#71332 = ORIENTED_EDGE ( 'NONE', *, *, #80739, .T. ) ;
#71333 = CARTESIAN_POINT ( 'NONE',  ( 30.09341516180546350, -1.477225279485574028, -11.39311774897855756 ) ) ;
#71334 = CARTESIAN_POINT ( 'NONE',  ( -122.5228709571500616, -29.50247984919015209, -1.443849546365046699 ) ) ;
#71335 = CARTESIAN_POINT ( 'NONE',  ( -41.52287095715005449, -23.96127896942119051, -0.6493128930941884924 ) ) ;
#71336 = CARTESIAN_POINT ( 'NONE',  ( -97.26334014122947735, -23.47593901973090524, -1.443836447538996648 ) ) ;
#71337 = CARTESIAN_POINT ( 'NONE',  ( -18.23851433863309879, 7.102826447048048664, 11.49999999999998934 ) ) ;
#71338 = PLANE ( 'NONE',  #16616 ) ;
#71339 = ORIENTED_EDGE ( 'NONE', *, *, #18955, .F. ) ;
#71340 = CARTESIAN_POINT ( 'NONE',  ( 16.48747857468482891, 13.79107804547330929, 11.49999999999998934 ) ) ;
#71341 = CARTESIAN_POINT ( 'NONE',  ( 27.53860345374808105, -1.477225279485574028, 19.84760796525321780 ) ) ;
#71342 = CARTESIAN_POINT ( 'NONE',  ( -54.62287095715004170, -24.33927499327855060, 9.819080762295818943 ) ) ;
#71343 = CARTESIAN_POINT ( 'NONE',  ( -63.52287095715006160, -24.66019654487199375, 8.947790411086122830 ) ) ;
#71344 = VECTOR ( 'NONE', #59177, 1000.000000000000114 ) ;
#71345 = CARTESIAN_POINT ( 'NONE',  ( -111.6228709571500701, -23.96127896941633750, -0.6493128931037791540 ) ) ;
#71346 = CARTESIAN_POINT ( 'NONE',  ( -0.4961427919413599064, 22.93664481792237453, -1.500000000000002220 ) ) ;
#71347 = EDGE_CURVE ( 'NONE', #26963, #12709, #97563, .T. ) ;
#71348 = EDGE_CURVE ( 'NONE', #73913, #81354, #54705, .T. ) ;
#71349 = APPROVAL_DATE_TIME ( #57631, #42673 ) ;
#71350 = LINE ( 'NONE', #63757, #46668 ) ;
#71351 = CARTESIAN_POINT ( 'NONE',  ( -70.66096558152140972, -25.31062324876412006, 5.350544532130630415 ) ) ;
#71352 = CARTESIAN_POINT ( 'NONE',  ( -20.00956492049148494, -0.6725752471728385640, 11.49999999999999645 ) ) ;
#71353 = CARTESIAN_POINT ( 'NONE',  ( -79.16633218095056179, -25.26612511361882341, 5.138964462063473349 ) ) ;
#71354 = CARTESIAN_POINT ( 'NONE',  ( 30.53060340732036337, 5.297812262124996785, 1.539714685317421505 ) ) ;
#71355 = CARTESIAN_POINT ( 'NONE',  ( 4.692776824272364422, -5.876774720514406525, 18.67160386110882442 ) ) ;
#71356 = DIRECTION ( 'NONE',  ( 0.000000000000000000, -0.000000000000000000, -1.000000000000000000 ) ) ;
#71357 = CARTESIAN_POINT ( 'NONE',  ( -65.55620429048339304, -23.47593901973091235, -1.443836447539006196 ) ) ;
#71358 = EDGE_CURVE ( 'NONE', #97163, #79765, #63620, .T. ) ;
#71359 = CARTESIAN_POINT ( 'NONE',  ( 14.05712878599199200, -16.60762996970646199, 11.49999999999998934 ) ) ;
#71360 = DIRECTION ( 'NONE',  ( 0.000000000000000000, 0.000000000000000000, 1.000000000000000000 ) ) ;
#71361 = CARTESIAN_POINT ( 'NONE',  ( -6.620539020842763911, -18.51205181221761720, -1.500000000000002220 ) ) ;
#71362 = DIRECTION ( 'NONE',  ( 0.000000000000000000, 0.000000000000000000, 1.000000000000000000 ) ) ;
#71363 = EDGE_CURVE ( 'NONE', #57842, #29757, #81745, .T. ) ;
#71364 = EDGE_CURVE ( 'NONE', #93240, #87941, #58694, .T. ) ;
#71365 = AXIS2_PLACEMENT_3D ( 'NONE', #71935, #12013, #73427 ) ;
#71366 = CARTESIAN_POINT ( 'NONE',  ( 27.53860345374771867, -4.132774720517318201, -9.482392034746242260 ) ) ;
#71367 = PERSON_AND_ORGANIZATION ( #45265, #70186 ) ;
#71368 = VECTOR ( 'NONE', #20448, 1000.000000000000000 ) ;
#71369 = CARTESIAN_POINT ( 'NONE',  ( 11.62916340711181284, -0.3587747205144265483, 28.75961759920349792 ) ) ;
#71370 = CARTESIAN_POINT ( 'NONE',  ( -102.5228709571501042, -23.48783264083375144, -1.443836473376139740 ) ) ;
#71371 = CARTESIAN_POINT ( 'NONE',  ( 18.12345787009687115, -9.690629616749632191, 11.49999999999999645 ) ) ;
#71372 = CARTESIAN_POINT ( 'NONE',  ( 4.573489327750471567, -6.376774720514420736, 20.79634280254998657 ) ) ;
#71373 = FACE_OUTER_BOUND ( 'NONE', #56557, .T. ) ;
#71374 = VECTOR ( 'NONE', #22636, 1000.000000000000114 ) ;
#71375 = CARTESIAN_POINT ( 'NONE',  ( 0.2737972009257602091, 22.58959237946467624, 11.49999999999999645 ) ) ;
#71376 = VERTEX_POINT ( 'NONE', #87650 ) ;
#71377 =( NAMED_UNIT ( * ) SI_UNIT ( $, .STERADIAN. ) SOLID_ANGLE_UNIT ( ) );
#71378 = CARTESIAN_POINT ( 'NONE',  ( -69.94684934828960365, -25.25639587450186951, 7.037048054415059539 ) ) ;
#71379 = DIRECTION ( 'NONE',  ( 0.000000000000000000, 0.000000000000000000, -1.000000000000000000 ) ) ;
#71380 = CARTESIAN_POINT ( 'NONE',  ( -97.54780332990628722, -24.51314013834316086, 0.6176544820404162861 ) ) ;
#71381 = CARTESIAN_POINT ( 'NONE',  ( -72.62287095715005592, -24.64965695001468404, 8.947790433994184056 ) ) ;
#71382 = CARTESIAN_POINT ( 'NONE',  ( -25.53444008324515124, -24.93062977454840023, 5.226875182649808771 ) ) ;
#71383 = FACE_OUTER_BOUND ( 'NONE', #41653, .T. ) ;
#71384 = ORIENTED_EDGE ( 'NONE', *, *, #96206, .T. ) ;
#71385 = DIRECTION ( 'NONE',  ( -0.5630016722799281448, 5.365801633547210331E-16, 0.8264557562326034779 ) ) ;
#71386 = CARTESIAN_POINT ( 'NONE',  ( -22.75767140345847750, 1.815691853630000629, 11.49999999999998934 ) ) ;
#71387 = CARTESIAN_POINT ( 'NONE',  ( -69.52287095715006160, -23.47596703998600631, 11.44779298504228748 ) ) ;
#71388 = CARTESIAN_POINT ( 'NONE',  ( -96.51332711276727139, -24.15543982623907482, -0.2315651400026596807 ) ) ;
#71389 = CARTESIAN_POINT ( 'NONE',  ( 8.971512145086528278, -9.528487854913501920, 6.500000000000001776 ) ) ;
#71390 = CARTESIAN_POINT ( 'NONE',  ( 3.433349652534986696, 22.22849440524942111, 11.49999999999999645 ) ) ;
#71391 = ORIENTED_EDGE ( 'NONE', *, *, #94359, .F. ) ;
#71392 = CARTESIAN_POINT ( 'NONE',  ( -43.61623332758254179, -23.48783264082478084, -1.443836473390076369 ) ) ;
#71393 = CARTESIAN_POINT ( 'NONE',  ( 14.12621959167996977, 16.79361087625908056, -1.500000000000002220 ) ) ;
#71394 = CARTESIAN_POINT ( 'NONE',  ( 32.74291612378888061, 3.662501476888925467, -3.918438066536008346 ) ) ;
#71395 = CARTESIAN_POINT ( 'NONE',  ( -34.66748501521039572, -23.48786465467240347, 11.44779295918255535 ) ) ;
#71396 = PLANE ( 'NONE',  #63277 ) ;
#71397 = ORIENTED_EDGE ( 'NONE', *, *, #49348, .T. ) ;
#71398 = CARTESIAN_POINT ( 'NONE',  ( 13.57151214508650305, -0.8999999999999998002, -1.500000000000000666 ) ) ;
#71399 = CARTESIAN_POINT ( 'NONE',  ( 30.53060340732036337, -5.340035977923286659, 2.705756132044235152 ) ) ;
#71400 = ORIENTED_EDGE ( 'NONE', *, *, #51407, .T. ) ;
#71401 = CARTESIAN_POINT ( 'NONE',  ( -8.751980504941329286, -18.49744413911281882, 11.49999999999998934 ) ) ;
#71402 = ORIENTED_EDGE ( 'NONE', *, *, #91518, .T. ) ;
#71403 = ORIENTED_EDGE ( 'NONE', *, *, #20018, .T. ) ;
#71404 = ORIENTED_EDGE ( 'NONE', *, *, #13604, .T. ) ;
#71405 = ORIENTED_EDGE ( 'NONE', *, *, #66142, .T. ) ;
#71406 = CARTESIAN_POINT ( 'NONE',  ( 22.95697726795019378, -2.620641032420567118, -1.500000000000002220 ) ) ;
#71407 = CARTESIAN_POINT ( 'NONE',  ( -102.6228709571500701, -24.66019654487199730, 8.947790411086121054 ) ) ;
#71408 = CARTESIAN_POINT ( 'NONE',  ( 3.729398819442638846, -20.01364129133569136, -1.500000000000002220 ) ) ;
#71409 = ORIENTED_EDGE ( 'NONE', *, *, #98325, .T. ) ;
#71410 = CARTESIAN_POINT ( 'NONE',  ( 19.75748517575715368, -0.3587747205144265483, 28.87153971905864580 ) ) ;
#71411 = DIRECTION ( 'NONE',  ( 0.000000000000000000, 0.000000000000000000, -1.000000000000000000 ) ) ;
#71412 = DIRECTION ( 'NONE',  ( -1.000000000000000000, -3.773278334444166432E-23, -8.201307841325785021E-29 ) ) ;
#71413 = CARTESIAN_POINT ( 'NONE',  ( 4.639502537026700679, -6.376774720514415407, 19.60647575951318800 ) ) ;
#71415 = EDGE_LOOP ( 'NONE', ( #68417, #1137, #16492, #60758 ) ) ;
#71414 = CARTESIAN_POINT ( 'NONE',  ( 19.32660459246815421, -9.429101867163046435, 11.49999999999999645 ) ) ;
#71416 = CARTESIAN_POINT ( 'NONE',  ( -75.63151842343319231, -24.63355581998385802, 0.9682620441943947664 ) ) ;
#71417 = DIRECTION ( 'NONE',  ( -3.773278334453080206E-23, 0.9999999999976377785, 2.173523156925979975E-06 ) ) ;
#71418 = VERTEX_POINT ( 'NONE', #73917 ) ;
#71419 = B_SPLINE_CURVE_WITH_KNOTS ( 'NONE', 3,
 ( #57290, #2485, #4846, #66773, #72499, #95326, #41046, #97691, #63399, #86705, #80098, #33419, #94316, #28186, #10583 ),
 .UNSPECIFIED., .F., .F.,
 ( 4, 1, 1, 1, 1, 1, 1, 1, 1, 1, 1, 1, 4 ),
 ( 0.000000000000000000, 0.09781818961471311358, 0.1997260534018265310, 0.3052763574779380207, 0.4158114905382894744, 0.4744722311435595752, 0.5372738797760960860, 0.6036574205596552112, 0.6742988630901243230, 0.7498344853162268731, 0.8285984767571009657, 0.9123777781577814272, 1.000000000000000000 ),
 .UNSPECIFIED. ) ;
#71420 = CARTESIAN_POINT ( 'NONE',  ( 8.056674255711671506, 19.11000797562349618, 11.49999999999998934 ) ) ;
#71421 = CIRCLE ( 'NONE', #27669, 1.049999999999998934 ) ;
#71422 = VERTEX_POINT ( 'NONE', #19621 ) ;
#71424 = VERTEX_POINT ( 'NONE', #4415 ) ;
#71423 = CARTESIAN_POINT ( 'NONE',  ( -89.49044894935767047, -29.50248914370730091, 2.832395270851967073 ) ) ;
#71425 = ADVANCED_FACE ( 'NONE', ( #50582 ), #95255, .T. ) ;
#71426 = CARTESIAN_POINT ( 'NONE',  ( 14.76093561896379214, -6.475225279485573360, -27.88148769130088667 ) ) ;
#71427 = CARTESIAN_POINT ( 'NONE',  ( -108.6228709571500559, -29.50247984919015209, -1.443849546365048253 ) ) ;
#71428 = VERTEX_POINT ( 'NONE', #18131 ) ;
#71429 = ORIENTED_EDGE ( 'NONE', *, *, #41534, .F. ) ;
#71430 = ADVANCED_FACE ( 'NONE', ( #49100 ), #58204, .F. ) ;
#71431 = CARTESIAN_POINT ( 'NONE',  ( -40.52287095715006870, -24.52232992886361629, 0.6492154411905992628 ) ) ;
#71432 = PLANE ( 'NONE',  #25448 ) ;
#71433 = CARTESIAN_POINT ( 'NONE',  ( -28.89873962686151287, -24.82198293592782079, 2.051091576938187444 ) ) ;
#71435 = ORIENTED_EDGE ( 'NONE', *, *, #29938, .F. ) ;
#71434 = CARTESIAN_POINT ( 'NONE',  ( 13.70243205411677145, -17.22335469805116048, 11.49999999999999645 ) ) ;
#71436 = CARTESIAN_POINT ( 'NONE',  ( -101.5895376238167387, -23.47596703998600631, 11.44779298504227683 ) ) ;
#71437 = CARTESIAN_POINT ( 'NONE',  ( -13.16310354753345990, -18.33534949228788236, 11.49999999999998934 ) ) ;
#71438 = EDGE_CURVE ( 'NONE', #54707, #50701, #89138, .T. ) ;
#71439 = CARTESIAN_POINT ( 'NONE',  ( 20.78037738254806399, 3.014218216234254566, 11.49999999999998934 ) ) ;
#71440 = ADVANCED_FACE ( 'NONE', ( #11021 ), #64338, .T. ) ;
#71442 = ORIENTED_EDGE ( 'NONE', *, *, #741, .F. ) ;
#71441 = CARTESIAN_POINT ( 'NONE',  ( -70.62287095715007013, -24.91544648472620693, 1.928969306349231472 ) ) ;
#71443 = B_SPLINE_CURVE_WITH_KNOTS ( 'NONE', 3,
 ( #38380, #99758, #46009, #30263, #16531, #92658 ),
 .UNSPECIFIED., .F., .F.,
 ( 4, 2, 4 ),
 ( 6.391158118975501388E-06, 0.001387004593080791133, 0.002767618028042606766 ),
 .UNSPECIFIED. ) ;
#71444 = CIRCLE ( 'NONE', #27687, 28.96799999999999287 ) ;
#71445 = ORIENTED_EDGE ( 'NONE', *, *, #55113, .F. ) ;
#71447 = EDGE_CURVE ( 'NONE', #92224, #79658, #72928, .T. ) ;
#71446 = AXIS2_PLACEMENT_3D ( 'NONE', #13234, #5631, #36577 ) ;
#71448 = CYLINDRICAL_SURFACE ( 'NONE', #72577, 251.4258649670780699 ) ;
#71449 = CARTESIAN_POINT ( 'NONE',  ( 9.071512145086501278, -0.9000000000000000222, -3.687490859131162591 ) ) ;
#71450 = VERTEX_POINT ( 'NONE', #3429 ) ;
#71451 = CARTESIAN_POINT ( 'NONE',  ( 14.48694714638828884, 15.39972936300609341, -1.500000000000002220 ) ) ;
#71452 = FACE_OUTER_BOUND ( 'NONE', #94644, .T. ) ;
#71453 = CARTESIAN_POINT ( 'NONE',  ( -51.44452858623887437, -25.03148670408844012, 7.233630129720098445 ) ) ;
#71454 = CARTESIAN_POINT ( 'NONE',  ( -121.5556940823614127, -23.96119346886880308, -0.6495511937832032512 ) ) ;
#71455 = CARTESIAN_POINT ( 'NONE',  ( -7.304748120944324796, -6.376774720514417183, 19.95463486386180563 ) ) ;
#71456 = CARTESIAN_POINT ( 'NONE',  ( -47.62287095715004881, -24.64965695001467694, 8.947790433994185832 ) ) ;
#71457 = CARTESIAN_POINT ( 'NONE',  ( 19.10802705166043580, 11.29804532628753044, -1.500000000000002220 ) ) ;
#71458 = CARTESIAN_POINT ( 'NONE',  ( -74.62287095715005592, -23.47596703998600631, 11.44779298504227860 ) ) ;
#71459 = EDGE_CURVE ( 'NONE', #39807, #72214, #95047, .T. ) ;
#71460 = VERTEX_POINT ( 'NONE', #2926 ) ;
#71461 = CARTESIAN_POINT ( 'NONE',  ( 5.271800844830267785, 5.965225279485592225, -28.56638892017480913 ) ) ;
#71462 = CARTESIAN_POINT ( 'NONE',  ( -58.55620429048339304, -23.47596703998600276, 11.44779298504227505 ) ) ;
#71463 = CARTESIAN_POINT ( 'NONE',  ( -126.5891258169978784, -24.65952944569305316, 1.056160979905705455 ) ) ;
#71465 = B_SPLINE_CURVE_WITH_KNOTS ( 'NONE', 3,
 ( #52321, #98974, #59945, #60447, #13736, #83753, #75632, #44707, #6133, #99471, #20347, #20850, #37086, #68049, #53323, #45209, #76136, #82261 ),
 .UNSPECIFIED., .F., .F.,
 ( 4, 2, 2, 2, 2, 2, 2, 2, 4 ),
 ( 0.000000000000000000, 0.0002883515756762773229, 0.0005767031513525546459, 0.0008650547270288318604, 0.001153406302705109292, 0.001730109454057662420, 0.002018461029733941044, 0.002162636817572077211, 0.002306812605410212946 ),
 .UNSPECIFIED. ) ;
#71464 = FACE_OUTER_BOUND ( 'NONE', #16504, .T. ) ;
#71466 = CARTESIAN_POINT ( 'NONE',  ( -33.62287095715005592, -23.47596703998600276, 11.44779298504227505 ) ) ;
#71467 = EDGE_CURVE ( 'NONE', #17861, #18030, #64844, .T. ) ;
#71468 = CARTESIAN_POINT ( 'NONE',  ( -16.97169330436246781, 9.548981535075045102, 11.49999999999998934 ) ) ;
#71469 = CARTESIAN_POINT ( 'NONE',  ( 10.55508701655855575, -18.62573008410804221, 11.49999999999998934 ) ) ;
#71470 = DIRECTION ( 'NONE',  ( -0.6392559695863496705, -6.845827386180411947E-16, -0.7689940216596069522 ) ) ;
#71471 = DIRECTION ( 'NONE',  ( 0.000000000000000000, 0.000000000000000000, 1.000000000000000000 ) ) ;
#71472 = CARTESIAN_POINT ( 'NONE',  ( -116.6228709571500559, -23.47593901973091235, -1.443836447538997536 ) ) ;
#71473 = CARTESIAN_POINT ( 'NONE',  ( -36.92287095715006018, -23.47593901973090169, -1.443836447538998202 ) ) ;
#71474 = CARTESIAN_POINT ( 'NONE',  ( -17.66434017299383896, 14.31182286555179139, -1.500000000000002220 ) ) ;
#71475 = EDGE_CURVE ( 'NONE', #40343, #61548, #66148, .T. ) ;
#71476 = DIRECTION ( 'NONE',  ( 0.000000000000000000, 0.000000000000000000, 1.000000000000000000 ) ) ;
#71477 = DIRECTION ( 'NONE',  ( 3.773278334444167608E-23, -1.000000000000000000, 0.000000000000000000 ) ) ;
#71478 = CARTESIAN_POINT ( 'NONE',  ( 15.00000000000000533, 0.000000000000000000, 24.00000000000000000 ) ) ;
#71479 = CARTESIAN_POINT ( 'NONE',  ( -1.214729172165279092, -19.82145330704504360, 11.49999999999999645 ) ) ;
#71480 = CARTESIAN_POINT ( 'NONE',  ( 5.786755829966409692, -6.376774720514413630, 19.89762986309224857 ) ) ;
#71481 = LINE ( 'NONE', #15170, #39229 ) ;
#71482 = CARTESIAN_POINT ( 'NONE',  ( 29.73860345376319003, 5.356471260711259674, 19.84760796525321780 ) ) ;
#71483 = VERTEX_POINT ( 'NONE', #65829 ) ;
#71484 = CARTESIAN_POINT ( 'NONE',  ( -49.27933479010542328, -25.24522353769383898, 6.214461776597443254 ) ) ;
#71485 = DIRECTION ( 'NONE',  ( 1.000000000000000000, -0.000000000000000000, -0.000000000000000000 ) ) ;
#71486 = CARTESIAN_POINT ( 'NONE',  ( -50.89113880358890185, -25.10935775592824726, 2.917241375188960095 ) ) ;
#71487 = CARTESIAN_POINT ( 'NONE',  ( -10.04279811845843007, 19.21892966915218892, 11.49999999999998934 ) ) ;
#71488 = CARTESIAN_POINT ( 'NONE',  ( -84.52287095715004739, -24.51387760970724372, 9.387446482453409402 ) ) ;
#71489 = CARTESIAN_POINT ( 'NONE',  ( 17.91360334016800593, 7.682165803940314674, -1.500000000000002220 ) ) ;
#71490 = CARTESIAN_POINT ( 'NONE',  ( -55.52866363368176650, -24.92592662359561118, 8.075495903017996469 ) ) ;
#71491 = EDGE_CURVE ( 'NONE', #70059, #81022, #4939, .T. ) ;
#71492 = ORIENTED_EDGE ( 'NONE', *, *, #56419, .T. ) ;
#71493 = CARTESIAN_POINT ( 'NONE',  ( 0.5039804632396667206, -20.40334623801319580, 11.49999999999999645 ) ) ;
#71494 = DIRECTION ( 'NONE',  ( 0.000000000000000000, -0.9999999999976377785, -2.173523156925979128E-06 ) ) ;
#71496 = EDGE_CURVE ( 'NONE', #17763, #100181, #693, .T. ) ;
#71495 = VECTOR ( 'NONE', #40532, 1000.000000000000000 ) ;
#71497 = CARTESIAN_POINT ( 'NONE',  ( -41.58953762381673158, -23.47593901973091235, -1.443836447539011525 ) ) ;
#71498 = ORIENTED_EDGE ( 'NONE', *, *, #13338, .F. ) ;
#71499 = CARTESIAN_POINT ( 'NONE',  ( -79.79717327896997858, -25.06342317198667047, 7.417202478348898786 ) ) ;
#71500 = CARTESIAN_POINT ( 'NONE',  ( 33.64270623324222953, 3.650451339955370855, -11.69061897474703571 ) ) ;
#71501 = CARTESIAN_POINT ( 'NONE',  ( -39.42702772597635175, -25.31628691207657766, 5.331662186571982431 ) ) ;
#71502 = CARTESIAN_POINT ( 'NONE',  ( -49.35642674012009223, -25.31439406600090081, 5.792946613328529004 ) ) ;
#71503 = CARTESIAN_POINT ( 'NONE',  ( -86.52287095715007581, -23.96127896942158841, -0.6493128930933981247 ) ) ;
#71504 = CARTESIAN_POINT ( 'NONE',  ( 13.72940079880349984, -14.68433028913016791, 11.49999999999998934 ) ) ;
#71505 = CARTESIAN_POINT ( 'NONE',  ( -87.62287095715004170, -23.47593901973091235, -1.443836447539002865 ) ) ;
#71506 = ORIENTED_EDGE ( 'NONE', *, *, #72872, .T. ) ;
#71507 = CYLINDRICAL_SURFACE ( 'NONE', #90078, 4.299999999999999822 ) ;
#71508 = VECTOR ( 'NONE', #27169, 1000.000000000000114 ) ;
#71509 = CARTESIAN_POINT ( 'NONE',  ( 22.43992371924722917, 4.826111843257130829, 11.49999999999999645 ) ) ;
#71510 = B_SPLINE_CURVE_WITH_KNOTS ( 'NONE', 3,
 ( #10176, #80685, #50247, #63993, #94906, #81184 ),
 .UNSPECIFIED., .F., .F.,
 ( 4, 2, 4 ),
 ( 1.570887131794638196E-05, 0.001396322306279763458, 0.002776935741241580609 ),
 .UNSPECIFIED. ) ;
#71511 = CARTESIAN_POINT ( 'NONE',  ( 15.23092229589061830, -16.91372389758942418, 11.49999999999998934 ) ) ;
#71512 = VERTEX_POINT ( 'NONE', #84382 ) ;
#71513 = CARTESIAN_POINT ( 'NONE',  ( -109.6228709571500417, -24.65952944569305316, 1.056160979905704345 ) ) ;
#71514 = DIRECTION ( 'NONE',  ( 0.000000000000000000, 0.000000000000000000, 1.000000000000000000 ) ) ;
#71515 = CARTESIAN_POINT ( 'NONE',  ( -90.54023547609000389, -25.00158670708910336, 2.256160236439220146 ) ) ;
#71516 = AXIS2_PLACEMENT_3D ( 'NONE', #87185, #71476, #25281 ) ;
#71517 = CARTESIAN_POINT ( 'NONE',  ( -49.52287095715005449, -23.73907113216989373, -1.053371485793255902 ) ) ;
#71518 = CARTESIAN_POINT ( 'NONE',  ( -69.58783992205957247, -24.35071581493542681, 9.817618358456032368 ) ) ;
#71519 = DIRECTION ( 'NONE',  ( 0.000000000000000000, -1.000000000000000000, 0.000000000000000000 ) ) ;
#71520 = CARTESIAN_POINT ( 'NONE',  ( -54.52287095715006160, -23.94994826722564696, -0.6494450866342733608 ) ) ;
#71521 = CARTESIAN_POINT ( 'NONE',  ( -58.64320200748918666, -23.96119346886880308, -0.6495511937832116889 ) ) ;
#71522 = VERTEX_POINT ( 'NONE', #84879 ) ;
#71523 = CARTESIAN_POINT ( 'NONE',  ( -0.5597704280004801580, 20.37679164443051505, 11.49999999999998934 ) ) ;
#71524 = VERTEX_POINT ( 'NONE', #23460 ) ;
#71525 = ORIENTED_EDGE ( 'NONE', *, *, #57305, .F. ) ;
#71526 = CARTESIAN_POINT ( 'NONE',  ( 18.48385363477634513, -13.70420857335572506, 11.49999999999998934 ) ) ;
#71527 = CARTESIAN_POINT ( 'NONE',  ( -6.815415664272417295, -5.876774720514410966, 19.46427715384223234 ) ) ;
#71528 = VERTEX_POINT ( 'NONE', #90140 ) ;
#71529 = DIRECTION ( 'NONE',  ( -3.773278334453079030E-23, 0.9999999999976377785, 2.173523156925979128E-06 ) ) ;
#71530 = CARTESIAN_POINT ( 'NONE',  ( -101.5228709571500474, -24.33832256527048088, 0.1851278514138640363 ) ) ;
#71531 = CARTESIAN_POINT ( 'NONE',  ( -122.5562042904833930, -24.66019654487199730, 8.947790411086121054 ) ) ;
#71532 = CARTESIAN_POINT ( 'NONE',  ( 3.300000000000004707, 4.450000000000000178, 0.000000000000000000 ) ) ;
#71534 = ORIENTED_EDGE ( 'NONE', *, *, #2709, .T. ) ;
#71533 = CARTESIAN_POINT ( 'NONE',  ( 17.14628872753620215, 12.71262973326862245, 11.49999999999999645 ) ) ;
#71535 = ORIENTED_EDGE ( 'NONE', *, *, #75182, .T. ) ;
#71536 = CARTESIAN_POINT ( 'NONE',  ( -22.22723998432330106, 0.1330083165726352878, -1.500000000000002220 ) ) ;
#71537 = CARTESIAN_POINT ( 'NONE',  ( -15.52656095410427817, -13.64048245868121434, -1.500000000000002220 ) ) ;
#71538 = ORIENTED_EDGE ( 'NONE', *, *, #68378, .F. ) ;
#71539 = CARTESIAN_POINT ( 'NONE',  ( -5.837039262820512775, -5.876774720514413630, 19.76512419871795245 ) ) ;
#71540 = CARTESIAN_POINT ( 'NONE',  ( -95.62721265448736574, -24.73531770709095312, 8.716586749053508498 ) ) ;
#71541 = ORIENTED_EDGE ( 'NONE', *, *, #61110, .T. ) ;
#71542 = EDGE_CURVE ( 'NONE', #55530, #57540, #100079, .T. ) ;
#71543 = DIRECTION ( 'NONE',  ( 0.000000000000000000, 0.9999999999976377785, 2.173523156925979975E-06 ) ) ;
#71544 = ORIENTED_EDGE ( 'NONE', *, *, #73377, .F. ) ;
#71546 = ADVANCED_FACE ( 'NONE', ( #14862 ), #51585, .T. ) ;
#71545 = CARTESIAN_POINT ( 'NONE',  ( -58.61167521426755656, -23.48786465467241058, 11.44779295918254824 ) ) ;
#71547 = CYLINDRICAL_SURFACE ( 'NONE', #42270, 3.549999999999999378 ) ;
#71548 = CARTESIAN_POINT ( 'NONE',  ( 20.83135763335140922, 1.668377004047274959, -1.500000000000002220 ) ) ;
#71549 = CARTESIAN_POINT ( 'NONE',  ( -18.37190169643047355, -11.86832528159398237, 11.49999999999999645 ) ) ;
#71550 = ADVANCED_FACE ( 'NONE', ( #36355 ), #74414, .F. ) ;
#71551 = CARTESIAN_POINT ( 'NONE',  ( -73.58111444669631851, -24.66019654487200441, 8.947790411086119278 ) ) ;
#71552 = CARTESIAN_POINT ( 'NONE',  ( -37.62287095715005592, -23.73907113216990439, -1.053371485793235918 ) ) ;
#71553 = CARTESIAN_POINT ( 'NONE',  ( -6.794891441663577503, 21.43730618243864683, 11.49999999999998934 ) ) ;
#71554 = EDGE_CURVE ( 'NONE', #40469, #50986, #74370, .T. ) ;
#71555 = CARTESIAN_POINT ( 'NONE',  ( -44.55620429048339304, -24.64898659630527789, 1.056161002820819039 ) ) ;
#71556 = LINE ( 'NONE', #40098, #95466 ) ;
#71557 = CARTESIAN_POINT ( 'NONE',  ( -78.58953762381673869, -23.48783264082478439, -1.443836473390065711 ) ) ;
#71558 = ORIENTED_EDGE ( 'NONE', *, *, #7791, .T. ) ;
#71559 = B_SPLINE_CURVE_WITH_KNOTS ( 'NONE', 3,
 ( #46145, #68480, #53262, #29406, #7073, #37027 ),
 .UNSPECIFIED., .F., .F.,
 ( 4, 2, 4 ),
 ( 1.570887131794333942E-05, 0.001396322306279760422, 0.002776935741241577573 ),
 .UNSPECIFIED. ) ;
#71560 = ORIENTED_EDGE ( 'NONE', *, *, #66413, .F. ) ;
#71561 = ORIENTED_EDGE ( 'NONE', *, *, #95836, .F. ) ;
#71562 = CIRCLE ( 'NONE', #9980, 0.2499999999997798983 ) ;
#71563 = CARTESIAN_POINT ( 'NONE',  ( -52.60590739768218782, -23.73766607897671221, -1.055555164236436472 ) ) ;
#71564 = ORIENTED_EDGE ( 'NONE', *, *, #1565, .F. ) ;
#71565 = CARTESIAN_POINT ( 'NONE',  ( 17.72605931280000391, -11.99821887194124770, -1.500000000000002220 ) ) ;
#71566 = EDGE_CURVE ( 'NONE', #78758, #86308, #7249, .T. ) ;
#71567 = CARTESIAN_POINT ( 'NONE',  ( 0.3464652362752086434, -22.36268665536068667, 11.49999999999999645 ) ) ;
#71568 = EDGE_LOOP ( 'NONE', ( #74943, #289, #8756, #69976 ) ) ;
#71569 = CARTESIAN_POINT ( 'NONE',  ( 31.68302997424993350, -5.121054483180515149, -3.958552486145202831 ) ) ;
#71570 = CARTESIAN_POINT ( 'NONE',  ( 21.04674311342985860, -0.3259866984596996864, -1.500000000000002220 ) ) ;
#71571 = CARTESIAN_POINT ( 'NONE',  ( -30.57654984345184701, -25.31559415887666020, 6.147639284700202822 ) ) ;
#71572 = CARTESIAN_POINT ( 'NONE',  ( 19.80199147212610811, 2.383747631481649254, -1.500000000000002220 ) ) ;
#71573 = CARTESIAN_POINT ( 'NONE',  ( -101.5193659238633757, -23.73766607897671221, -1.055555164236452237 ) ) ;
#71574 = CARTESIAN_POINT ( 'NONE',  ( -61.52287095715007581, -23.48783264082476308, -1.443836473390092356 ) ) ;
#71575 = CARTESIAN_POINT ( 'NONE',  ( -2.902263480631018577, 21.84654903556016947, -1.500000000000002220 ) ) ;
#71576 = VERTEX_POINT ( 'NONE', #35853 ) ;
#71577 = CARTESIAN_POINT ( 'NONE',  ( -65.49302343295822482, -24.63419186844611275, 9.035850630976918652 ) ) ;
#71578 = LINE ( 'NONE', #19268, #40073 ) ;
#71579 = CARTESIAN_POINT ( 'NONE',  ( -19.85847575633505713, -6.422239212204448044, 11.49999999999999645 ) ) ;
#71580 = CARTESIAN_POINT ( 'NONE',  ( 29.58033090225963591, -3.719533051881441121, 29.19816577366266941 ) ) ;
#71581 = AXIS2_PLACEMENT_3D ( 'NONE', #60880, #69979, #54273 ) ;
#71582 = LINE ( 'NONE', #93392, #5216 ) ;
#71583 = LOCAL_TIME ( 0, 54, 15.00000000000000000, #67741 ) ;
#71584 = CARTESIAN_POINT ( 'NONE',  ( -90.58953762381672448, -25.00158670708909625, 2.256160236439167299 ) ) ;
#71585 = CARTESIAN_POINT ( 'NONE',  ( -14.93283513470682067, -15.21490397768744529, -1.500000000000002220 ) ) ;
#71586 = CARTESIAN_POINT ( 'NONE',  ( -70.58604916688682351, -25.31487095459964820, 4.870313056136089891 ) ) ;
#71587 = CARTESIAN_POINT ( 'NONE',  ( -100.6228709571500559, -29.50250786944525672, 11.44777988621623166 ) ) ;
#71588 = DIRECTION ( 'NONE',  ( 1.000000000000000000, 0.000000000000000000, 0.000000000000000000 ) ) ;
#71589 = CARTESIAN_POINT ( 'NONE',  ( 18.72495633783376334, -0.5000000000000000000, 2.346898003627108320 ) ) ;
#71590 = CARTESIAN_POINT ( 'NONE',  ( -22.11960324842224423, 4.537628740662121629, -1.500000000000002220 ) ) ;
#71591 = PLANE ( 'NONE',  #37685 ) ;
#71592 = ORIENTED_EDGE ( 'NONE', *, *, #55903, .F. ) ;
#71593 = CARTESIAN_POINT ( 'NONE',  ( -101.6228709571500559, -29.50247984919015209, -1.443849546365050029 ) ) ;
#71594 = CARTESIAN_POINT ( 'NONE',  ( -67.92287095715009571, -23.47593901973090524, -1.443836447538997980 ) ) ;
#71595 = CARTESIAN_POINT ( 'NONE',  ( 17.62393913918218402, -8.800128315780904487, 11.49999999999999645 ) ) ;
#71596 = DIRECTION ( 'NONE',  ( 0.000000000000000000, 1.000000000000000000, -0.000000000000000000 ) ) ;
#71597 = PLANE ( 'NONE',  #70653 ) ;
#71598 = VERTEX_POINT ( 'NONE', #97748 ) ;
#71599 = B_SPLINE_CURVE_WITH_KNOTS ( 'NONE', 3,
 ( #50154, #82091, #88712, #12574, #35914, #12067, #51649, #81093, #90701, #43041, #74475, #98294, #66391, #73481 ),
 .UNSPECIFIED., .F., .F.,
 ( 4, 2, 2, 2, 2, 2, 4 ),
 ( 0.000000000000000000, 0.002392375077555367480, 0.003588562616333051004, 0.004784750155110734093, 0.005980937693888416749, 0.007177125232666099405, 0.009569500310221466452 ),
 .UNSPECIFIED. ) ;
#71600 = CARTESIAN_POINT ( 'NONE',  ( -89.52287095715007581, -24.50321055353804667, 9.387540953477524042 ) ) ;
#71601 = CARTESIAN_POINT ( 'NONE',  ( -119.5228709571500758, -24.64965694238408034, 8.947790433994191162 ) ) ;
#71602 = CARTESIAN_POINT ( 'NONE',  ( 4.784292611718075072, -3.316774720514426456, -25.54547254883186014 ) ) ;
#71603 = EDGE_CURVE ( 'NONE', #10167, #27806, #82807, .T. ) ;
#71604 = FACE_OUTER_BOUND ( 'NONE', #99207, .T. ) ;
#71605 = FACE_OUTER_BOUND ( 'NONE', #74143, .T. ) ;
#71606 = CARTESIAN_POINT ( 'NONE',  ( 12.99534586470982234, -14.87506298573330632, -1.500000000000002220 ) ) ;
#71607 = ORIENTED_EDGE ( 'NONE', *, *, #26300, .F. ) ;
#71608 = CARTESIAN_POINT ( 'NONE',  ( -13.58233929615340152, 14.99024694321910900, 11.49999999999999645 ) ) ;
#71609 = CARTESIAN_POINT ( 'NONE',  ( -112.6228709571500701, -23.48786465467241769, 11.44779295918254114 ) ) ;
#71610 = ADVANCED_FACE ( 'NONE', ( #22958 ), #92985, .F. ) ;
#71611 = AXIS2_PLACEMENT_3D ( 'NONE', #97262, #82040, #12519 ) ;
#71612 = ORIENTED_EDGE ( 'NONE', *, *, #87146, .T. ) ;
#71613 = DIRECTION ( 'NONE',  ( -0.000000000000000000, 2.173523156925979552E-06, -0.9999999999976378895 ) ) ;
#71614 = CARTESIAN_POINT ( 'NONE',  ( -69.39786140845737350, -25.27247757640623149, 5.900849392275183902 ) ) ;
#71615 = CARTESIAN_POINT ( 'NONE',  ( -100.4498239493576648, -25.26638541557128548, 7.563173708901921088 ) ) ;
#71616 = DIRECTION ( 'NONE',  ( 0.000000000000000000, 0.000000000000000000, 1.000000000000000000 ) ) ;
#71617 = CARTESIAN_POINT ( 'NONE',  ( -62.58953762381672448, -23.48786465467241058, 11.44779295918254824 ) ) ;
#71618 = CARTESIAN_POINT ( 'NONE',  ( -86.55620429048337883, -24.66019654487199730, 8.947790411086126383 ) ) ;
#71619 = CARTESIAN_POINT ( 'NONE',  ( -19.87929632332335927, 2.386914507623989490, -1.500000000000002220 ) ) ;
#71620 = CARTESIAN_POINT ( 'NONE',  ( -99.92788026055190187, -25.10935056794787457, 2.920408329580228557 ) ) ;
#71621 = CARTESIAN_POINT ( 'NONE',  ( 31.53822845103994865, -4.132774720514425404, -2.786383594989611634 ) ) ;
#71622 = VERTEX_POINT ( 'NONE', #74898 ) ;
#71623 = CARTESIAN_POINT ( 'NONE',  ( 9.354492577077031967, -4.915585290655217321, -26.27927344818281696 ) ) ;
#71624 = LINE ( 'NONE', #41175, #52616 ) ;
#71625 = CARTESIAN_POINT ( 'NONE',  ( -115.6228709571500559, -29.50250786944525672, 11.44777988621622811 ) ) ;
#71626 = B_SPLINE_CURVE_WITH_KNOTS ( 'NONE', 3,
 ( #86754, #48720, #48210, #72051, #71043, #26861, #50702, #73540, #73051, #96873, #88266, #81149 ),
 .UNSPECIFIED., .F., .F.,
 ( 4, 2, 2, 2, 2, 4 ),
 ( 8.673617379884035472E-19, 0.002088620103345146476, 0.003132930155017719064, 0.004177240206690291217, 0.006265860310035430321, 0.008354480413380570292 ),
 .UNSPECIFIED. ) ;
#71627 = AXIS2_PLACEMENT_3D ( 'NONE', #59896, #66527, #51272 ) ;
#71628 = DIRECTION ( 'NONE',  ( -0.000000000000000000, -0.9513357669802769978, 0.3081562241202474572 ) ) ;
#71629 = CARTESIAN_POINT ( 'NONE',  ( -83.63634622578109656, -23.96119346886880308, -0.6495511937832110227 ) ) ;
#71630 = DIRECTION ( 'NONE',  ( -3.773278334444167608E-23, 1.000000000000000000, 0.000000000000000000 ) ) ;
#71631 = DIRECTION ( 'NONE',  ( 0.000000000000000000, -2.173523156925980399E-06, 0.9999999999976378895 ) ) ;
#71632 = ORIENTED_EDGE ( 'NONE', *, *, #72010, .F. ) ;
#71633 = CARTESIAN_POINT ( 'NONE',  ( 5.347689060783223702, 19.56899250667117229, 11.49999999999998934 ) ) ;
#71634 = DIRECTION ( 'NONE',  ( -1.000000000000000000, 0.000000000000000000, 2.246662546894773332E-15 ) ) ;
#71635 = CARTESIAN_POINT ( 'NONE',  ( 30.53060340732036693, -4.132774720514426292, -5.153186819891554471 ) ) ;
#71636 = CARTESIAN_POINT ( 'NONE',  ( -59.49368872175574552, -24.51419770103156281, 9.386484678747184063 ) ) ;
#71637 = ORIENTED_EDGE ( 'NONE', *, *, #91235, .T. ) ;
#71638 = EDGE_CURVE ( 'NONE', #82766, #7634, #43966, .T. ) ;
#71639 = DIRECTION ( 'NONE',  ( 0.000000000000000000, -0.000000000000000000, -1.000000000000000000 ) ) ;
#71640 = B_SPLINE_CURVE_WITH_KNOTS ( 'NONE', 3,
 ( #51485, #51984, #13899, #43870 ),
 .UNSPECIFIED., .F., .F.,
 ( 4, 4 ),
 ( 0.000000000000000000, 9.999999999998206125E-05 ),
 .UNSPECIFIED. ) ;
#71641 = VECTOR ( 'NONE', #28300, 1000.000000000000000 ) ;
#71642 = CARTESIAN_POINT ( 'NONE',  ( 13.25904570721172604, 16.46799385432867169, 11.49999999999999645 ) ) ;
#71643 = CC_DESIGN_SECURITY_CLASSIFICATION ( #29472, ( #21418 ) ) ;
#71644 = CARTESIAN_POINT ( 'NONE',  ( -21.88945651911318535, 3.243594245096953710, 11.49999999999998934 ) ) ;
#71645 = CARTESIAN_POINT ( 'NONE',  ( 3.262959013008915665, -20.29835246810489835, 11.49999999999998934 ) ) ;
#71646 = ORIENTED_EDGE ( 'NONE', *, *, #47477, .F. ) ;
#71647 = DIRECTION ( 'NONE',  ( 0.5630016722799281448, 5.365801633547219206E-16, -0.8264557562326033668 ) ) ;
#71648 = ORIENTED_EDGE ( 'NONE', *, *, #2351, .F. ) ;
#71649 = CARTESIAN_POINT ( 'NONE',  ( 13.57581083383196940, -5.876774720514426953, 20.21213203435597094 ) ) ;
#71650 = CARTESIAN_POINT ( 'NONE',  ( -68.62287095715005592, -29.50247984919015209, -1.443849546365055359 ) ) ;
#71651 = ORIENTED_EDGE ( 'NONE', *, *, #11628, .F. ) ;
#71653 = VERTEX_POINT ( 'NONE', #20258 ) ;
#71652 = ADVANCED_FACE ( 'NONE', ( #7758 ), #66900, .T. ) ;
#71654 = ORIENTED_EDGE ( 'NONE', *, *, #653, .T. ) ;
#71655 = CARTESIAN_POINT ( 'NONE',  ( -100.5228709571500758, -24.51163499207175533, 0.6490370598554370263 ) ) ;
#71657 = CARTESIAN_POINT ( 'NONE',  ( 7.164391295225654765, -6.376774720514420736, 20.71606273170883838 ) ) ;
#71656 = B_SPLINE_CURVE_WITH_KNOTS ( 'NONE', 3,
 ( #6006, #87870, #41712, #64560 ),
 .UNSPECIFIED., .F., .F.,
 ( 4, 4 ),
 ( 0.8293726295494769918, 0.8303733765902421293 ),
 .UNSPECIFIED. ) ;
#71658 = CARTESIAN_POINT ( 'NONE',  ( -91.62287095715004170, -23.96127896941631619, -0.6493128931037837059 ) ) ;
#71659 = CARTESIAN_POINT ( 'NONE',  ( 9.361532043782798240, 18.45020211870636118, -1.500000000000002220 ) ) ;
#71660 = CARTESIAN_POINT ( 'NONE',  ( 13.31326451270642330, 17.06472021985377552, 11.49999999999999645 ) ) ;
#71661 = ORIENTED_EDGE ( 'NONE', *, *, #14952, .T. ) ;
#71662 = EDGE_CURVE ( 'NONE', #4955, #61510, #16892, .T. ) ;
#71663 = CARTESIAN_POINT ( 'NONE',  ( -98.89303308397303738, -25.25494757631710385, 6.110950176066591411 ) ) ;
#71664 = LINE ( 'NONE', #10256, #64235 ) ;
#71665 = CARTESIAN_POINT ( 'NONE',  ( 1.926536275058113867, -22.33200895297504474, 11.49999999999998934 ) ) ;
#71666 = ADVANCED_FACE ( 'NONE', ( #95896 ), #58353, .F. ) ;
#71667 = CARTESIAN_POINT ( 'NONE',  ( -79.47715298469661604, -25.27874961927179953, 6.508607590754126093 ) ) ;
#71668 = DIRECTION ( 'NONE',  ( 0.000000000000000000, -0.9999999999976377785, -2.173523156925979128E-06 ) ) ;
#71669 = ORIENTED_EDGE ( 'NONE', *, *, #50774, .F. ) ;
#71670 = CARTESIAN_POINT ( 'NONE',  ( 29.70917971445138051, 6.219445159570049064, 27.14760184111773356 ) ) ;
#71671 = LINE ( 'NONE', #93482, #62050 ) ;
#71672 = EDGE_CURVE ( 'NONE', #59761, #58570, #10216, .T. ) ;
#71673 = ORIENTED_EDGE ( 'NONE', *, *, #90091, .T. ) ;
#71674 = EDGE_CURVE ( 'NONE', #49847, #26695, #54969, .T. ) ;
#71675 = ORIENTED_EDGE ( 'NONE', *, *, #92956, .F. ) ;
#71676 = CARTESIAN_POINT ( 'NONE',  ( -109.6228709571500559, -23.47596703998600631, 11.44779298504227860 ) ) ;
#71677 = ORIENTED_EDGE ( 'NONE', *, *, #85922, .T. ) ;
#71678 = FACE_OUTER_BOUND ( 'NONE', #35846, .T. ) ;
#71679 = CARTESIAN_POINT ( 'NONE',  ( -6.347832186973104029, -20.24257907634199682, -1.500000000000002220 ) ) ;
#71680 = ORIENTED_EDGE ( 'NONE', *, *, #4303, .T. ) ;
#71681 = FACE_OUTER_BOUND ( 'NONE', #75392, .T. ) ;
#71682 = PRODUCT ( 'Spring-loaded Plate_Varsay\X2\0131\X0\lan', 'Spring-loaded Plate_Varsay\X2\0131\X0\lan', '', ( #3230 ) ) ;
#71683 = CARTESIAN_POINT ( 'NONE',  ( -21.01659442711627790, -5.882202039844940167, 11.49999999999998934 ) ) ;
#71684 = CARTESIAN_POINT ( 'NONE',  ( -52.58235619518457327, -24.51419770103158413, 9.386484678747189392 ) ) ;
#71685 = CARTESIAN_POINT ( 'NONE',  ( -107.5228709571500758, -24.64898659630367916, 1.056161002820831474 ) ) ;
#71686 = CARTESIAN_POINT ( 'NONE',  ( -35.52287095715006870, -23.47596703998600631, 11.44779298504229281 ) ) ;
#71687 = CARTESIAN_POINT ( 'NONE',  ( 19.20967809413044236, -10.42350525531561978, -1.500000000000002220 ) ) ;
#71688 = CARTESIAN_POINT ( 'NONE',  ( -30.57287095715007652, -24.67296300714258805, 8.878589634568275102 ) ) ;
#71689 = ORIENTED_EDGE ( 'NONE', *, *, #90788, .T. ) ;
#71690 = EDGE_CURVE ( 'NONE', #41555, #21327, #1778, .T. ) ;
#71691 = CARTESIAN_POINT ( 'NONE',  ( 26.14999174255633463, 4.132774720517320866, -11.56127575336603286 ) ) ;
#71692 = CARTESIAN_POINT ( 'NONE',  ( -85.54469269819122701, -24.63419186844611275, 9.035850630976915099 ) ) ;
#71693 = ORIENTED_EDGE ( 'NONE', *, *, #80182, .T. ) ;
#71694 = ORIENTED_EDGE ( 'NONE', *, *, #94920, .F. ) ;
#71695 = VERTEX_POINT ( 'NONE', #72571 ) ;
#71696 = VECTOR ( 'NONE', #26792, 1000.000000000000114 ) ;
#71697 = LINE ( 'NONE', #31115, #52442 ) ;
#71698 = CARTESIAN_POINT ( 'NONE',  ( -6.660000000000001030, -10.98394470431085601, -0.7905513910579705650 ) ) ;
#71699 = CARTESIAN_POINT ( 'NONE',  ( -14.73150212448299357, 15.28860238833873808, 11.49999999999998934 ) ) ;
#71700 = CIRCLE ( 'NONE', #14963, 80.18232118519038920 ) ;
#71701 = CARTESIAN_POINT ( 'NONE',  ( 10.46399479596398052, 3.105441387181091972, -27.03001098546561920 ) ) ;
#71702 = CARTESIAN_POINT ( 'NONE',  ( -41.62287095715006302, -24.65952944569303895, 1.056160979905692576 ) ) ;
#71703 = CARTESIAN_POINT ( 'NONE',  ( 29.73860345376318293, 4.772799050253824227, -4.021133283355260879 ) ) ;
#71704 = PLANE ( 'NONE',  #54062 ) ;
#71705 = CARTESIAN_POINT ( 'NONE',  ( -1.428710472040144452, 19.32843595812722626, -1.500000000000002220 ) ) ;
#71706 = CARTESIAN_POINT ( 'NONE',  ( -117.5877651003913229, -24.66019654487200441, 8.947790411086110396 ) ) ;
#71707 = ORIENTED_EDGE ( 'NONE', *, *, #59236, .T. ) ;
#71708 = CARTESIAN_POINT ( 'NONE',  ( 18.70946937610417038, -5.484834493922766896, 11.49999999999999645 ) ) ;
#71709 = CARTESIAN_POINT ( 'NONE',  ( -5.439936175300728927, -5.876774720514408301, 19.67454710845353816 ) ) ;
#71710 = CARTESIAN_POINT ( 'NONE',  ( 10.86264265030973952, 0.3587747205144257157, -27.62597719988137612 ) ) ;
#71711 = EDGE_CURVE ( 'NONE', #11676, #34861, #40579, .T. ) ;
#71712 = VERTEX_POINT ( 'NONE', #27884 ) ;
#71713 = CARTESIAN_POINT ( 'NONE',  ( 4.967948717948723392, -6.376774720514415407, 20.00140224358974095 ) ) ;
#71714 = CARTESIAN_POINT ( 'NONE',  ( -119.5895376238167103, -24.64965694238408034, 8.947790433994649462 ) ) ;
#71715 = FACE_OUTER_BOUND ( 'NONE', #76758, .T. ) ;
#71716 = EDGE_CURVE ( 'NONE', #93143, #11983, #10667, .T. ) ;
#71717 = CIRCLE ( 'NONE', #52299, 1.050000000000000488 ) ;
#71718 = DIRECTION ( 'NONE',  ( -0.000000000000000000, 1.000000000000000000, -0.000000000000000000 ) ) ;
#71719 = CARTESIAN_POINT ( 'NONE',  ( -17.62575346185542102, 8.740161020289619387, -1.500000000000002220 ) ) ;
#71721 = EDGE_LOOP ( 'NONE', ( #73687, #43188, #43469, #91047 ) ) ;
#71720 = LOCAL_TIME ( 0, 54, 15.00000000000000000, #59254 ) ;
#71722 = CARTESIAN_POINT ( 'NONE',  ( -7.543271203275294212, -10.70368373228984460, 1.194479805693834162 ) ) ;
#71723 = CARTESIAN_POINT ( 'NONE',  ( -100.6228709571500559, -29.50248789122583659, 2.256150453626215580 ) ) ;
#71724 = VECTOR ( 'NONE', #13655, 1000.000000000000114 ) ;
#71725 = PERSON_AND_ORGANIZATION ( #70597, #27821 ) ;
#71726 = ADVANCED_FACE ( 'NONE', ( #51226 ), #82170, .F. ) ;
#71727 = CARTESIAN_POINT ( 'NONE',  ( 3.045412351277957175, -6.376774720514422512, 20.90433128744512814 ) ) ;
#71728 = CARTESIAN_POINT ( 'NONE',  ( -90.52287095715006160, -23.47596703998600631, 11.44779298504228393 ) ) ;
#71729 = CARTESIAN_POINT ( 'NONE',  ( -114.5228709571500616, -24.64898659630529565, 1.056161002820831474 ) ) ;
#71730 = CARTESIAN_POINT ( 'NONE',  ( -76.52287095715006160, -24.51283580621364067, 0.6167428607019798115 ) ) ;
#71731 = CARTESIAN_POINT ( 'NONE',  ( -80.91469753264981080, -25.03722721891040948, 7.590183713343859218 ) ) ;
#71732 = CARTESIAN_POINT ( 'NONE',  ( -50.40445135320379677, -25.19502912051677868, 3.293943094755626078 ) ) ;
#71733 = CARTESIAN_POINT ( 'NONE',  ( -121.6228709571500275, -23.73934037231757799, 11.05740245334328087 ) ) ;
#71734 = AXIS2_PLACEMENT_3D ( 'NONE', #84263, #86152, #29475 ) ;
#71735 = CARTESIAN_POINT ( 'NONE',  ( -78.62287095715005592, -29.50250243563736774, 8.947779886222141599 ) ) ;
#71736 = CARTESIAN_POINT ( 'NONE',  ( -19.52388446859773552, -3.948942086532154061, 11.49999999999998934 ) ) ;
#71737 = EDGE_CURVE ( 'NONE', #79772, #37238, #21254, .T. ) ;
#71738 = CARTESIAN_POINT ( 'NONE',  ( -75.49987233357580863, -24.52399227489127043, 9.353111116836526406 ) ) ;
#71739 = CARTESIAN_POINT ( 'NONE',  ( 15.03354914759215966, -12.96403794047452607, -1.500000000000002220 ) ) ;
#71740 = ORIENTED_EDGE ( 'NONE', *, *, #87111, .F. ) ;
#71741 = DIRECTION ( 'NONE',  ( 0.000000000000000000, 0.000000000000000000, -1.000000000000000000 ) ) ;
#71742 = CARTESIAN_POINT ( 'NONE',  ( -51.52764846858840997, -25.25773520710183817, 6.187572766161611781 ) ) ;
#71743 = LINE ( 'NONE', #2237, #86388 ) ;
#71744 = CARTESIAN_POINT ( 'NONE',  ( -19.11632921840048738, -8.121837694355717119, 11.49999999999999645 ) ) ;
#71745 = DIRECTION ( 'NONE',  ( 2.338552693767719605E-15, 0.000000000000000000, 1.000000000000000000 ) ) ;
#71746 = APPROVAL ( #39757, 'UNSPECIFIED' ) ;
#71747 = CARTESIAN_POINT ( 'NONE',  ( -56.62287095715005592, -24.65952944569304250, 1.056160979905693464 ) ) ;
#71748 = CARTESIAN_POINT ( 'NONE',  ( -17.51746294255814718, -14.55262482891283504, 11.49999999999999645 ) ) ;
#71749 = CIRCLE ( 'NONE', #31245, 10.20000000000000107 ) ;
#71750 = VERTEX_POINT ( 'NONE', #99382 ) ;
#71751 = B_SPLINE_SURFACE_WITH_KNOTS ( 'NONE', 3, 3, ( 
 ( #94879, #4047, #48734, #25371 ),
 ( #79653, #71563, #3550, #19253 ),
 ( #34989, #49733, #10152, #72069 ),
 ( #2550, #3054, #42124, #33484 ),
 ( #56350, #87269, #49236, #80165 ),
 ( #81163, #72559, #33995, #26878 ),
 ( #64972, #50720, #26380, #57350 ) ),
 .UNSPECIFIED., .F., .F., .F.,
 ( 4, 3, 4 ),
 ( 4, 4 ),
 ( 0.0004766839783839493675, 0.1029713700210903582, 0.2054660560637967537 ),
 ( 0.7796923376582600707, 0.7810648108262568945 ),
 .UNSPECIFIED. ) ;
#71752 = CARTESIAN_POINT ( 'NONE',  ( -111.6228709571500843, -23.47596703998600631, 11.44779298504227860 ) ) ;
#71753 = CARTESIAN_POINT ( 'NONE',  ( -90.92287095715006728, -23.47596703998600631, 11.44779298504227860 ) ) ;
#71754 = VERTEX_POINT ( 'NONE', #61347 ) ;
#71755 = CARTESIAN_POINT ( 'NONE',  ( -20.01257119864951051, 2.908879540851186274, -1.500000000000002220 ) ) ;
#71756 = CARTESIAN_POINT ( 'NONE',  ( -4.929522925832178437, 5.965225279485572685, -28.63504101147568903 ) ) ;
#71757 = CARTESIAN_POINT ( 'NONE',  ( -97.62287095715002749, -23.72773821059535848, 11.05748984161097503 ) ) ;
#71758 = AXIS2_PLACEMENT_3D ( 'NONE', #33706, #40811, #25586 ) ;
#71759 = VERTEX_POINT ( 'NONE', #28377 ) ;
#71760 = CARTESIAN_POINT ( 'NONE',  ( -25.92875734969025814, -3.316774720514426456, 26.43402280011862615 ) ) ;
#71761 = CARTESIAN_POINT ( 'NONE',  ( -10.13340495651384288, 4.304508339349029988, 30.35717091805029355 ) ) ;
#71762 = CARTESIAN_POINT ( 'NONE',  ( -11.57650325489309395, -16.32560983125179277, -1.500000000000002220 ) ) ;
#71763 = FACE_OUTER_BOUND ( 'NONE', #27340, .T. ) ;
#71764 = CIRCLE ( 'NONE', #94427, 6.594667762285751245 ) ;
#71765 = CARTESIAN_POINT ( 'NONE',  ( 5.463070048063013218, -20.23478146675526190, 11.49999999999999645 ) ) ;
#71766 = CARTESIAN_POINT ( 'NONE',  ( -29.78625860165176320, -25.23684457897835287, 5.682942667385789903 ) ) ;
#71767 = CARTESIAN_POINT ( 'NONE',  ( -124.6228709571500417, -23.95044443724992433, 10.65354141964649415 ) ) ;
#71768 = CARTESIAN_POINT ( 'NONE',  ( 4.500060333422437608, -21.59917750860068963, 11.49999999999998934 ) ) ;
#71769 = CARTESIAN_POINT ( 'NONE',  ( -10.58858228176428717, 5.965225279485594001, -27.03148018517017093 ) ) ;
#71770 = ORIENTED_EDGE ( 'NONE', *, *, #38947, .T. ) ;
#71771 = CARTESIAN_POINT ( 'NONE',  ( -26.09636659181000695, -24.95932275238217102, 4.940287574183225061 ) ) ;
#71772 = DIRECTION ( 'NONE',  ( -0.2164396139380966033, 0.9762960071199348056, 0.000000000000000000 ) ) ;
#71773 = CARTESIAN_POINT ( 'NONE',  ( -50.62287095715005592, -24.99132157543083821, 2.256160258750667502 ) ) ;
#71774 = EDGE_LOOP ( 'NONE', ( #38392, #81902, #10608, #73197 ) ) ;
#71775 = CARTESIAN_POINT ( 'NONE',  ( 3.398951772795901771, -6.376774720514402972, 18.23562605320997676 ) ) ;
#71776 = B_SPLINE_CURVE_WITH_KNOTS ( 'NONE', 3,
 ( #22401, #38640, #46260, #68601, #31529, #77189 ),
 .UNSPECIFIED., .F., .F.,
 ( 4, 2, 4 ),
 ( 1.570887131794638196E-05, 0.001396322306279759555, 0.002776935741241572803 ),
 .UNSPECIFIED. ) ;
#71777 = ORIENTED_EDGE ( 'NONE', *, *, #73316, .T. ) ;
#71778 = ORIENTED_EDGE ( 'NONE', *, *, #71798, .T. ) ;
#71779 = EDGE_CURVE ( 'NONE', #32503, #79100, #91264, .T. ) ;
#71780 = CARTESIAN_POINT ( 'NONE',  ( 26.73860345374794534, 1.682774720514426114, -1.352392034746782823 ) ) ;
#71781 = CARTESIAN_POINT ( 'NONE',  ( -101.1996739087839075, -25.10935851964410759, 3.060140785615252046 ) ) ;
#71782 = LINE ( 'NONE', #95109, #76261 ) ;
#71783 = CARTESIAN_POINT ( 'NONE',  ( 9.245221688665949955, -18.36014492602614467, -1.500000000000002220 ) ) ;
#71784 = ORIENTED_EDGE ( 'NONE', *, *, #59512, .F. ) ;
#71785 = CARTESIAN_POINT ( 'NONE',  ( -100.3681461616303636, -25.30369546473245634, 5.218539490501125755 ) ) ;
#71786 = CARTESIAN_POINT ( 'NONE',  ( 21.57151214508649772, -0.8999999999999998002, 1.500000000000000666 ) ) ;
#71787 = CARTESIAN_POINT ( 'NONE',  ( -53.01255352321339842, 4.772774720514425972, 35.59556822165056644 ) ) ;
#71788 = CARTESIAN_POINT ( 'NONE',  ( -22.28969446433750434, -1.297463027894488086, 11.49999999999998934 ) ) ;
#71790 = CARTESIAN_POINT ( 'NONE',  ( -0.05748996396964648620, -22.30574723846597962, 8.909134979017297340 ) ) ;
#71789 = VECTOR ( 'NONE', #2608, 1000.000000000000000 ) ;
#71791 = CARTESIAN_POINT ( 'NONE',  ( -1.428094109758638819, -5.876774720514416295, 20.04104409779160179 ) ) ;
#71792 = ORIENTED_EDGE ( 'NONE', *, *, #53122, .T. ) ;
#71793 = DIRECTION ( 'NONE',  ( 0.000000000000000000, 0.000000000000000000, 1.000000000000000000 ) ) ;
#71794 = CARTESIAN_POINT ( 'NONE',  ( -4.209565145052936330, 8.865772972990910716, 1.700000000000008837 ) ) ;
#71795 = CC_DESIGN_APPROVAL ( #15255, ( #91265 ) ) ;
#71796 = EDGE_CURVE ( 'NONE', #26914, #61766, #59336, .T. ) ;
#71797 = CARTESIAN_POINT ( 'NONE',  ( -6.911038104174170194, -19.68591361114308214, 11.49999999999998934 ) ) ;
#71798 = EDGE_CURVE ( 'NONE', #34509, #79503, #50124, .T. ) ;
#71799 = ORIENTED_EDGE ( 'NONE', *, *, #25862, .F. ) ;
#71801 = VERTEX_POINT ( 'NONE', #90285 ) ;
#71800 = CARTESIAN_POINT ( 'NONE',  ( -116.5228709571499905, -23.48783264083416711, -1.443836473375476270 ) ) ;
#71802 = EDGE_LOOP ( 'NONE', ( #87971, #80260, #78399, #20339 ) ) ;
#71803 = AXIS2_PLACEMENT_3D ( 'NONE', #81089, #41536, #58749 ) ;
#71804 = DIRECTION ( 'NONE',  ( -1.000000000000000000, 0.000000000000000000, 0.000000000000000000 ) ) ;
#71805 = CARTESIAN_POINT ( 'NONE',  ( 16.43158684610488862, 13.14696595092960152, -1.500000000000002220 ) ) ;
#71806 = ORIENTED_EDGE ( 'NONE', *, *, #37780, .T. ) ;
#71807 = CARTESIAN_POINT ( 'NONE',  ( -69.52287095715003318, -24.66019654487199375, 8.947790411086119278 ) ) ;
#71808 = DIRECTION ( 'NONE',  ( 0.000000000000000000, -1.000000000000000000, 0.000000000000000000 ) ) ;
#71809 = CARTESIAN_POINT ( 'NONE',  ( -120.5520467162983067, -25.00182538069147142, 7.747789668545046027 ) ) ;
#71810 = VECTOR ( 'NONE', #95251, 1000.000000000000114 ) ;
#71811 = CARTESIAN_POINT ( 'NONE',  ( -86.55835959473523644, -23.73791477778911840, 11.05961554403170766 ) ) ;
#71812 = CARTESIAN_POINT ( 'NONE',  ( -59.53837624874798706, -24.51314013834316441, 0.6176544820404136216 ) ) ;
#71813 = CARTESIAN_POINT ( 'NONE',  ( 21.21565077533257337, 4.556159429511043690, -1.500000000000002220 ) ) ;
#71814 = CARTESIAN_POINT ( 'NONE',  ( -63.55620429048339304, -24.64898659630528144, 1.056161002820822370 ) ) ;
#71816 = ORIENTED_EDGE ( 'NONE', *, *, #93018, .T. ) ;
#71815 = CARTESIAN_POINT ( 'NONE',  ( 21.95989154999629278, -3.605859658025859282, 11.49999999999999645 ) ) ;
#71817 = EDGE_CURVE ( 'NONE', #99053, #64340, #52228, .T. ) ;
#71818 = CARTESIAN_POINT ( 'NONE',  ( -51.02375840103924531, -25.31441758376955065, 5.363929648462054445 ) ) ;
#71819 = CARTESIAN_POINT ( 'NONE',  ( -69.52287095715006160, -23.48786465467241058, 11.44779295918254647 ) ) ;
#71820 = ORIENTED_EDGE ( 'NONE', *, *, #78715, .F. ) ;
#71821 = CARTESIAN_POINT ( 'NONE',  ( 4.697487806458584991, -22.17256498326293013, 11.49999999999998934 ) ) ;
#71823 = VERTEX_POINT ( 'NONE', #60848 ) ;
#71822 = CYLINDRICAL_SURFACE ( 'NONE', #89619, 22.69500000000000384 ) ;
#71824 = ORIENTED_EDGE ( 'NONE', *, *, #4444, .T. ) ;
#71825 = CARTESIAN_POINT ( 'NONE',  ( 30.61866831821571111, -5.272393720821680674, 0.8164977272573440414 ) ) ;
#71826 = CARTESIAN_POINT ( 'NONE',  ( 17.11712468798820908, 10.61635618877791742, -1.500000000000002220 ) ) ;
#71827 = CARTESIAN_POINT ( 'NONE',  ( -36.62287095715005592, -24.66019654487199020, 8.947790411086138818 ) ) ;
#71828 = ORIENTED_EDGE ( 'NONE', *, *, #68252, .F. ) ;
#71829 = CARTESIAN_POINT ( 'NONE',  ( -130.5728709571500588, -24.90664209387383110, 1.540770492762566057 ) ) ;
#71830 = CARTESIAN_POINT ( 'NONE',  ( -16.61153998044026991, -15.06042057022924929, -1.500000000000002220 ) ) ;
#71831 = ORIENTED_EDGE ( 'NONE', *, *, #44099, .T. ) ;
#71832 = VERTEX_POINT ( 'NONE', #29376 ) ;
#71833 = DIRECTION ( 'NONE',  ( -0.000000000000000000, 1.000000000000000000, -0.000000000000000000 ) ) ;
#71835 = CARTESIAN_POINT ( 'NONE',  ( -101.5105846445331679, -24.51419770103158413, 9.386484678747175181 ) ) ;
#71834 = VECTOR ( 'NONE', #54442, 1000.000000000000000 ) ;
#71836 = CARTESIAN_POINT ( 'NONE',  ( -39.78092239315489564, -25.31507905443482542, 4.883898260817319148 ) ) ;
#71837 = DIRECTION ( 'NONE',  ( -3.773278334453079030E-23, 0.9999999999976377785, 2.173523156925979128E-06 ) ) ;
#71838 = CARTESIAN_POINT ( 'NONE',  ( -30.60524947077498936, -24.47827083238275492, 0.5637492489085982328 ) ) ;
#71839 = EDGE_CURVE ( 'NONE', #79516, #11582, #69524, .T. ) ;
#71840 = CARTESIAN_POINT ( 'NONE',  ( -19.30006219055749739, -3.230038287793697283, -1.500000000000002220 ) ) ;
#71841 = AXIS2_PLACEMENT_3D ( 'NONE', #21420, #28546, #59515 ) ;
#71842 = CARTESIAN_POINT ( 'NONE',  ( -46.50655037741685760, -23.96119346886880308, -0.6495511937832144644 ) ) ;
#71843 = EDGE_LOOP ( 'NONE', ( #97231, #70267, #40455, #37625 ) ) ;
#71844 = CARTESIAN_POINT ( 'NONE',  ( 20.53733210929814845, -6.371126427052321795, 11.49999999999998934 ) ) ;
#71845 = CARTESIAN_POINT ( 'NONE',  ( -128.5903318345393984, -23.48783264082479150, -1.443836473390056829 ) ) ;
#71846 = DIRECTION ( 'NONE',  ( -1.000000000000000000, 0.000000000000000000, 0.000000000000000000 ) ) ;
#71847 = CARTESIAN_POINT ( 'NONE',  ( -51.93149462243456327, -25.24900417239232908, 6.174051150523328424 ) ) ;
#71848 = CARTESIAN_POINT ( 'NONE',  ( -77.62287095715007013, -24.35013146730204525, 9.818937971375111928 ) ) ;
#71849 = CARTESIAN_POINT ( 'NONE',  ( -22.60589916338503613, 3.847557683979087706, -1.500000000000002220 ) ) ;
#71850 = EDGE_CURVE ( 'NONE', #39979, #11739, #53731, .T. ) ;
#71851 = ADVANCED_FACE ( 'NONE', ( #22248 ), #91279, .F. ) ;
#71852 = DATE_AND_TIME ( #48013, #18124 ) ;
#71853 = DIRECTION ( 'NONE',  ( 0.000000000000000000, -0.9999999999976377785, -2.173523156925979128E-06 ) ) ;
#71854 = CARTESIAN_POINT ( 'NONE',  ( -42.52287095715005449, -24.65952944569303895, 1.056160979905691910 ) ) ;
#71855 = CARTESIAN_POINT ( 'NONE',  ( -18.49208213979201076, -7.923680710433813168, 11.49999999999999645 ) ) ;
#71856 = CARTESIAN_POINT ( 'NONE',  ( -110.2646033073992129, -25.10927396522695432, 2.833559977893872261 ) ) ;
#71857 = LINE ( 'NONE', #80458, #63071 ) ;
#71858 = CARTESIAN_POINT ( 'NONE',  ( -99.52287095715006160, -24.65952944569304961, 1.056160979905702346 ) ) ;
#71859 = CARTESIAN_POINT ( 'NONE',  ( -38.55620429048339304, -24.64965694238574656, 8.947790433994203596 ) ) ;
#71860 = DIRECTION ( 'NONE',  ( 0.000000000000000000, -0.000000000000000000, -1.000000000000000000 ) ) ;
#71861 = CARTESIAN_POINT ( 'NONE',  ( 13.50462702941046977, 14.53317887778067252, -1.500000000000002220 ) ) ;
#71862 = CARTESIAN_POINT ( 'NONE',  ( 17.47290450027814757, -12.96279059203284767, 11.49999999999998934 ) ) ;
#71863 = CARTESIAN_POINT ( 'NONE',  ( -90.62287095715009855, -24.52323809116983355, 9.355190652339423707 ) ) ;
#71864 = CARTESIAN_POINT ( 'NONE',  ( 10.71975780190685690, -16.47196428025586812, -1.500000000000002220 ) ) ;
#71865 = CARTESIAN_POINT ( 'NONE',  ( -42.64758970778231628, -23.96119346886880663, -0.6495511937831991434 ) ) ;
#71866 = AXIS2_PLACEMENT_3D ( 'NONE', #19308, #36037, #67011 ) ;
#71867 = LINE ( 'NONE', #94685, #64598 ) ;
#71868 = DATE_AND_TIME ( #41413, #5210 ) ;
#71869 = DIRECTION ( 'NONE',  ( 0.000000000000000000, 0.000000000000000000, -1.000000000000000000 ) ) ;
#71870 = CARTESIAN_POINT ( 'NONE',  ( 3.262959013008915665, -20.29835246810489835, 11.49999999999999645 ) ) ;
#71871 = CARTESIAN_POINT ( 'NONE',  ( 6.727764423076923350, -6.376774720514413630, 19.76442307692307665 ) ) ;
#71872 = EDGE_CURVE ( 'NONE', #81148, #20503, #70790, .T. ) ;
#71873 = CARTESIAN_POINT ( 'NONE',  ( -42.62287095715004881, -24.65952944569303895, 1.056160979905691688 ) ) ;
#71874 = EDGE_CURVE ( 'NONE', #21858, #68694, #29620, .T. ) ;
#71875 = AXIS2_PLACEMENT_3D ( 'NONE', #1353, #32288, #17060 ) ;
#71876 = CARTESIAN_POINT ( 'NONE',  ( -22.13905560727926414, 4.690293145198261904, 11.49999999999999645 ) ) ;
#71877 = ORIENTED_EDGE ( 'NONE', *, *, #69043, .F. ) ;
#71878 = DIRECTION ( 'NONE',  ( -1.000000000000000000, -2.464095846557964090E-17, 0.000000000000000000 ) ) ;
#71879 = CARTESIAN_POINT ( 'NONE',  ( -31.62287095715005236, -29.50250786944525672, 11.44777988621624409 ) ) ;
#71880 = CARTESIAN_POINT ( 'NONE',  ( -109.6228709571500701, -23.72773821059536559, 11.05748984161097503 ) ) ;
#71881 = DIRECTION ( 'NONE',  ( 0.000000000000000000, 0.000000000000000000, -1.000000000000000000 ) ) ;
#71882 = AXIS2_PLACEMENT_3D ( 'NONE', #39496, #79550, #2946 ) ;
#71883 = CARTESIAN_POINT ( 'NONE',  ( -110.6228709571500417, -23.84081130438200802, 10.88220057463248835 ) ) ;
#71884 = CARTESIAN_POINT ( 'NONE',  ( -28.52287095715006870, -24.18853882557989010, 9.819127037903783162 ) ) ;
#71885 = EDGE_CURVE ( 'NONE', #4386, #98717, #38988, .T. ) ;
#71886 = EDGE_CURVE ( 'NONE', #39047, #63950, #100363, .T. ) ;
#71887 = ORIENTED_EDGE ( 'NONE', *, *, #58902, .T. ) ;
#71888 = CARTESIAN_POINT ( 'NONE',  ( 20.31487730549432413, -11.01532776123576518, 11.49999999999999645 ) ) ;
#71889 = CARTESIAN_POINT ( 'NONE',  ( -10.82450569625279613, 20.10975305113172951, -1.500000000000002220 ) ) ;
#71890 = CARTESIAN_POINT ( 'NONE',  ( -110.9788531467586381, -25.21179375825580493, 3.492134297454125846 ) ) ;
#71891 = CARTESIAN_POINT ( 'NONE',  ( 31.04236049493789906, 5.965225279485572685, 19.84760796525321780 ) ) ;
#71892 = CARTESIAN_POINT ( 'NONE',  ( -63.59272554027524649, -24.15620529776628089, 10.23563542870660470 ) ) ;
#71893 = CARTESIAN_POINT ( 'NONE',  ( -22.46026885398333661, -0.8929446408661095846, 11.49999999999999645 ) ) ;
#71894 = ORIENTED_EDGE ( 'NONE', *, *, #96979, .F. ) ;
#71895 = DIRECTION ( 'NONE',  ( 0.000000000000000000, 0.000000000000000000, 1.000000000000000000 ) ) ;
#71896 = CARTESIAN_POINT ( 'NONE',  ( -21.97012646571106842, -0.5360883523215664859, -1.500000000000002220 ) ) ;
#71897 = B_SPLINE_CURVE_WITH_KNOTS ( 'NONE', 3,
 ( #62215, #16511, #70319, #91639, #61222, #46981 ),
 .UNSPECIFIED., .F., .F.,
 ( 4, 2, 4 ),
 ( 0.001731663773559584266, 0.004550964303235467343, 0.007370264832911350636 ),
 .UNSPECIFIED. ) ;
#71898 = CARTESIAN_POINT ( 'NONE',  ( -126.3656671591979688, -25.31826104724057913, 3.540018580561483663 ) ) ;
#71899 = FACE_OUTER_BOUND ( 'NONE', #49988, .T. ) ;
#71900 = FACE_BOUND ( 'NONE', #33886, .T. ) ;
#71901 = VERTEX_POINT ( 'NONE', #85160 ) ;
#71902 = DIRECTION ( 'NONE',  ( 0.000000000000000000, 0.9999999999976377785, 2.173523156925979128E-06 ) ) ;
#71903 = LINE ( 'NONE', #97227, #73775 ) ;
#71904 = ORIENTED_EDGE ( 'NONE', *, *, #81071, .F. ) ;
#71905 = CARTESIAN_POINT ( 'NONE',  ( 10.70087849588422380, -17.49211976490306597, 11.49999999999998934 ) ) ;
#71906 =( BOUNDED_SURFACE ( )  B_SPLINE_SURFACE ( 3, 2, ( 
 ( #15079, #60278, #46046 ),
 ( #84090, #54165, #91203 ),
 ( #76465, #7459, #69872 ),
 ( #45049, #29305, #38418 ),
 ( #22676, #14071, #69371 ),
 ( #47044, #21676, #100290 ),
 ( #77959, #83586, #30808 ),
 ( #61774, #99312, #92692 ) ),
 .UNSPECIFIED., .F., .F., .T. ) 
 B_SPLINE_SURFACE_WITH_KNOTS ( ( 4, 2, 2, 4 ),
 ( 3, 3 ),
 ( 0.04217399329892001364, 0.04593451325143335651, 0.04781477322769002447, 0.04969503320394669937 ),
 ( 0.000000000000000000, 1.000000000000000000 ),
 .UNSPECIFIED. ) 
 GEOMETRIC_REPRESENTATION_ITEM ( )  RATIONAL_B_SPLINE_SURFACE ( (
 ( 1.000000000000000000, 0.7071067811865475727, 1.000000000000000000),
 ( 1.000000000000000000, 0.7337798844374378016, 1.000000000000000000),
 ( 1.000000000000000000, 0.7590275050786486899, 1.000000000000000000),
 ( 1.000000000000000000, 0.7948576648490734975, 1.000000000000000000),
 ( 1.000000000000000000, 0.8064603411375558251, 1.000000000000000000),
 ( 1.000000000000000000, 0.8289835611541060967, 1.000000000000000000),
 ( 1.000000000000000000, 0.8399042809640585583, 1.000000000000000000),
 ( 1.000000000000000000, 0.8504728678901986028, 1.000000000000000000) ) ) 
 REPRESENTATION_ITEM ( '' )  SURFACE ( )  );
#71907 = ORIENTED_EDGE ( 'NONE', *, *, #17760, .F. ) ;
#71908 = ORIENTED_EDGE ( 'NONE', *, *, #32063, .F. ) ;
#71909 = ORIENTED_EDGE ( 'NONE', *, *, #66447, .F. ) ;
#71910 = EDGE_LOOP ( 'NONE', ( #79425, #36841, #73736, #94420, #96632, #5395 ) ) ;
#71911 = EDGE_CURVE ( 'NONE', #72639, #42765, #6615, .T. ) ;
#71912 = DIRECTION ( 'NONE',  ( 0.000000000000000000, 0.000000000000000000, -1.000000000000000000 ) ) ;
#71913 = CARTESIAN_POINT ( 'NONE',  ( 21.75596283627254479, -7.788036635067100200, 11.49999999999998934 ) ) ;
#71914 = CARTESIAN_POINT ( 'NONE',  ( -63.62287095715007723, -23.47596703998600631, 11.44779298504227683 ) ) ;
#71915 = CARTESIAN_POINT ( 'NONE',  ( 17.42226438573850800, -10.51879874471254261, -1.500000000000002220 ) ) ;
#71916 = VECTOR ( 'NONE', #75289, 1000.000000000000114 ) ;
#71917 = ORIENTED_EDGE ( 'NONE', *, *, #90033, .T. ) ;
#71918 = PLANE ( 'NONE',  #93100 ) ;
#71919 = CARTESIAN_POINT ( 'NONE',  ( -29.52490032455085611, -24.57700738376806626, 8.947790440257527678 ) ) ;
#71920 = LINE ( 'NONE', #24718, #78838 ) ;
#71921 = FACE_OUTER_BOUND ( 'NONE', #80137, .T. ) ;
#71923 = VERTEX_POINT ( 'NONE', #9541 ) ;
#71922 = CARTESIAN_POINT ( 'NONE',  ( 7.253797376210795456, 20.28272692992397808, 11.49999999999999645 ) ) ;
#71924 = CARTESIAN_POINT ( 'NONE',  ( -29.17364183714287762, -24.76881193471582066, 3.835941365018065596 ) ) ;
#71926 = VECTOR ( 'NONE', #9046, 1000.000000000000000 ) ;
#71925 = FACE_OUTER_BOUND ( 'NONE', #59801, .T. ) ;
#71927 = ORIENTED_EDGE ( 'NONE', *, *, #40914, .T. ) ;
#71928 = CARTESIAN_POINT ( 'NONE',  ( -12.26507114386991226, -16.75673120704366426, -1.500000000000002220 ) ) ;
#71929 = EDGE_CURVE ( 'NONE', #64230, #50455, #23252, .T. ) ;
#71930 = ORIENTED_EDGE ( 'NONE', *, *, #43418, .F. ) ;
#71932 = VERTEX_POINT ( 'NONE', #16148 ) ;
#71931 = CARTESIAN_POINT ( 'NONE',  ( -125.5204591733787822, -24.40034930558991633, 0.3402023900116222244 ) ) ;
#71933 = EDGE_CURVE ( 'NONE', #74167, #46180, #64875, .T. ) ;
#71934 = CARTESIAN_POINT ( 'NONE',  ( 14.76093561896379214, 6.475225279485573360, -27.88148769130088667 ) ) ;
#71935 = CARTESIAN_POINT ( 'NONE',  ( -0.02075734969026423599, -6.376774720514426953, -0.08597719988137648983 ) ) ;
#71936 = ORIENTED_EDGE ( 'NONE', *, *, #62784, .F. ) ;
#71937 = ORIENTED_EDGE ( 'NONE', *, *, #3766, .T. ) ;
#71938 = FACE_OUTER_BOUND ( 'NONE', #23761, .T. ) ;
#71939 = CARTESIAN_POINT ( 'NONE',  ( -27.83739072329610664, -5.965225279485592225, -8.084349702057698650 ) ) ;
#71940 = CARTESIAN_POINT ( 'NONE',  ( -29.80801515927848655, -25.24993384078980085, 4.570450481866611625 ) ) ;
#71942 = ORIENTED_EDGE ( 'NONE', *, *, #53662, .T. ) ;
#71941 = CARTESIAN_POINT ( 'NONE',  ( 15.63414672909509839, 15.54323407889855879, 11.49999999999999645 ) ) ;
#71943 = EDGE_CURVE ( 'NONE', #47459, #49734, #52634, .T. ) ;
#71944 = LINE ( 'NONE', #81042, #38180 ) ;
#71945 = CARTESIAN_POINT ( 'NONE',  ( -3.174168706971715270, 22.36591850054903929, -1.500000000000002220 ) ) ;
#71946 = EDGE_CURVE ( 'NONE', #51976, #41756, #75608, .T. ) ;
#71948 = EDGE_LOOP ( 'NONE', ( #59799, #61415, #86615, #34360, #49690 ) ) ;
#71947 = CARTESIAN_POINT ( 'NONE',  ( -79.73149462243461016, -25.13069340115296058, 2.947789388436138580 ) ) ;
#71949 = EDGE_LOOP ( 'NONE', ( #23442, #32891, #9092, #34844 ) ) ;
#71950 = CARTESIAN_POINT ( 'NONE',  ( -72.62287095715005592, -29.50250243563736774, 8.947779886222143375 ) ) ;
#71951 = CIRCLE ( 'NONE', #99440, 1.000000000000000000 ) ;
#71952 = CARTESIAN_POINT ( 'NONE',  ( -46.52287095715006160, -29.50247984919015209, -1.443849546365058689 ) ) ;
#71953 = ORIENTED_EDGE ( 'NONE', *, *, #92161, .F. ) ;
#71954 = CARTESIAN_POINT ( 'NONE',  ( 21.03498508994548999, -2.205306954651367946, -1.500000000000002220 ) ) ;
#71955 = CARTESIAN_POINT ( 'NONE',  ( -34.62287095715005592, -24.35013146730203459, 9.818937971375117257 ) ) ;
#71956 = CARTESIAN_POINT ( 'NONE',  ( -61.66125566941204994, -25.29489609436098263, 6.057563354383567855 ) ) ;
#71957 = CARTESIAN_POINT ( 'NONE',  ( 6.600000000000001421, 0.000000000000000000, 0.000000000000000000 ) ) ;
#71958 = CARTESIAN_POINT ( 'NONE',  ( -80.62287095715008434, -24.52323809116982289, 9.355190652339425483 ) ) ;
#71959 = CARTESIAN_POINT ( 'NONE',  ( -13.35739915041183323, 17.77566839534079435, -1.500000000000002220 ) ) ;
#71960 = VECTOR ( 'NONE', #29273, 1000.000000000000000 ) ;
#71961 = PLANE ( 'NONE',  #38666 ) ;
#71962 = ORIENTED_EDGE ( 'NONE', *, *, #100154, .T. ) ;
#71963 = CARTESIAN_POINT ( 'NONE',  ( -5.576690828732316696, -6.376774720514417183, 20.34213149456667935 ) ) ;
#71964 = DIRECTION ( 'NONE',  ( 0.000000000000000000, 0.000000000000000000, 1.000000000000000000 ) ) ;
#71965 = CARTESIAN_POINT ( 'NONE',  ( -17.77321681866180469, -7.816401696202086136, 11.49999999999999645 ) ) ;
#71966 = CARTESIAN_POINT ( 'NONE',  ( -36.49753981958003379, -24.15620529776627379, 10.23563542870660825 ) ) ;
#71967 = CARTESIAN_POINT ( 'NONE',  ( 12.66784028006542151, -2.682774720514427003, -27.12025593822526304 ) ) ;
#71968 = EDGE_CURVE ( 'NONE', #2798, #21553, #63356, .T. ) ;
#71969 = CARTESIAN_POINT ( 'NONE',  ( -10.96721834449554933, 16.09610527815933168, -1.500000000000002220 ) ) ;
#71970 = CARTESIAN_POINT ( 'NONE',  ( 9.091334071971768793, -19.38302982324925239, 11.49999999999998934 ) ) ;
#71971 = CARTESIAN_POINT ( 'NONE',  ( -32.62287095715004881, -24.64965695001467694, 8.947790433994189385 ) ) ;
#71972 = DIRECTION ( 'NONE',  ( 3.773278334444167608E-23, -1.000000000000000000, 0.000000000000000000 ) ) ;
#71973 = CARTESIAN_POINT ( 'NONE',  ( -51.63915335351398994, -24.15543982623907127, -0.2315651400026664530 ) ) ;
#71974 = CARTESIAN_POINT ( 'NONE',  ( -52.62287095715005592, -23.48786465467240703, 11.44779295918255002 ) ) ;
#71975 = CARTESIAN_POINT ( 'NONE',  ( -20.44213351528904354, 10.05872170072450977, -1.500000000000002220 ) ) ;
#71976 = DIRECTION ( 'NONE',  ( -1.804726700711574591E-28, -1.000000000000000000, -3.334835254233795279E-28 ) ) ;
#71977 = CARTESIAN_POINT ( 'NONE',  ( -106.5125960639114027, -24.51419770103158768, 9.386484678747164523 ) ) ;
#71978 = CARTESIAN_POINT ( 'NONE',  ( 31.79364159983995464, -6.376774720514426953, -11.59305536555894278 ) ) ;
#71979 = CARTESIAN_POINT ( 'NONE',  ( 12.81631318294326505, -15.22695477405695996, 11.49999999999999645 ) ) ;
#71980 = CARTESIAN_POINT ( 'NONE',  ( -123.6253775573720475, -23.96169478059714919, 10.65365249895717348 ) ) ;
#71981 = B_SPLINE_CURVE_WITH_KNOTS ( 'NONE', 3,
 ( #95918, #72098, #56381, #3584, #43140, #80196, #2583, #10687, #34025, #81697, #48762, #26412 ),
 .UNSPECIFIED., .F., .F.,
 ( 4, 2, 2, 2, 2, 4 ),
 ( 8.673617379884035472E-19, 0.002088620103345146476, 0.003132930155017719064, 0.004177240206690291217, 0.006265860310035430321, 0.008354480413380570292 ),
 .UNSPECIFIED. ) ;
#71982 = CARTESIAN_POINT ( 'NONE',  ( -128.5228709571500758, -23.47596703998600631, 11.44779298504227683 ) ) ;
#71983 = DIRECTION ( 'NONE',  ( -3.773278334453080206E-23, 0.9999999999976377785, 2.173523156925979975E-06 ) ) ;
#71984 = ORIENTED_EDGE ( 'NONE', *, *, #75688, .F. ) ;
#71985 = CARTESIAN_POINT ( 'NONE',  ( 30.42805396430595977, 4.988345540211635232, 19.84760796525322135 ) ) ;
#71986 = CARTESIAN_POINT ( 'NONE',  ( -32.99704036429253762, -25.31558585043574183, 4.997857581739419075 ) ) ;
#71987 = B_SPLINE_CURVE_WITH_KNOTS ( 'NONE', 3,
 ( #83923, #4317, #75802, #20030, #5302, #50995 ),
 .UNSPECIFIED., .F., .F.,
 ( 4, 2, 4 ),
 ( 0.000000000000000000, 0.001380764517854763014, 0.002761529035709526028 ),
 .UNSPECIFIED. ) ;
#71988 = AXIS2_PLACEMENT_3D ( 'NONE', #13327, #67646, #43308 ) ;
#71989 = DIRECTION ( 'NONE',  ( 1.000000000000000000, 3.773278334444167608E-23, 8.201307833595939069E-29 ) ) ;
#71990 = CARTESIAN_POINT ( 'NONE',  ( 9.217229664113554932, 19.63635308506117383, -1.500000000000002220 ) ) ;
#71991 = CARTESIAN_POINT ( 'NONE',  ( -51.72093146136422348, -25.16667630403369671, 6.901880236027385429 ) ) ;
#71992 = CARTESIAN_POINT ( 'NONE',  ( 5.544562197198338538, -18.70016399976332977, -1.500000000000002220 ) ) ;
#71993 = DIRECTION ( 'NONE',  ( -0.000000000000000000, -1.000000000000000000, -0.000000000000000000 ) ) ;
#71994 = VERTEX_POINT ( 'NONE', #934 ) ;
#71995 = AXIS2_PLACEMENT_3D ( 'NONE', #29574, #45805, #14338 ) ;
#71996 = CARTESIAN_POINT ( 'NONE',  ( -14.54385459823299875, 14.27422344363935025, 11.49999999999999645 ) ) ;
#71997 = CARTESIAN_POINT ( 'NONE',  ( -49.58953762381671737, -23.47596703998600276, 11.44779298504227505 ) ) ;
#71998 = CARTESIAN_POINT ( 'NONE',  ( 14.52511747680497933, 6.475225279485573360, -27.86035006098926559 ) ) ;
#71999 = EDGE_CURVE ( 'NONE', #65732, #15617, #25262, .T. ) ;
#72000 = ORIENTED_EDGE ( 'NONE', *, *, #79118, .F. ) ;
#72001 = CARTESIAN_POINT ( 'NONE',  ( -0.07965933291641426328, -22.01874733586428690, 9.960208392924579712 ) ) ;
#72002 = CARTESIAN_POINT ( 'NONE',  ( 6.660000000000001030, -10.15233964170348457, 1.310587897985993955 ) ) ;
#72003 = CARTESIAN_POINT ( 'NONE',  ( 30.57287095715005520, -6.475225279485573360, 25.41160796525322141 ) ) ;
#72004 = CARTESIAN_POINT ( 'NONE',  ( -125.5562042904833646, -23.48786465467241413, 11.44779295918253581 ) ) ;
#72005 = CARTESIAN_POINT ( 'NONE',  ( -1.041963229364719634, -5.876774720514417183, 20.24089781925592746 ) ) ;
#72006 = CARTESIAN_POINT ( 'NONE',  ( 21.57151214508649772, 3.625915217019311583E-15, 0.5000000000000000000 ) ) ;
#72007 = ORIENTED_EDGE ( 'NONE', *, *, #11318, .F. ) ;
#72008 = EDGE_CURVE ( 'NONE', #20514, #31485, #36814, .T. ) ;
#72009 = CARTESIAN_POINT ( 'NONE',  ( -4.141025641025638748, -6.376774720514427841, 21.75000000000000355 ) ) ;
#72010 = EDGE_CURVE ( 'NONE', #73650, #62726, #48118, .T. ) ;
#72011 = ADVANCED_FACE ( 'NONE', ( #87166 ), #8544, .F. ) ;
#72012 = CARTESIAN_POINT ( 'NONE',  ( -21.13427563780003382, 8.902639844219676135, 11.49999999999999645 ) ) ;
#72013 = CARTESIAN_POINT ( 'NONE',  ( 21.73672277138745201, -6.736064506363727666, -1.500000000000002220 ) ) ;
#72014 = CARTESIAN_POINT ( 'NONE',  ( -71.54080034593859239, -25.17052887806732997, 6.883280112116211491 ) ) ;
#72015 = CARTESIAN_POINT ( 'NONE',  ( -77.62287095715005592, -29.50247984919015209, -1.443849546365053582 ) ) ;
#72016 = CARTESIAN_POINT ( 'NONE',  ( -90.54280940977186276, -24.83618233451451118, 1.606449574219535492 ) ) ;
#72017 = EDGE_CURVE ( 'NONE', #69295, #52438, #55239, .T. ) ;
#72018 = CARTESIAN_POINT ( 'NONE',  ( -69.39514063290955903, -25.22191518979476754, 6.510382875654499912 ) ) ;
#72019 = CARTESIAN_POINT ( 'NONE',  ( -6.606886629844116676, -20.84447163495035937, -1.500000000000002220 ) ) ;
#72020 = CARTESIAN_POINT ( 'NONE',  ( -69.59245699313737532, -24.15620529776627734, 10.23563542870660825 ) ) ;
#72021 = LINE ( 'NONE', #64427, #36339 ) ;
#72022 = DIRECTION ( 'NONE',  ( 1.000000000000000000, 0.000000000000000000, 0.000000000000000000 ) ) ;
#72023 = CARTESIAN_POINT ( 'NONE',  ( -40.22287095715007155, -23.47593901973090169, -1.443836447538997980 ) ) ;
#72024 = ORIENTED_EDGE ( 'NONE', *, *, #3859, .T. ) ;
#72025 = CARTESIAN_POINT ( 'NONE',  ( -18.16121111207539940, 9.348575961806686152, 11.49999999999998934 ) ) ;
#72026 = EDGE_LOOP ( 'NONE', ( #38467, #12329, #14450, #36914, #59222, #77967, #53478, #11519, #95612, #62042, #21453, #58002, #12699, #15477, #88612, #16439, #1992, #3376, #11753, #67608, #36835, #39950, #71777, #46119, #60711, #64018, #75037, #92824, #40214, #3161, #86884, #516, #35518, #98459, #54257, #66845, #77507, #3188, #11022, #9214, #68649, #21885, #7682, #38091, #68564, #42395, #41831, #37330, #1303, #14094, #30726, #99417, #172, #31741, #86233, #6104, #42579, #60325, #99258, #86642, #3790, #37847, #7620, #26833, #16571, #62078, #94352, #60932, #47153, #70149, #88618, #80802, #65390, #76899, #97125, #65336, #85902, #52254, #51330, #71009, #41941, #80422, #17352, #36615, #33991, #45380, #12121, #89379, #77621, #35595, #61021, #78530, #9992, #27615, #70671, #61196, #60461, #64591, #6267, #26356, #12964, #4393, #76110, #39089, #26136, #82002, #63520, #15964, #2088, #6532, #277, #49584, #17411, #100265, #57967, #55681, #47798, #62661, #97346, #80277, #298, #58012, #10031, #15783, #52268, #49380, #71064, #46561, #91786, #34857, #32960, #68299, #11731, #53147, #27845, #90271, #19307, #22716, #97614, #56590, #46186, #43374, #11109, #71147, #84610, #32834, #10669, #48593, #9844, #36942, #27501, #96096, #37820, #90931, #17769, #54799, #44061, #91719, #96990, #3687, #61113, #54061, #84897, #89142, #48586, #64837, #89054, #62224, #54038, #93591, #22204, #72556, #72040, #72104, #34433, #47589, #60452, #90611, #67928, #3411, #1180, #22668, #30964, #94276, #62428, #95672, #254, #81324, #44818, #3134, #29861, #57333, #85986, #59389, #19009, #55918, #63273, #75274, #48986, #7747, #56354, #9884, #54422, #3812, #67285, #51792, #21739, #61381, #41043, #73403, #19940, #100076, #73895, #17296, #66566, #98463, #16870, #1938, #16197, #58168, #95498, #8787, #98829, #66116, #16586, #6262, #12225, #97794, #75599, #63609, #49856, #13501, #29728, #49975, #21478, #92376, #46080, #54630, #30399, #78728, #44191, #52879, #15503, #36553, #9409, #20229, #21626, #21220, #56975, #97020, #34946, #42037, #28860, #80031, #48746, #97347, #6357, #49164, #55577, #81489, #34456, #20878, #32724, #13131, #19623, #45192, #95385, #50200, #88051, #24746, #44816, #74292, #8241, #100081, #68529, #80002, #16589, #12398, #9766, #33184, #73176, #45071, #33254, #2172, #59171, #83712, #31482, #51686, #34259, #41580, #66055, #17355, #93853, #68891, #79622, #47067, #96390, #91298, #38358, #95245, #7119, #73784, #68914, #78460, #63969, #54943, #13392, #68468, #42682, #29982, #68798, #61412, #25368, #98251, #21091, #5262, #85499, #46304, #13253, #35585, #25718, #29864, #39032, #96504, #36572, #7082, #7468, #29189, #26724, #84506, #87491, #74520, #70127, #81599, #42268, #92537, #83467, #84128, #42209, #20206, #78363, #24896, #31431, #20615, #42620, #51418, #23566, #83294, #85822, #16973, #19901, #70947, #49343, #8196, #31576, #789, #10509, #34986, #60842, #95983, #25055, #56744, #75846, #66809, #72542, #48401, #27972, #37846, #36708, #55975, #2210, #80419, #28409, #88136, #75921, #53829, #97246, #71877, #6205, #70746, #75716, #14788, #30635, #79927, #23203, #2602, #82343, #82372, #18339, #33203, #35479, #46099, #29882, #20626, #74429, #21493, #59201, #89868, #39632, #34745, #64666, #28586, #1768, #19134, #7512, #59938, #79316, #72891, #15351, #73887, #9404, #73759, #86222, #62035, #88708, #60380, #88254, #94381, #68510, #95898, #47475, #14951, #56460, #35849, #27967, #96872, #58083, #93639, #95848, #51712, #1419, #87094, #57885, #83736, #66914, #16243, #19863, #94015, #13872, #12378, #68189, #3821, #7882, #71661, #18224, #58922, #81426, #43871, #17607, #46, #76284, #13997, #47198, #8574, #68032, #82048, #70164, #93717, #69770, #662, #81236, #25573, #78294, #70801, #20958, #87549, #46067, #5988, #98996, #40837, #97254, #20168, #47519, #45582, #20708, #92754, #91247, #64833, #51335, #28756, #22379, #74615, #67195, #66801, #42782, #11354, #67787, #1662, #100334, #61175, #38226, #95934, #22240, #25594, #47412, #82826, #44484, #38939, #50076, #40365, #20898, #461, #72836, #18142, #16952, #62041, #50725, #42318, #59520, #10909, #29972, #75197, #31887, #38176, #7383, #56722, #98968, #49328, #77240, #91113, #24054, #39967, #40761, #9030, #31878, #84323, #53565, #97816, #39245, #44098, #84423, #48949, #88538, #25353, #51700, #92735, #4900, #34807, #74264, #3279, #69112, #35396, #72312, #45485, #41718, #629, #39370, #28595, #1087, #49306, #71831, #58695, #9181, #14635, #52599, #38726, #43525, #16047, #28013, #40607, #60869, #625, #73814, #30979, #55107, #42488, #92632, #64846, #77976, #66915, #31833, #56775, #93584, #2070, #97146, #74631, #46590, #60299, #27026, #84388, #10391, #35418, #16485, #55972, #77409, #74027, #29734, #6523, #20484, #31355, #30842, #10190, #6494, #41735, #21866, #6397, #39055, #65561, #72775, #52533, #20707, #51457, #96345, #87521, #76117, #31177, #72883, #58339, #73026, #97646, #7268, #61924, #53615, #45314, #77750, #97940, #8140, #63572, #61202, #38827, #78236, #39070, #59806, #62955, #66088, #68553, #77649, #48274, #99371, #54970, #22921, #66934, #7650, #69392, #94738, #23953, #3672, #86247, #43473, #66280, #57404, #55275, #56693, #7246, #43086, #38442, #37044, #43943, #43067, #98567, #34587, #11085, #46720, #27046, #27758, #33996, #70906, #93707, #71792, #78106, #93576, #33262, #21880, #53706, #1760, #71022, #5723, #3155, #11078, #3251, #73740, #96052, #86863, #13129, #63443, #39546, #43764, #20750, #23910, #73200, #87133, #58642, #42342, #40100, #92258, #9978, #39075, #54211, #93504, #26951, #41844, #35609, #77829, #15343, #10516, #593, #86523, #44204, #15823, #26973, #67674, #20091, #53567, #82203, #54592, #4909, #92080, #375, #74038, #63199, #4468, #15622, #6157, #96518, #97570, #32743, #73165, #42711, #53087, #47489, #82133, #96316, #25076, #73553, #76988, #12996, #16726, #94307, #34317, #42508, #7508, #2054, #11420, #92646, #95250, #91466, #10408, #74280, #21701, #17383, #42389, #42893, #36983, #56628, #30187, #94719, #12027, #50068, #33223, #41086, #3921, #15755, #31341, #70490, #27584, #63327, #33134, #43722, #34990, #28921, #91620, #41339, #76488, #59449, #31449, #89042, #27411, #36073, #44463, #34873, #19834, #24345, #60550, #66615, #38597, #73382, #9668, #48735, #64717, #99187, #36104, #24165, #90254, #47570, #92637, #10632, #8011, #69531, #10388, #8863, #89909, #35267, #30596, #30446, #10151, #67686 ) ) ;
#72027 = EDGE_LOOP ( 'NONE', ( #17628, #52766, #31986, #90856 ) ) ;
#72028 = EDGE_CURVE ( 'NONE', #87941, #36724, #78536, .T. ) ;
#72029 = CARTESIAN_POINT ( 'NONE',  ( 20.35648204094723468, -10.72454223111430593, 11.49999999999998934 ) ) ;
#72030 = DIRECTION ( 'NONE',  ( -1.000000000000000000, -0.000000000000000000, -0.000000000000000000 ) ) ;
#72031 = VERTEX_POINT ( 'NONE', #1442 ) ;
#72032 = CARTESIAN_POINT ( 'NONE',  ( -65.05438548721848235, -6.475225279485573360, 0.7300228001186309656 ) ) ;
#72033 = CARTESIAN_POINT ( 'NONE',  ( -118.5895376238167245, -24.65952944569304961, 1.056160979905702346 ) ) ;
#72034 = B_SPLINE_CURVE_WITH_KNOTS ( 'NONE', 3,
 ( #24975, #71166, #31085, #53946, #22954, #46321 ),
 .UNSPECIFIED., .F., .F.,
 ( 4, 2, 4 ),
 ( 0.000000000000000000, 0.001380764517854761279, 0.002761529035709522559 ),
 .UNSPECIFIED. ) ;
#72035 = EDGE_CURVE ( 'NONE', #18359, #60162, #32380, .T. ) ;
#72036 = DIRECTION ( 'NONE',  ( -3.773278334453079618E-23, 0.9999999999976377785, 2.173523156925978705E-06 ) ) ;
#72037 = CARTESIAN_POINT ( 'NONE',  ( -13.89275734969026388, -5.965225279485572685, 31.02402280011862246 ) ) ;
#72039 = ORIENTED_EDGE ( 'NONE', *, *, #82022, .T. ) ;
#72038 = CARTESIAN_POINT ( 'NONE',  ( -21.20786952941880443, -2.223526401999901925, 11.49999999999999645 ) ) ;
#72040 = ORIENTED_EDGE ( 'NONE', *, *, #3775, .F. ) ;
#72041 = CARTESIAN_POINT ( 'NONE',  ( -22.15176777451872425, 1.842445310382735624, -1.500000000000002220 ) ) ;
#72042 = CARTESIAN_POINT ( 'NONE',  ( 16.46467569749531634, 12.45148609503053017, 11.49999999999998934 ) ) ;
#72043 = VECTOR ( 'NONE', #38140, 1000.000000000000000 ) ;
#72044 = EDGE_CURVE ( 'NONE', #93818, #46475, #7541, .T. ) ;
#72045 = ORIENTED_EDGE ( 'NONE', *, *, #99069, .T. ) ;
#72046 = CARTESIAN_POINT ( 'NONE',  ( -6.728471858368818559, -5.876774720514408301, 19.14926908420045137 ) ) ;
#72047 = CARTESIAN_POINT ( 'NONE',  ( -71.72404080852884078, -25.30060019737137367, 6.009288023823078362 ) ) ;
#72048 = ORIENTED_EDGE ( 'NONE', *, *, #67143, .F. ) ;
#72049 = CARTESIAN_POINT ( 'NONE',  ( -95.52287095715004739, -23.47593901973090169, -1.443836447538996648 ) ) ;
#72050 = ORIENTED_EDGE ( 'NONE', *, *, #63940, .T. ) ;
#72051 = CARTESIAN_POINT ( 'NONE',  ( 7.681304422638354445, -3.316774720514426900, -28.19747436301255661 ) ) ;
#72052 = DIRECTION ( 'NONE',  ( -0.9890158633619159367, -0.1478094111296165691, -0.000000000000000000 ) ) ;
#72053 = CARTESIAN_POINT ( 'NONE',  ( 11.47802407633690258, -17.41396394059345454, -1.500000000000002220 ) ) ;
#72054 = CARTESIAN_POINT ( 'NONE',  ( -21.73523922981167189, -2.474665994198115726, 11.49999999999999645 ) ) ;
#72055 = EDGE_CURVE ( 'NONE', #61839, #62307, #34385, .T. ) ;
#72056 = VECTOR ( 'NONE', #40956, 1000.000000000000114 ) ;
#72057 = CARTESIAN_POINT ( 'NONE',  ( -8.376690734369036662, 11.49999999999999645, 2.100000000000000089 ) ) ;
#72058 = CARTESIAN_POINT ( 'NONE',  ( -122.5228709571500616, -29.50248528299804818, 1.056150453629045360 ) ) ;
#72059 = CARTESIAN_POINT ( 'NONE',  ( -11.50411854321151672, 19.32100693743031528, 11.49999999999998934 ) ) ;
#72060 = CARTESIAN_POINT ( 'NONE',  ( 8.587038044527741221, -19.06309208085484386, 11.49999999999998934 ) ) ;
#72061 = ADVANCED_FACE ( 'NONE', ( #26768 ), #96281, .T. ) ;
#72062 = CARTESIAN_POINT ( 'NONE',  ( -38.62372276496436996, -24.65952944569304606, 1.056160979905694131 ) ) ;
#72063 = CARTESIAN_POINT ( 'NONE',  ( -72.52287095715010423, -24.66019654487199375, 8.947790411086128159 ) ) ;
#72064 = CARTESIAN_POINT ( 'NONE',  ( 4.948291700218025113, -5.876774720514418071, 20.47145334051262111 ) ) ;
#72065 = EDGE_LOOP ( 'NONE', ( #52287, #3404, #83625, #59362 ) ) ;
#72066 = EDGE_CURVE ( 'NONE', #69390, #22695, #34882, .T. ) ;
#72067 = VERTEX_POINT ( 'NONE', #10041 ) ;
#72068 = ORIENTED_EDGE ( 'NONE', *, *, #18061, .T. ) ;
#72069 = CARTESIAN_POINT ( 'NONE',  ( -52.50767261960347554, -23.96119346886881019, -0.6495511937831939253 ) ) ;
#72070 = ORIENTED_EDGE ( 'NONE', *, *, #50523, .T. ) ;
#72071 = B_SPLINE_CURVE_WITH_KNOTS ( 'NONE', 3,
 ( #17482, #40819, #17986, #49453 ),
 .UNSPECIFIED., .F., .F.,
 ( 4, 4 ),
 ( 0.000000000000000000, 9.999999999998898659E-05 ),
 .UNSPECIFIED. ) ;
#72072 = CARTESIAN_POINT ( 'NONE',  ( 13.27131465344908001, -16.79725507166503462, -1.500000000000002220 ) ) ;
#72073 = CARTESIAN_POINT ( 'NONE',  ( 11.21425909587273928, 19.38466839394011387, 11.49999999999999645 ) ) ;
#72074 = ORIENTED_EDGE ( 'NONE', *, *, #96045, .F. ) ;
#72075 = CARTESIAN_POINT ( 'NONE',  ( 0.06697178475903577122, -6.376774720514410077, 19.29815762497054976 ) ) ;
#72076 = CARTESIAN_POINT ( 'NONE',  ( 20.56459456670464547, 4.482388377596099538, -1.500000000000002220 ) ) ;
#72077 = CARTESIAN_POINT ( 'NONE',  ( -30.45987998222503634, -25.30657267508212271, 5.002391647799127483 ) ) ;
#72078 = CARTESIAN_POINT ( 'NONE',  ( 5.901097582950029619, 19.04237314665466485, -1.500000000000002220 ) ) ;
#72079 = CYLINDRICAL_SURFACE ( 'NONE', #19347, 1.000000000000000222 ) ;
#72080 = DIRECTION ( 'NONE',  ( -3.773278334453080206E-23, 0.9999999999976377785, 2.173523156925979975E-06 ) ) ;
#72081 = CARTESIAN_POINT ( 'NONE',  ( -14.94409825380703616, 16.19114737329946507, -1.500000000000002220 ) ) ;
#72082 = ORIENTED_EDGE ( 'NONE', *, *, #97679, .T. ) ;
#72083 = CARTESIAN_POINT ( 'NONE',  ( -65.48565164118330983, -24.92592662359560762, 8.075495903017996469 ) ) ;
#72084 = CARTESIAN_POINT ( 'NONE',  ( -111.6228709571500701, -23.48786465467241769, 11.44779295918254114 ) ) ;
#72085 = CARTESIAN_POINT ( 'NONE',  ( -63.58953762381672448, -23.47593901973091235, -1.443836447539007972 ) ) ;
#72086 = CARTESIAN_POINT ( 'NONE',  ( -47.52287095715008292, -24.33832256527048088, 0.1851278514138576248 ) ) ;
#72087 = CYLINDRICAL_SURFACE ( 'NONE', #82996, 252.4458649670781085 ) ;
#72088 = AXIS2_PLACEMENT_3D ( 'NONE', #91540, #43392, #28654 ) ;
#72089 = DIRECTION ( 'NONE',  ( 0.000000000000000000, 0.000000000000000000, -1.000000000000000000 ) ) ;
#72090 = CARTESIAN_POINT ( 'NONE',  ( 3.515848477382193416, 21.04717058667041130, -1.500000000000002220 ) ) ;
#72091 = CARTESIAN_POINT ( 'NONE',  ( -40.52287095715006870, -29.50250243563736774, 8.947779886222148704 ) ) ;
#72092 = LINE ( 'NONE', #8678, #62715 ) ;
#72093 = CARTESIAN_POINT ( 'NONE',  ( -17.97250661212648026, -0.3587747205144057872, -23.43622901028613725 ) ) ;
#72094 = DIRECTION ( 'NONE',  ( -0.000000000000000000, 2.173523156925979552E-06, -0.9999999999976378895 ) ) ;
#72095 = CARTESIAN_POINT ( 'NONE',  ( -19.94007547503736788, -10.58355046294204094, -1.500000000000002220 ) ) ;
#72096 = DIRECTION ( 'NONE',  ( -1.000000000000000000, 0.000000000000000000, 0.000000000000000000 ) ) ;
#72097 = ORIENTED_EDGE ( 'NONE', *, *, #90288, .T. ) ;
#72098 = CARTESIAN_POINT ( 'NONE',  ( 5.959527149828093506, 3.316774720514425567, -28.45540529974545407 ) ) ;
#72099 = CARTESIAN_POINT ( 'NONE',  ( -120.5228709571500616, -23.47596703998600631, 11.44779298504227860 ) ) ;
#72100 = CARTESIAN_POINT ( 'NONE',  ( -17.62575346185542102, 8.740161020289619387, 11.49999999999999645 ) ) ;
#72101 = LINE ( 'NONE', #2586, #27757 ) ;
#72102 = DIRECTION ( 'NONE',  ( 1.000000000000000000, 3.389844910009033029E-15, 0.000000000000000000 ) ) ;
#72103 = B_SPLINE_CURVE_WITH_KNOTS ( 'NONE', 3,
 ( #88598, #10461, #41421, #64788 ),
 .UNSPECIFIED., .F., .F.,
 ( 4, 4 ),
 ( 0.000000000000000000, 9.999999999998206125E-05 ),
 .UNSPECIFIED. ) ;
#72104 = ORIENTED_EDGE ( 'NONE', *, *, #95524, .F. ) ;
#72105 = DIRECTION ( 'NONE',  ( 3.773278334444165844E-23, -1.000000000000000000, 0.000000000000000000 ) ) ;
#72106 = CARTESIAN_POINT ( 'NONE',  ( -127.4728709571500360, -25.40675522342679926, 5.000950437786769953 ) ) ;
#72107 = CARTESIAN_POINT ( 'NONE',  ( 5.550000000000004263, -2.000000000000001776, 18.24068255301867936 ) ) ;
#72108 = CARTESIAN_POINT ( 'NONE',  ( -88.58953762381671027, -23.47593901973091235, -1.443836447539002865 ) ) ;
#72109 = DIRECTION ( 'NONE',  ( 0.000000000000000000, 0.000000000000000000, -1.000000000000000000 ) ) ;
#72110 = PLANE ( 'NONE',  #38323 ) ;
#72111 = CARTESIAN_POINT ( 'NONE',  ( -19.76903914530799966, 0.2396048511829373395, 11.49999999999998934 ) ) ;
#72112 = ORIENTED_EDGE ( 'NONE', *, *, #8867, .T. ) ;
#72113 = CARTESIAN_POINT ( 'NONE',  ( 3.706880958665978998, 19.89330832657401515, 11.49999999999999645 ) ) ;
#72114 = CARTESIAN_POINT ( 'NONE',  ( -6.818021687177533430, -5.876774720514409189, 19.14905311829361167 ) ) ;
#72115 = AXIS2_PLACEMENT_3D ( 'NONE', #73989, #4485, #35433 ) ;
#72116 = ORIENTED_EDGE ( 'NONE', *, *, #32875, .T. ) ;
#72117 = DIRECTION ( 'NONE',  ( -0.9997753877537054468, 0.000000000000000000, 0.02119372647572819943 ) ) ;
#72118 = CARTESIAN_POINT ( 'NONE',  ( -69.34303308397305443, -25.24554880456021522, 6.209207408033732278 ) ) ;
#72119 = CARTESIAN_POINT ( 'NONE',  ( -50.51883597636249590, -25.30394825761364785, 5.202350221066103231 ) ) ;
#72120 = CARTESIAN_POINT ( 'NONE',  ( -82.62287095715005592, -24.64898659630367916, 1.056161002820826145 ) ) ;
#72121 = ADVANCED_FACE ( 'NONE', ( #26269, #81054 ), #41500, .F. ) ;
#72122 = CARTESIAN_POINT ( 'NONE',  ( -28.47875734969025885, 5.965225279485572685, -0.08597719988137300651 ) ) ;
#72123 = EDGE_CURVE ( 'NONE', #80787, #34855, #21173, .T. ) ;
#72124 = CARTESIAN_POINT ( 'NONE',  ( -120.5228709571500616, -23.48786465467241769, 11.44779295918253759 ) ) ;
#72125 = CARTESIAN_POINT ( 'NONE',  ( -19.63739455291241498, 3.909132673056371132, 11.49999999999998934 ) ) ;
#72126 = CIRCLE ( 'NONE', #760, 1.000000000000000444 ) ;
#72127 = EDGE_CURVE ( 'NONE', #15143, #90740, #33882, .T. ) ;
#72128 = CARTESIAN_POINT ( 'NONE',  ( -117.6228709571500559, -24.64898659630368627, 1.056161002820833028 ) ) ;
#72129 = ORIENTED_EDGE ( 'NONE', *, *, #25599, .F. ) ;
#72130 = ADVANCED_FACE ( 'NONE', ( #42011 ), #65858, .T. ) ;
#72131 = EDGE_CURVE ( 'NONE', #50353, #27980, #57508, .T. ) ;
#72132 = CARTESIAN_POINT ( 'NONE',  ( -73.62287095715007013, -24.33927499327854704, 9.819080762295822495 ) ) ;
#72133 = CARTESIAN_POINT ( 'NONE',  ( -35.64144378499706534, -24.52300882791529446, 0.6510814631126419227 ) ) ;
#72134 = LINE ( 'NONE', #71625, #37046 ) ;
#72135 = CARTESIAN_POINT ( 'NONE',  ( -119.4728709571500644, -25.40558663563398056, 5.000950440326719537 ) ) ;
#72136 = CARTESIAN_POINT ( 'NONE',  ( -101.6837879195638124, -25.23386281078603943, 3.681742193200927105 ) ) ;
#72137 = DIRECTION ( 'NONE',  ( 0.000000000000000000, 1.000000000000000000, 0.000000000000000000 ) ) ;
#72138 = CARTESIAN_POINT ( 'NONE',  ( -98.87408511115022236, -25.31392319263090585, 5.203681702801228326 ) ) ;
#72139 = ORIENTED_EDGE ( 'NONE', *, *, #79386, .T. ) ;
#72140 = CARTESIAN_POINT ( 'NONE',  ( 19.34776771173714849, 6.126202725962671458, 11.49999999999998934 ) ) ;
#72141 = ORIENTED_EDGE ( 'NONE', *, *, #77818, .T. ) ;
#72142 = EDGE_CURVE ( 'NONE', #92874, #96665, #56251, .T. ) ;
#72143 = CARTESIAN_POINT ( 'NONE',  ( 29.72095141006403196, 6.296447751620394939, 26.96056093718771152 ) ) ;
#72144 = CARTESIAN_POINT ( 'NONE',  ( -96.52287095715007581, -23.47593901973090524, -1.443836447538996648 ) ) ;
#72145 = CARTESIAN_POINT ( 'NONE',  ( -59.50358786707867154, -24.15620529776628089, 10.23563542870661180 ) ) ;
#72146 = CARTESIAN_POINT ( 'NONE',  ( -86.52287095715009002, -23.96177878511310055, 10.65340807706330217 ) ) ;
#72147 = EDGE_CURVE ( 'NONE', #51300, #45390, #81560, .T. ) ;
#72148 = CARTESIAN_POINT ( 'NONE',  ( -30.47287095715006444, -25.29799310117780919, 4.442956538296639835 ) ) ;
#72149 = CARTESIAN_POINT ( 'NONE',  ( 6.139388171429570384, 20.22809724653347985, 11.49999999999999645 ) ) ;
#72150 = VECTOR ( 'NONE', #55393, 1000.000000000000114 ) ;
#72151 = CARTESIAN_POINT ( 'NONE',  ( 10.50125231818214289, 19.49540335892314502, 11.49999999999998934 ) ) ;
#72152 = CARTESIAN_POINT ( 'NONE',  ( -19.32567751138619982, -7.045664331180771178, -1.500000000000002220 ) ) ;
#72153 = EDGE_LOOP ( 'NONE', ( #34970, #10997, #87894, #42385 ) ) ;
#72154 = CARTESIAN_POINT ( 'NONE',  ( 29.68479148105952703, -1.682774720514426114, -9.431263391055123790 ) ) ;
#72155 = VERTEX_POINT ( 'NONE', #49126 ) ;
#72156 = CARTESIAN_POINT ( 'NONE',  ( -54.63281596392198480, -24.34968618360932879, 0.1864209137778771175 ) ) ;
#72157 = CARTESIAN_POINT ( 'NONE',  ( -80.52287095715006160, -23.47593901973090169, -1.443836447538996648 ) ) ;
#72158 = EDGE_LOOP ( 'NONE', ( #90537, #66825, #75588 ) ) ;
#72159 = VERTEX_POINT ( 'NONE', #27766 ) ;
#72160 = B_SPLINE_CURVE_WITH_KNOTS ( 'NONE', 3,
 ( #32000, #39611, #70562, #55354 ),
 .UNSPECIFIED., .F., .F.,
 ( 4, 4 ),
 ( 0.000000000000000000, 1.000000000000000000 ),
 .UNSPECIFIED. ) ;
#72161 = VERTEX_POINT ( 'NONE', #58716 ) ;
#72162 = CARTESIAN_POINT ( 'NONE',  ( -111.7078649355182023, -25.26111664902047238, 3.848907687874172812 ) ) ;
#72163 = PLANE ( 'NONE',  #97271 ) ;
#72164 = CARTESIAN_POINT ( 'NONE',  ( 6.156881756163101294, -6.376774720514413630, 19.74809127057764968 ) ) ;
#72165 = CARTESIAN_POINT ( 'NONE',  ( -4.968023186724614959, -20.10795263665959709, -1.500000000000002220 ) ) ;
#72166 = CARTESIAN_POINT ( 'NONE',  ( -11.49108604648090548, 18.38894055434275643, 11.49999999999999645 ) ) ;
#72167 = ORIENTED_EDGE ( 'NONE', *, *, #85601, .F. ) ;
#72168 = CARTESIAN_POINT ( 'NONE',  ( -60.52287095715007581, -25.00182538069855198, 7.747789668514453609 ) ) ;
#72169 = CARTESIAN_POINT ( 'NONE',  ( 2.747717285871495108, -5.876774720514405637, 18.94713297040818034 ) ) ;
#72170 = CARTESIAN_POINT ( 'NONE',  ( 21.16571772479873204, -7.350578744355993344, -1.500000000000002220 ) ) ;
#72171 = ADVANCED_FACE ( 'NONE', ( #17655 ), #80053, .F. ) ;
#72172 = CARTESIAN_POINT ( 'NONE',  ( -7.160000000000000142, 7.891155995661685019, 5.788828319098143993 ) ) ;
#72173 = CARTESIAN_POINT ( 'NONE',  ( -27.68651082257922980, -24.78174777341091328, 2.274903344755643708 ) ) ;
#72174 = EDGE_LOOP ( 'NONE', ( #17862, #41999, #22198, #83034 ) ) ;
#72175 = FACE_OUTER_BOUND ( 'NONE', #95549, .T. ) ;
#72176 = CARTESIAN_POINT ( 'NONE',  ( -35.67969092473991566, -23.48786465467240703, 11.44779295918255180 ) ) ;
#72177 = ORIENTED_EDGE ( 'NONE', *, *, #43189, .F. ) ;
#72178 = ORIENTED_EDGE ( 'NONE', *, *, #44079, .F. ) ;
#72179 = ADVANCED_FACE ( 'NONE', ( #60227 ), #62110, .T. ) ;
#72180 = AXIS2_PLACEMENT_3D ( 'NONE', #50024, #88577, #72355 ) ;
#72181 = CARTESIAN_POINT ( 'NONE',  ( -70.62287095715007013, -23.47596703998600631, 11.44779298504227505 ) ) ;
#72182 = ORIENTED_EDGE ( 'NONE', *, *, #12213, .F. ) ;
#72183 = PLANE ( 'NONE',  #73015 ) ;
#72184 = CARTESIAN_POINT ( 'NONE',  ( -20.82729772986975547, -4.079710536234080642, -1.500000000000002220 ) ) ;
#72185 = ORIENTED_EDGE ( 'NONE', *, *, #74077, .F. ) ;
#72186 = CARTESIAN_POINT ( 'NONE',  ( -88.54318482745297558, -24.65952944569304606, 1.056160979905701902 ) ) ;
#72187 = CARTESIAN_POINT ( 'NONE',  ( -11.22809577558575000, 18.72649003030000259, -1.500000000000002220 ) ) ;
#72188 = CARTESIAN_POINT ( 'NONE',  ( -103.5530466354624508, -24.15620529776628445, 10.23563542870660292 ) ) ;
#72189 = DIRECTION ( 'NONE',  ( 0.000000000000000000, -1.000000000000000000, 0.000000000000000000 ) ) ;
#72190 = DIRECTION ( 'NONE',  ( 3.773278334444166432E-23, -1.000000000000000000, 0.000000000000000000 ) ) ;
#72191 = CARTESIAN_POINT ( 'NONE',  ( 19.28182042344761626, 10.37885539243483812, -1.500000000000002220 ) ) ;
#72192 = CARTESIAN_POINT ( 'NONE',  ( 6.944081373883786767, -6.376774720514424288, 21.27829155525578031 ) ) ;
#72193 = ORIENTED_EDGE ( 'NONE', *, *, #94113, .F. ) ;
#72194 = FACE_BOUND ( 'NONE', #8154, .T. ) ;
#72195 = LINE ( 'NONE', #1175, #67060 ) ;
#72196 = VECTOR ( 'NONE', #24607, 999.9999999999998863 ) ;
#72197 = ORIENTED_EDGE ( 'NONE', *, *, #42916, .T. ) ;
#72198 = FACE_OUTER_BOUND ( 'NONE', #46372, .T. ) ;
#72199 = VERTEX_POINT ( 'NONE', #37379 ) ;
#72200 = CARTESIAN_POINT ( 'NONE',  ( 5.885012508251304730, 6.475225279485574248, -27.43431635654696521 ) ) ;
#72201 = LINE ( 'NONE', #41758, #54613 ) ;
#72202 = B_SPLINE_CURVE_WITH_KNOTS ( 'NONE', 3,
 ( #60854, #92278, #90791, #22755, #76048, #90290 ),
 .UNSPECIFIED., .F., .F.,
 ( 4, 2, 4 ),
 ( 0.0005551796157830859177, 0.008843260483942988470, 0.01713134135210289330 ),
 .UNSPECIFIED. ) ;
#72203 = CARTESIAN_POINT ( 'NONE',  ( 21.11169859150035677, 2.410084449224629832, 11.49999999999998934 ) ) ;
#72204 = CARTESIAN_POINT ( 'NONE',  ( 8.978253834636468866, -5.876774720514426953, 21.48128695274316158 ) ) ;
#72205 = CARTESIAN_POINT ( 'NONE',  ( -40.43801387148943149, -25.26938797564855932, 6.123095479407366426 ) ) ;
#72206 = PLANE ( 'NONE',  #77783 ) ;
#72207 = CARTESIAN_POINT ( 'NONE',  ( -112.6228709571500559, -29.50248528299804818, 1.056150453629043584 ) ) ;
#72208 = CARTESIAN_POINT ( 'NONE',  ( -13.34961138979462270, 14.11212085816309880, 11.49999999999998934 ) ) ;
#72209 = CARTESIAN_POINT ( 'NONE',  ( -80.62287095715004170, -23.48786465467241058, 11.44779295918254469 ) ) ;
#72210 = EDGE_LOOP ( 'NONE', ( #46315, #19584, #31935, #75000 ) ) ;
#72211 = CARTESIAN_POINT ( 'NONE',  ( 16.96702763494397104, -9.608290155750392358, 11.49999999999999645 ) ) ;
#72212 = CYLINDRICAL_SURFACE ( 'NONE', #77842, 27.94799999999999685 ) ;
#72213 = CARTESIAN_POINT ( 'NONE',  ( 282.9764569301858046, 5.152774720514427642, 20.79159422840526616 ) ) ;
#72214 = VERTEX_POINT ( 'NONE', #90656 ) ;
#72215 = CARTESIAN_POINT ( 'NONE',  ( -58.62287095715004881, -23.72773821059535848, 11.05748984161097503 ) ) ;
#72216 = CARTESIAN_POINT ( 'NONE',  ( -89.59466492980996577, -23.96119346886881019, -0.6495511937831908167 ) ) ;
#72217 = B_SPLINE_CURVE_WITH_KNOTS ( 'NONE', 3,
 ( #53300, #77111, #92345, #29951, #44689, #98956, #22818, #38061 ),
 .UNSPECIFIED., .F., .F.,
 ( 4, 2, 2, 4 ),
 ( 0.000000000000000000, 0.002001098010032686253, 0.003001647015049031114, 0.004002196020065375975 ),
 .UNSPECIFIED. ) ;
#72218 = DIRECTION ( 'NONE',  ( -1.838928956454364527E-13, 0.000000000000000000, -1.000000000000000000 ) ) ;
#72219 = CARTESIAN_POINT ( 'NONE',  ( -81.13115756185166560, -25.03156031351837996, 7.427330859781487327 ) ) ;
#72220 = CARTESIAN_POINT ( 'NONE',  ( -14.15603575923578283, -13.64839490926926580, -1.500000000000002220 ) ) ;
#72221 = ORIENTED_EDGE ( 'NONE', *, *, #94187, .F. ) ;
#72222 = AXIS2_PLACEMENT_3D ( 'NONE', #59897, #67015, #90828 ) ;
#72223 = CARTESIAN_POINT ( 'NONE',  ( -78.52287095715009002, -23.96127896941631974, -0.6493128931038031348 ) ) ;
#72224 = CARTESIAN_POINT ( 'NONE',  ( -14.75821945985506645, 17.75411527500383002, -1.500000000000002220 ) ) ;
#72225 = SHAPE_DEFINITION_REPRESENTATION ( #96842, #37291 ) ;
#72226 = CARTESIAN_POINT ( 'NONE',  ( 3.128267882468583228, -5.876774720514423400, 21.08409277973916218 ) ) ;
#72227 = CARTESIAN_POINT ( 'NONE',  ( -83.62287095715005592, -29.50250243563736774, 8.947779886222141599 ) ) ;
#72228 = CARTESIAN_POINT ( 'NONE',  ( -108.9545715455115129, -25.27705962214097113, 4.170144839539424275 ) ) ;
#72229 = CARTESIAN_POINT ( 'NONE',  ( -97.51608334452220106, -23.96169478059713853, 10.65365249895717703 ) ) ;
#72230 = CARTESIAN_POINT ( 'NONE',  ( -114.6228709571500417, -24.65952944569305316, 1.056160979905703234 ) ) ;
#72231 = ADVANCED_FACE ( 'NONE', ( #60725 ), #76414, .F. ) ;
#72232 = CARTESIAN_POINT ( 'NONE',  ( 5.766314450391940127, -6.376774720514424288, 21.17177008079512035 ) ) ;
#72233 = CARTESIAN_POINT ( 'NONE',  ( -69.34512923434627396, -25.24515217105749443, 6.118189401617559753 ) ) ;
#72234 = CARTESIAN_POINT ( 'NONE',  ( -50.62287095715005592, -23.47593901973091235, -1.443836447539009749 ) ) ;
#72235 = CARTESIAN_POINT ( 'NONE',  ( -19.80664267627650688, 2.137978742899185214, 11.49999999999998934 ) ) ;
#72236 = ADVANCED_FACE ( 'NONE', ( #66846 ), #97768, .F. ) ;
#72237 = CARTESIAN_POINT ( 'NONE',  ( -75.58684609491236017, -24.63419186844611275, 9.035850630976923981 ) ) ;
#72238 = CARTESIAN_POINT ( 'NONE',  ( -19.84341114293531305, -1.032944114202840824, -1.500000000000002220 ) ) ;
#72239 = ORIENTED_EDGE ( 'NONE', *, *, #30630, .F. ) ;
#72240 = PLANE ( 'NONE',  #28118 ) ;
#72241 = ADVANCED_FACE ( 'NONE', ( #52600 ), #30246, .F. ) ;
#72242 = B_SPLINE_CURVE_WITH_KNOTS ( 'NONE', 3,
 ( #48441, #1266, #24082, #9864, #93588, #40814, #71775, #16972, #87492, #8864, #26091, #47936, #2270, #2770, #32698, #39812, #62671, #64183, #18476, #86488, #70770, #95104, #94600, #56057, #57063, #17981, #25589 ),
 .UNSPECIFIED., .F., .F.,
 ( 4, 1, 1, 1, 1, 1, 1, 1, 1, 1, 1, 1, 1, 1, 1, 1, 1, 1, 1, 1, 1, 1, 1, 1, 4 ),
 ( 0.000000000000000000, 0.03378811616271038681, 0.06719393237388025797, 0.09986241085682510954, 0.1325666121262582542, 0.1651511732547865374, 0.1979131873557924692, 0.2313190035669614730, 0.2650832782673732679, 0.2992553087581151794, 0.3343985665049788447, 0.3699428235093072392, 0.4062835607000603866, 0.4440638196985079444, 0.4829977068727749345, 0.5233544466133041029, 0.5655365896041484319, 0.6096129240658189063, 0.6563908113764170826, 0.7058854949364568032, 0.7583245002617304831, 0.8138317829411497728, 0.8727945590393887398, 0.9347222295400740011, 1.000000000000000000 ),
 .UNSPECIFIED. ) ;
#72243 = EDGE_CURVE ( 'NONE', #937, #81281, #87681, .T. ) ;
#72244 = PLANE ( 'NONE',  #84091 ) ;
#72245 = CARTESIAN_POINT ( 'NONE',  ( -93.52287095715006160, -24.66019654487200086, 8.947790411086110396 ) ) ;
#72246 = CARTESIAN_POINT ( 'NONE',  ( 11.22265027773143231, -6.376774720513926908, -28.06709888789093554 ) ) ;
#72247 = CARTESIAN_POINT ( 'NONE',  ( 15.20108283357335921, -14.20388156210760577, 11.49999999999999645 ) ) ;
#72248 = CARTESIAN_POINT ( 'NONE',  ( -37.92287095715006018, -23.47593901973090169, -1.443836447538997980 ) ) ;
#72249 = ADVANCED_FACE ( 'NONE', ( #14018 ), #89667, .T. ) ;
#72250 = CARTESIAN_POINT ( 'NONE',  ( 28.87399897812681004, -1.477225279485574028, -12.57761096169975445 ) ) ;
#72251 = CARTESIAN_POINT ( 'NONE',  ( -16.39533425382319720, 15.89506036719111037, 11.49999999999999645 ) ) ;
#72252 = CIRCLE ( 'NONE', #57630, 21.89999999999999858 ) ;
#72253 = EDGE_LOOP ( 'NONE', ( #40021, #21944, #83514, #89166 ) ) ;
#72254 = LINE ( 'NONE', #49425, #51139 ) ;
#72255 = DIRECTION ( 'NONE',  ( 3.773278334444166432E-23, -1.000000000000000000, 0.000000000000000000 ) ) ;
#72256 = ORIENTED_EDGE ( 'NONE', *, *, #33054, .T. ) ;
#72257 = AXIS2_PLACEMENT_3D ( 'NONE', #12795, #74698, #4705 ) ;
#72258 = CARTESIAN_POINT ( 'NONE',  ( -5.148175472751820081, -19.54457232503198227, -1.500000000000002220 ) ) ;
#72259 = CARTESIAN_POINT ( 'NONE',  ( 7.343377932919765705, -5.876774720514422512, 21.31293098237466310 ) ) ;
#72260 = AXIS2_PLACEMENT_3D ( 'NONE', #100116, #69200, #28771 ) ;
#72261 = CARTESIAN_POINT ( 'NONE',  ( -114.5562042904833930, -24.66019654487199730, 8.947790411086124607 ) ) ;
#72263 = EDGE_CURVE ( 'NONE', #59988, #20176, #23484, .T. ) ;
#72262 = AXIS2_PLACEMENT_3D ( 'NONE', #91856, #7628, #22330 ) ;
#72264 = CARTESIAN_POINT ( 'NONE',  ( -100.6228709571500701, -24.63287334234177450, 0.9662140553045522884 ) ) ;
#72265 = ORIENTED_EDGE ( 'NONE', *, *, #46047, .F. ) ;
#72266 = CARTESIAN_POINT ( 'NONE',  ( -70.62287095715004170, -24.91570333823099759, 8.075032458375549282 ) ) ;
#72267 = CARTESIAN_POINT ( 'NONE',  ( -10.14776687836540070, 4.675267808546679227, 30.20327419389746382 ) ) ;
#72268 = CARTESIAN_POINT ( 'NONE',  ( -10.14125802585430947, 17.27231531754821603, -1.500000000000002220 ) ) ;
#72269 = CARTESIAN_POINT ( 'NONE',  ( 19.40473180639871131, -7.901900427366274293, 11.49999999999999645 ) ) ;
#72270 = CARTESIAN_POINT ( 'NONE',  ( -27.79917671128472634, -24.65826116135614754, 8.250243081618606311 ) ) ;
#72271 = CARTESIAN_POINT ( 'NONE',  ( -70.48669436695099932, -25.00182538069146787, 7.747789668545044250 ) ) ;
#72272 = CARTESIAN_POINT ( 'NONE',  ( 19.60348439636399931, 10.09110264789753053, -1.500000000000002220 ) ) ;
#72273 = CARTESIAN_POINT ( 'NONE',  ( -42.55620429048339304, -24.64898659630528144, 1.056161002820814154 ) ) ;
#72274 = ORIENTED_EDGE ( 'NONE', *, *, #18285, .T. ) ;
#72275 = DIRECTION ( 'NONE',  ( 0.1736481776669262511, 0.9848077530122087975, 0.000000000000000000 ) ) ;
#72276 = CARTESIAN_POINT ( 'NONE',  ( -118.5228709571501184, -24.35013146730205236, 9.818937971375092388 ) ) ;
#72277 = CARTESIAN_POINT ( 'NONE',  ( -50.58953762381673158, -24.99132157543083821, 2.256160258750496084 ) ) ;
#72278 = ORIENTED_EDGE ( 'NONE', *, *, #77232, .F. ) ;
#72279 = PLANE ( 'NONE',  #58338 ) ;
#72280 = ORIENTED_EDGE ( 'NONE', *, *, #75313, .T. ) ;
#72281 = VERTEX_POINT ( 'NONE', #44999 ) ;
#72282 = DIRECTION ( 'NONE',  ( 1.000000000000000000, -0.000000000000000000, 0.000000000000000000 ) ) ;
#72283 = CARTESIAN_POINT ( 'NONE',  ( 32.25249349869194759, -1.477225279485574028, -12.65342752644895263 ) ) ;
#72284 = CARTESIAN_POINT ( 'NONE',  ( -58.62287095715004170, -23.73907113216990794, -1.053371485793233919 ) ) ;
#72285 = CARTESIAN_POINT ( 'NONE',  ( 20.20254288951482735, -3.758238384022974277, -1.500000000000002220 ) ) ;
#72286 = ORIENTED_EDGE ( 'NONE', *, *, #45427, .F. ) ;
#72287 = LINE ( 'NONE', #65690, #54304 ) ;
#72288 = CARTESIAN_POINT ( 'NONE',  ( 7.165897526731081157, -5.876774720514420736, 20.76279523443833597 ) ) ;
#72289 = DIRECTION ( 'NONE',  ( -1.000000000000000000, -0.000000000000000000, 0.000000000000000000 ) ) ;
#72290 = CARTESIAN_POINT ( 'NONE',  ( 16.98343680692684643, -14.46476453587665389, 11.49999999999998934 ) ) ;
#72291 = CARTESIAN_POINT ( 'NONE',  ( -55.52287095715006870, -23.48786465467241058, 11.44779295918254824 ) ) ;
#72292 = ORIENTED_EDGE ( 'NONE', *, *, #84028, .F. ) ;
#72293 = CARTESIAN_POINT ( 'NONE',  ( 29.57907552799941087, 5.965225279485572685, 29.21818156447043791 ) ) ;
#72294 = CARTESIAN_POINT ( 'NONE',  ( -65.55620429048339304, -24.99132157543166599, 2.256160258750668390 ) ) ;
#72295 = CARTESIAN_POINT ( 'NONE',  ( -11.21968731015968856, -17.59241007644406096, -1.500000000000002220 ) ) ;
#72296 = ORIENTED_EDGE ( 'NONE', *, *, #30994, .T. ) ;
#72298 = ORIENTED_EDGE ( 'NONE', *, *, #53757, .F. ) ;
#72297 = FACE_OUTER_BOUND ( 'NONE', #25525, .T. ) ;
#72299 = VERTEX_POINT ( 'NONE', #12532 ) ;
#72300 = CARTESIAN_POINT ( 'NONE',  ( -70.15801421577009478, -25.03149371388890643, 7.556454810261096000 ) ) ;
#72301 = CARTESIAN_POINT ( 'NONE',  ( 20.15827220212406701, 6.050813824765241655, -1.500000000000002220 ) ) ;
#72302 = EDGE_CURVE ( 'NONE', #52789, #43797, #98255, .T. ) ;
#72303 = ORIENTED_EDGE ( 'NONE', *, *, #84407, .T. ) ;
#72304 = CYLINDRICAL_SURFACE ( 'NONE', #4108, 2.349999999999999645 ) ;
#72305 = FACE_OUTER_BOUND ( 'NONE', #88244, .T. ) ;
#72306 = CARTESIAN_POINT ( 'NONE',  ( -120.5177523882421582, -24.63419186844610920, 9.035850630976920428 ) ) ;
#72307 = CARTESIAN_POINT ( 'NONE',  ( -86.51402387307511788, -23.96169478059713498, 10.65365249895717881 ) ) ;
#72308 = CARTESIAN_POINT ( 'NONE',  ( -59.60445504388953708, -23.73766607897669445, -1.055555164236460675 ) ) ;
#72309 = CARTESIAN_POINT ( 'NONE',  ( 19.26462925850498920, -9.998780574493274287, -1.500000000000002220 ) ) ;
#72310 = CARTESIAN_POINT ( 'NONE',  ( 8.160000000000000142, -0.2368809837866518997, 5.288828319098142217 ) ) ;
#72312 = ORIENTED_EDGE ( 'NONE', *, *, #87565, .T. ) ;
#72311 = CARTESIAN_POINT ( 'NONE',  ( -9.338385371603758145, -20.21602636099808237, 11.49999999999999645 ) ) ;
#72313 = CARTESIAN_POINT ( 'NONE',  ( -51.52443300084429723, -25.31441916312803286, 6.090564871685868020 ) ) ;
#72314 = CARTESIAN_POINT ( 'NONE',  ( -30.64427850938830389, -23.56000036390796737, -1.497999999999532594 ) ) ;
#72315 = EDGE_CURVE ( 'NONE', #76871, #1915, #6425, .T. ) ;
#72316 = CARTESIAN_POINT ( 'NONE',  ( -70.48052921158478057, -25.30151219336677570, 5.317344105861852910 ) ) ;
#72317 = ORIENTED_EDGE ( 'NONE', *, *, #10508, .F. ) ;
#72318 = VECTOR ( 'NONE', #18062, 1000.000000000000000 ) ;
#72320 = ORIENTED_EDGE ( 'NONE', *, *, #80950, .F. ) ;
#72319 = CARTESIAN_POINT ( 'NONE',  ( -65.62287095715005592, -29.50248789122583659, 2.256150453626215580 ) ) ;
#72321 = EDGE_LOOP ( 'NONE', ( #49323, #71042, #91249, #74502, #45848, #32242, #13495 ) ) ;
#72322 = LINE ( 'NONE', #2817, #80544 ) ;
#72323 = CC_DESIGN_PERSON_AND_ORGANIZATION_ASSIGNMENT ( #88709, #57282, ( #10919 ) ) ;
#72324 = TOROIDAL_SURFACE ( 'NONE', #35023, 80.18232118519038920, 8.160000000000000142 ) ;
#72325 = CARTESIAN_POINT ( 'NONE',  ( -48.62287095715004881, -23.73907113216990794, -1.053371485793232143 ) ) ;
#72326 = CARTESIAN_POINT ( 'NONE',  ( -66.52287095715006160, -24.33927499327855770, 9.819080762295810061 ) ) ;
#72327 = ORIENTED_EDGE ( 'NONE', *, *, #25735, .F. ) ;
#72328 = VECTOR ( 'NONE', #32713, 1000.000000000000114 ) ;
#72329 = CARTESIAN_POINT ( 'NONE',  ( -130.5728709571500588, -24.45096232750585585, 9.783294602970084242 ) ) ;
#72330 = CARTESIAN_POINT ( 'NONE',  ( 12.67250375155129127, 18.46511205475877304, -1.500000000000002220 ) ) ;
#72331 = VECTOR ( 'NONE', #37210, 1000.000000000000000 ) ;
#72332 = VECTOR ( 'NONE', #84684, 1000.000000000000000 ) ;
#72333 = ORIENTED_EDGE ( 'NONE', *, *, #1438, .T. ) ;
#72334 = VERTEX_POINT ( 'NONE', #53110 ) ;
#72335 = CARTESIAN_POINT ( 'NONE',  ( -112.5222218478034790, -23.48786465467241769, 11.44779295918253936 ) ) ;
#72336 = CARTESIAN_POINT ( 'NONE',  ( -55.62287095715004170, -23.47596703998600631, 11.44779298504227505 ) ) ;
#72337 = DIRECTION ( 'NONE',  ( -1.000000000000000000, -3.773278334444166432E-23, -8.201307841325785021E-29 ) ) ;
#72338 = CARTESIAN_POINT ( 'NONE',  ( -48.62287095715004881, -23.47593901973091235, -1.443836447539009749 ) ) ;
#72339 = AXIS2_PLACEMENT_3D ( 'NONE', #57781, #59778, #83080 ) ;
#72340 = B_SPLINE_CURVE_WITH_KNOTS ( 'NONE', 3,
 ( #49294, #87327, #34554, #41678 ),
 .UNSPECIFIED., .F., .F.,
 ( 4, 4 ),
 ( 1.387778780781445521E-17, 9.999999999997510880E-05 ),
 .UNSPECIFIED. ) ;
#72341 = CARTESIAN_POINT ( 'NONE',  ( -97.23961514226040492, -25.30557784678704536, 3.856996771331004048 ) ) ;
#72342 = CARTESIAN_POINT ( 'NONE',  ( 3.528372621398383924, 19.26332229581237598, -1.500000000000002220 ) ) ;
#72343 = CARTESIAN_POINT ( 'NONE',  ( -59.58953762381671027, -24.65952944569304250, 1.056160979905690134 ) ) ;
#72344 = ORIENTED_EDGE ( 'NONE', *, *, #43157, .F. ) ;
#72345 = CARTESIAN_POINT ( 'NONE',  ( -0.8555947871142663974, 21.52075748220454798, 11.49999999999998934 ) ) ;
#72346 = CARTESIAN_POINT ( 'NONE',  ( 15.97264540888995299, -3.405665504423739609, -27.93485543958162864 ) ) ;
#72347 = CARTESIAN_POINT ( 'NONE',  ( -5.366453405989237702, 1.999999999999993117, 18.24068255301867936 ) ) ;
#72348 = CARTESIAN_POINT ( 'NONE',  ( -100.8359211054894899, -25.12990627727104354, 2.884779682363133535 ) ) ;
#72349 = CARTESIAN_POINT ( 'NONE',  ( 6.026614999332422182E-17, -23.47594215783195537, -5.102550391006585557E-05 ) ) ;
#72350 = CARTESIAN_POINT ( 'NONE',  ( 1.269710630819723463, 22.90746787927615102, -1.500000000000002220 ) ) ;
#72351 = APPROVAL_STATUS ( 'not_yet_approved' ) ;
#72352 = FACE_OUTER_BOUND ( 'NONE', #28733, .T. ) ;
#72353 = CARTESIAN_POINT ( 'NONE',  ( -49.56034765714075263, -23.73766607897670156, -1.055555164236457566 ) ) ;
#72354 = CARTESIAN_POINT ( 'NONE',  ( -20.11654390397962544, -0.4351469013266864860, 11.49999999999999645 ) ) ;
#72355 = DIRECTION ( 'NONE',  ( 0.000000000000000000, 0.000000000000000000, -1.000000000000000000 ) ) ;
#72356 = CARTESIAN_POINT ( 'NONE',  ( 32.45853543194704116, -5.965225279485572685, 9.169203677920338080 ) ) ;
#72357 = B_SPLINE_CURVE_WITH_KNOTS ( 'NONE', 3,
 ( #91119, #76869, #7876, #7372, #29223, #45463, #44461, #23085, #44962, #29722, #14487, #30211, #13985, #76380, #38326, #54075, #68790, #15482, #77375 ),
 .UNSPECIFIED., .F., .F.,
 ( 4, 1, 1, 1, 1, 1, 1, 1, 1, 1, 1, 1, 1, 1, 1, 1, 4 ),
 ( 0.000000000000000000, 0.06867706841303471144, 0.1368709585090958913, 0.2061143571452998258, 0.2775381819697287922, 0.3497719775548993604, 0.4212508361555678538, 0.4929107569233706077, 0.5670265889927378344, 0.6066141532413346082, 0.6497039535189880199, 0.6973031504846840534, 0.7490856597091360980, 0.8048806474593088733, 0.8654850057023349974, 0.9302371271531362229, 1.000000000000000000 ),
 .UNSPECIFIED. ) ;
#72358 = CARTESIAN_POINT ( 'NONE',  ( -7.160000000000000142, -6.754662360505032659, 7.925641719537454222 ) ) ;
#72359 = B_SPLINE_CURVE_WITH_KNOTS ( 'NONE', 3,
 ( #40062, #17214, #42074, #11103, #32950, #41570, #78595, #95342, #18705, #95841, #73019, #49685, #56804, #56305, #25829, #94837, #3010, #79613, #87225, #9606 ),
 .UNSPECIFIED., .F., .F.,
 ( 4, 2, 2, 2, 2, 2, 2, 2, 2, 4 ),
 ( 0.000000000000000000, 0.0004282660737508323275, 0.0008565321475016646549, 0.001284798221252496982, 0.001713064295003329310, 0.002141330368754161637, 0.002569596442504993965, 0.002997862516255826292, 0.003211995553131242673, 0.003426128590006658620 ),
 .UNSPECIFIED. ) ;
#72360 = CARTESIAN_POINT ( 'NONE',  ( 11.95416678406013489, 5.152774720514426754, -26.25966023343078248 ) ) ;
#72361 = CARTESIAN_POINT ( 'NONE',  ( -77.52287095715006160, -29.50250786944525672, 11.44777988621623521 ) ) ;
#72362 = CARTESIAN_POINT ( 'NONE',  ( 19.22361159462649027, -4.937694622890139939, -1.500000000000002220 ) ) ;
#72363 = CARTESIAN_POINT ( 'NONE',  ( -90.62287095715008434, -23.85229601348995843, 10.88205029486209696 ) ) ;
#72364 = CARTESIAN_POINT ( 'NONE',  ( -18.76583335001664565, 6.068782795689376286, -1.500000000000002220 ) ) ;
#72365 = VECTOR ( 'NONE', #90923, 1000.000000000000000 ) ;
#72366 = CARTESIAN_POINT ( 'NONE',  ( 14.83405752585718496, -4.881907540129191148, -27.54622755360254516 ) ) ;
#72367 = CARTESIAN_POINT ( 'NONE',  ( 0.000000000000000000, -16.94322527948557422, 0.000000000000000000 ) ) ;
#72368 = CALENDAR_DATE ( 2026, 9, 10 ) ;
#72369 = EDGE_CURVE ( 'NONE', #93232, #98936, #84041, .T. ) ;
#72370 = CARTESIAN_POINT ( 'NONE',  ( -60.52287095715007581, -23.84081130425356321, 10.88220057483158243 ) ) ;
#72371 = CARTESIAN_POINT ( 'NONE',  ( -39.56136241089613037, -25.29384247623274362, 5.536731341526268224 ) ) ;
#72372 = CARTESIAN_POINT ( 'NONE',  ( 19.88596897151998633, -5.565664080715476913, 11.49999999999999645 ) ) ;
#72373 = DIRECTION ( 'NONE',  ( -0.9994733861282923959, 0.000000000000000000, -0.03244919754393515293 ) ) ;
#72374 = EDGE_CURVE ( 'NONE', #69390, #51679, #45261, .T. ) ;
#72375 = CARTESIAN_POINT ( 'NONE',  ( 5.184553252003285984, 6.475225279485573360, -28.06387035751381731 ) ) ;
#72376 = CARTESIAN_POINT ( 'NONE',  ( -13.31036990564671818, -18.29084955798148471, 11.49999999999999645 ) ) ;
#72377 = ORIENTED_EDGE ( 'NONE', *, *, #64036, .T. ) ;
#72378 = CARTESIAN_POINT ( 'NONE',  ( -69.34303308397305443, -25.12218950775438842, 6.209207676158020384 ) ) ;
#72379 = CARTESIAN_POINT ( 'NONE',  ( -109.6228709571500559, -24.64965695001469115, 8.947790433994176951 ) ) ;
#72380 = CARTESIAN_POINT ( 'NONE',  ( -39.62287095715004170, -24.33832256526968507, 0.1851278514119840124 ) ) ;
#72381 = B_SPLINE_CURVE_WITH_KNOTS ( 'NONE', 3,
 ( #88736, #27823, #64921, #41565 ),
 .UNSPECIFIED., .F., .F.,
 ( 4, 4 ),
 ( 0.000000000000000000, 9.999999999999592548E-05 ),
 .UNSPECIFIED. ) ;
#72382 = EDGE_CURVE ( 'NONE', #86899, #9886, #90008, .T. ) ;
#72383 = CARTESIAN_POINT ( 'NONE',  ( -27.70544111104076990, -24.93063634934924266, 8.251826098080067950 ) ) ;
#72384 = CARTESIAN_POINT ( 'NONE',  ( -2.786875287040666560, -6.376774720514417183, 20.09505574050193388 ) ) ;
#72385 = VECTOR ( 'NONE', #87056, 1000.000000000000000 ) ;
#72386 = ORIENTED_EDGE ( 'NONE', *, *, #16200, .T. ) ;
#72387 = FACE_OUTER_BOUND ( 'NONE', #86409, .T. ) ;
#72388 = CARTESIAN_POINT ( 'NONE',  ( -12.33899560737860313, 19.21699747222852395, -1.500000000000002220 ) ) ;
#72389 = CARTESIAN_POINT ( 'NONE',  ( -98.55620429048337883, -24.64965694238575011, 8.947790433994191162 ) ) ;
#72390 = CARTESIAN_POINT ( 'NONE',  ( -96.55486200352346771, -23.96119346886881019, -0.6495511937832061378 ) ) ;
#72391 = CARTESIAN_POINT ( 'NONE',  ( -63.52208778886303264, -23.48786465467241058, 11.44779295918254824 ) ) ;
#72392 = CARTESIAN_POINT ( 'NONE',  ( 22.48569338394020534, -0.9006126209707296937, 11.49999999999999645 ) ) ;
#72393 = ORIENTED_EDGE ( 'NONE', *, *, #158, .T. ) ;
#72394 = CARTESIAN_POINT ( 'NONE',  ( -43.57658755379780757, -24.65952944569304606, 1.056160979905693909 ) ) ;
#72395 = CARTESIAN_POINT ( 'NONE',  ( 21.10488023177059347, -6.046698511884514460, 11.49999999999998934 ) ) ;
#72396 = CARTESIAN_POINT ( 'NONE',  ( -126.7287160163637054, -25.33540118152307485, 3.690489000554315169 ) ) ;
#72397 = VECTOR ( 'NONE', #37664, 1000.000000000000114 ) ;
#72398 = CARTESIAN_POINT ( 'NONE',  ( -111.5920145005471653, -23.96119346886881019, -0.6495511937832035843 ) ) ;
#72399 = CARTESIAN_POINT ( 'NONE',  ( -118.5895376238167529, -23.48783264082478794, -1.443836473390058384 ) ) ;
#72400 = ORIENTED_EDGE ( 'NONE', *, *, #74081, .T. ) ;
#72401 = CARTESIAN_POINT ( 'NONE',  ( -48.57733566618777132, -24.66019654487199730, 8.947790411086119278 ) ) ;
#72402 = CARTESIAN_POINT ( 'NONE',  ( -0.4453066574538939171, -5.876774720514410077, 19.14913681718892491 ) ) ;
#72403 = VERTEX_POINT ( 'NONE', #70323 ) ;
#72404 = AXIS2_PLACEMENT_3D ( 'NONE', #17371, #141, #71668 ) ;
#72405 = CARTESIAN_POINT ( 'NONE',  ( -68.62287095715005592, -23.47596703998600631, 11.44779298504227505 ) ) ;
#72406 = CARTESIAN_POINT ( 'NONE',  ( 19.38413035786728145, -6.671778716439519030, -1.500000000000002220 ) ) ;
#72407 = ORIENTED_EDGE ( 'NONE', *, *, #73549, .T. ) ;
#72408 = VECTOR ( 'NONE', #47466, 1000.000000000000000 ) ;
#72409 = ORIENTED_EDGE ( 'NONE', *, *, #44028, .F. ) ;
#72410 = VERTEX_POINT ( 'NONE', #93640 ) ;
#72411 = CARTESIAN_POINT ( 'NONE',  ( -67.52287095715006160, -23.47596703998600631, 11.44779298504228748 ) ) ;
#72412 = CARTESIAN_POINT ( 'NONE',  ( 5.194767643164344584, 22.50260600399833422, -1.500000000000002220 ) ) ;
#72413 = CARTESIAN_POINT ( 'NONE',  ( -104.5889232684893670, -24.35071581493543746, 9.817618358456019934 ) ) ;
#72414 = CARTESIAN_POINT ( 'NONE',  ( 16.70477854660759931, 11.60849435585976153, -1.500000000000002220 ) ) ;
#72415 = ORIENTED_EDGE ( 'NONE', *, *, #37962, .T. ) ;
#72416 = CARTESIAN_POINT ( 'NONE',  ( 9.383883476483161346, 17.86611652351680846, 0.000000000000000000 ) ) ;
#72417 = DIRECTION ( 'NONE',  ( -0.000000000000000000, 1.000000000000000000, -0.000000000000000000 ) ) ;
#72418 = AXIS2_PLACEMENT_3D ( 'NONE', #37422, #92189, #66885 ) ;
#72419 = ADVANCED_FACE ( 'NONE', ( #305 ), #78917, .F. ) ;
#72420 = CARTESIAN_POINT ( 'NONE',  ( -93.62287095715005592, -23.72773821059536559, 11.05748984161097681 ) ) ;
#72421 = CARTESIAN_POINT ( 'NONE',  ( 4.647383884978952828, -6.376774720514411854, 19.72975307774251164 ) ) ;
#72422 = VERTEX_POINT ( 'NONE', #85032 ) ;
#72423 = CARTESIAN_POINT ( 'NONE',  ( -28.66129012810275256, -25.21531751186669013, 2.702368919224620747 ) ) ;
#72424 = CARTESIAN_POINT ( 'NONE',  ( -93.52287095715009002, -23.72773821059536914, 11.05748984161097326 ) ) ;
#72425 = ORIENTED_EDGE ( 'NONE', *, *, #32972, .F. ) ;
#72426 = CARTESIAN_POINT ( 'NONE',  ( -11.59579830748209517, 17.24510332420730663, -1.500000000000002220 ) ) ;
#72428 = ADVANCED_FACE ( 'NONE', ( #76910 ), #38863, .T. ) ;
#72427 = EDGE_LOOP ( 'NONE', ( #98759, #14387, #84637, #23099 ) ) ;
#72430 = ORIENTED_EDGE ( 'NONE', *, *, #26862, .T. ) ;
#72429 = CARTESIAN_POINT ( 'NONE',  ( -125.6244081583916881, -24.52300882791529801, 0.6510814631126508045 ) ) ;
#72431 = CARTESIAN_POINT ( 'NONE',  ( -41.52202759913466679, -23.48786465467240347, 11.44779295918255002 ) ) ;
#72432 = DIRECTION ( 'NONE',  ( -0.7071067811865452413, 0.000000000000000000, 0.7071067811865497932 ) ) ;
#72433 = ORIENTED_EDGE ( 'NONE', *, *, #39252, .F. ) ;
#72434 = ORIENTED_EDGE ( 'NONE', *, *, #3167, .T. ) ;
#72435 = FACE_OUTER_BOUND ( 'NONE', #85847, .T. ) ;
#72436 = DIRECTION ( 'NONE',  ( -0.9496245541219264785, 0.000000000000000000, -0.3133898629642195011 ) ) ;
#72437 = FACE_OUTER_BOUND ( 'NONE', #94313, .T. ) ;
#72439 = ORIENTED_EDGE ( 'NONE', *, *, #72807, .F. ) ;
#72438 = CARTESIAN_POINT ( 'NONE',  ( 21.00647827173414939, 6.864759178008983831, 11.49999999999999645 ) ) ;
#72440 = CARTESIAN_POINT ( 'NONE',  ( -101.5562042904833930, -23.47596703998600631, 11.44779298504227683 ) ) ;
#72441 = CARTESIAN_POINT ( 'NONE',  ( -17.80605238980536953, 13.89162706601689479, 11.49999999999998934 ) ) ;
#72443 = EDGE_LOOP ( 'NONE', ( #42795, #18854, #43006, #94761 ) ) ;
#72442 = LINE ( 'NONE', #2937, #21430 ) ;
#72444 = ORIENTED_EDGE ( 'NONE', *, *, #26865, .T. ) ;
#72445 = CARTESIAN_POINT ( 'NONE',  ( -24.90875734969025501, -5.965225279485572685, 30.51402280011862089 ) ) ;
#72446 = ADVANCED_FACE ( 'NONE', ( #62220 ), #61227, .F. ) ;
#72447 = CARTESIAN_POINT ( 'NONE',  ( -57.57869602717082813, -24.66019654487199375, 8.947790411086119278 ) ) ;
#72448 = ORIENTED_EDGE ( 'NONE', *, *, #53371, .F. ) ;
#72449 = CARTESIAN_POINT ( 'NONE',  ( 4.708956132399880978, 20.65895737721473679, 11.49999999999998934 ) ) ;
#72450 = CARTESIAN_POINT ( 'NONE',  ( -44.52287095715006160, -24.64965694238575011, 8.947790433994205372 ) ) ;
#72451 = CARTESIAN_POINT ( 'NONE',  ( -52.62287095715005592, -23.48786465467240703, 11.44779295918255002 ) ) ;
#72452 = CARTESIAN_POINT ( 'NONE',  ( -7.324001883147635894, -5.876774720514413630, 20.17732409774492197 ) ) ;
#72453 = CARTESIAN_POINT ( 'NONE',  ( -80.62287095715008434, -24.92604778743018201, 8.074972756849359001 ) ) ;
#72454 = CARTESIAN_POINT ( 'NONE',  ( 13.39142644571787422, -17.71860720625715757, -1.500000000000002220 ) ) ;
#72455 = CARTESIAN_POINT ( 'NONE',  ( -114.6266393428067545, -24.15543982623908192, -0.2315651400026444429 ) ) ;
#72456 = ORIENTED_EDGE ( 'NONE', *, *, #71347, .F. ) ;
#72457 = DIRECTION ( 'NONE',  ( -0.2488812114211667037, -0.000000000000000000, -0.9685340172660599212 ) ) ;
#72458 = DIRECTION ( 'NONE',  ( -0.000000000000000000, 1.000000000000000000, -0.000000000000000000 ) ) ;
#72459 = CARTESIAN_POINT ( 'NONE',  ( 8.665315094346039970, 17.34094453737590769, 11.49999999999999645 ) ) ;
#72460 = EDGE_CURVE ( 'NONE', #22234, #72609, #16249, .T. ) ;
#72461 = VECTOR ( 'NONE', #54116, 1000.000000000000227 ) ;
#72462 = CARTESIAN_POINT ( 'NONE',  ( -36.58681848114003543, -24.35071581493542325, 9.817618358456030592 ) ) ;
#72463 = DIRECTION ( 'NONE',  ( 0.000000000000000000, -8.856219851039486941E-15, -1.000000000000000000 ) ) ;
#72464 = CARTESIAN_POINT ( 'NONE',  ( -19.44331071757236273, 1.017868325215548708, 11.49999999999998934 ) ) ;
#72465 = CARTESIAN_POINT ( 'NONE',  ( 15.25824911148008844, 15.06768998368162471, -1.500000000000002220 ) ) ;
#72466 = DIRECTION ( 'NONE',  ( 0.000000000000000000, -1.000000000000000000, 0.000000000000000000 ) ) ;
#72467 = CARTESIAN_POINT ( 'NONE',  ( -1.122631020312409245, -6.376774720514413630, 19.41635569784906679 ) ) ;
#72468 = CARTESIAN_POINT ( 'NONE',  ( -51.53190491943575324, -24.65952944569304250, 1.056160979905695463 ) ) ;
#72469 = CARTESIAN_POINT ( 'NONE',  ( -58.22287095715004313, -23.47593901973090169, -1.443836447538997758 ) ) ;
#72470 = CARTESIAN_POINT ( 'NONE',  ( -20.26579564662877075, -10.28286414166031726, -1.500000000000002220 ) ) ;
#72471 = VECTOR ( 'NONE', #86721, 1000.000000000000114 ) ;
#72472 = CARTESIAN_POINT ( 'NONE',  ( -20.27875734969025601, -19.69946567084330624, 24.00402280011861578 ) ) ;
#72473 = VECTOR ( 'NONE', #73798, 1000.000000000000000 ) ;
#72474 = CARTESIAN_POINT ( 'NONE',  ( -102.5474529007568378, -24.65952944569305316, 1.056160979905704123 ) ) ;
#72475 = DIRECTION ( 'NONE',  ( 0.000000000000000000, -0.000000000000000000, -1.000000000000000000 ) ) ;
#72476 = CARTESIAN_POINT ( 'NONE',  ( 13.74685606122050885, 14.44317598224977672, 11.49999999999999645 ) ) ;
#72477 = CARTESIAN_POINT ( 'NONE',  ( -61.62287095715004881, -29.50248528299804818, 1.056150453629034924 ) ) ;
#72478 = AXIS2_PLACEMENT_3D ( 'NONE', #21010, #75296, #82908 ) ;
#72479 = PLANE ( 'NONE',  #76521 ) ;
#72480 = CARTESIAN_POINT ( 'NONE',  ( -48.62369540941691781, -24.65952944569304606, 1.056160979905697239 ) ) ;
#72481 = ADVANCED_FACE ( 'NONE', ( #69317 ), #8417, .T. ) ;
#72482 = ORIENTED_EDGE ( 'NONE', *, *, #68324, .F. ) ;
#72483 = PLANE ( 'NONE',  #34776 ) ;
#72484 = CARTESIAN_POINT ( 'NONE',  ( -77.52287095715006160, -24.65952944569304606, 1.056160979905698794 ) ) ;
#72485 = CARTESIAN_POINT ( 'NONE',  ( -18.79206335510377102, -10.79472360063173397, 11.49999999999998934 ) ) ;
#72486 = CARTESIAN_POINT ( 'NONE',  ( -51.54694215012084157, -25.12787939889654609, 7.132508062825905881 ) ) ;
#72487 = CARTESIAN_POINT ( 'NONE',  ( 19.40022266231057202, 1.907866353064612053, -1.500000000000002220 ) ) ;
#72488 = DIRECTION ( 'NONE',  ( -1.000000000000000000, -3.773278334444166432E-23, -8.201307841325785021E-29 ) ) ;
#72489 = ORIENTED_EDGE ( 'NONE', *, *, #97653, .T. ) ;
#72490 = PERSON_AND_ORGANIZATION ( #70597, #27821 ) ;
#72491 = CYLINDRICAL_SURFACE ( 'NONE', #20784, 2.899999999999999467 ) ;
#72492 = CARTESIAN_POINT ( 'NONE',  ( 11.41020680648336771, 16.95828056793917682, 11.49999999999999645 ) ) ;
#72493 = FACE_OUTER_BOUND ( 'NONE', #42093, .T. ) ;
#72494 = EDGE_CURVE ( 'NONE', #96725, #30324, #78418, .T. ) ;
#72495 = CYLINDRICAL_SURFACE ( 'NONE', #99897, 0.3000000000000016542 ) ;
#72496 = ORIENTED_EDGE ( 'NONE', *, *, #70022, .F. ) ;
#72497 = CARTESIAN_POINT ( 'NONE',  ( -59.62287095715004881, -29.50248528299804818, 1.056150453629034924 ) ) ;
#72498 = CARTESIAN_POINT ( 'NONE',  ( -9.150000000000000355, -6.376774720514426953, -15.69999999999999929 ) ) ;
#72499 = CARTESIAN_POINT ( 'NONE',  ( 7.433267315672343223, -6.376774720514418959, 20.43888261666079842 ) ) ;
#72500 = CARTESIAN_POINT ( 'NONE',  ( -49.27881313098881577, -25.31439476491641472, 6.114505416649892666 ) ) ;
#72501 = ADVANCED_FACE ( 'NONE', ( #93140 ), #71328, .T. ) ;
#72502 = CARTESIAN_POINT ( 'NONE',  ( 3.737436867076077363, 13.63388347648318444, 0.000000000000000000 ) ) ;
#72503 = VERTEX_POINT ( 'NONE', #39368 ) ;
#72504 = CARTESIAN_POINT ( 'NONE',  ( -66.60923601032587271, -23.48786465467241058, 11.44779295918254824 ) ) ;
#72505 = AXIS2_PLACEMENT_3D ( 'NONE', #50331, #26494, #42729 ) ;
#72506 = EDGE_CURVE ( 'NONE', #14881, #26599, #76675, .T. ) ;
#72507 = CARTESIAN_POINT ( 'NONE',  ( -21.12268324108725892, 9.058254180033936009, 11.49999999999999645 ) ) ;
#72508 = CARTESIAN_POINT ( 'NONE',  ( -9.471985145535571249, 20.67137392225973258, -1.500000000000002220 ) ) ;
#72509 = CARTESIAN_POINT ( 'NONE',  ( -110.5878943189815118, -24.73531770709095312, 8.716586749053508498 ) ) ;
#72510 = B_SPLINE_SURFACE_WITH_KNOTS ( 'NONE', 3, 3, ( 
 ( #61137, #69231, #62631, #92064 ),
 ( #78326, #54020, #39769, #70734 ),
 ( #78822, #1228, #63134, #94060 ),
 ( #37784, #68738, #99656, #22533 ),
 ( #84948, #53526, #38274, #15432 ),
 ( #84449, #100147, #14931, #30668 ),
 ( #61637, #92557, #46394, #57024 ) ),
 .UNSPECIFIED., .F., .F., .F.,
 ( 4, 3, 4 ),
 ( 4, 4 ),
 ( 0.0004766839783816073282, 0.1029713700210892480, 0.2054660560637968925 ),
 ( 0.7396821597525450320, 0.7410361722979724730 ),
 .UNSPECIFIED. ) ;
#72511 = DIRECTION ( 'NONE',  ( -0.000000000000000000, 0.000000000000000000, -1.000000000000000000 ) ) ;
#72512 = CARTESIAN_POINT ( 'NONE',  ( 9.950000000000006395, 0.000000000000000000, 18.35000000000000142 ) ) ;
#72513 = AXIS2_PLACEMENT_3D ( 'NONE', #29142, #75309, #29642 ) ;
#72514 = CARTESIAN_POINT ( 'NONE',  ( -70.52287095715006160, -24.92579138211020151, 1.929029949965661794 ) ) ;
#72515 = LINE ( 'NONE', #19202, #41691 ) ;
#72516 = CARTESIAN_POINT ( 'NONE',  ( -11.13288495942205536, 18.84158392345546318, -1.500000000000002220 ) ) ;
#72517 = DIRECTION ( 'NONE',  ( 0.000000000000000000, 0.000000000000000000, 1.000000000000000000 ) ) ;
#72518 = LINE ( 'NONE', #65425, #21674 ) ;
#72519 = LINE ( 'NONE', #73020, #35534 ) ;
#72520 = CARTESIAN_POINT ( 'NONE',  ( -99.16166289166534398, -25.31200570402560146, 5.311370725124462844 ) ) ;
#72521 = ORIENTED_EDGE ( 'NONE', *, *, #26545, .F. ) ;
#72522 = CARTESIAN_POINT ( 'NONE',  ( -19.81292649638395531, 4.959676026661640869, 11.49999999999998934 ) ) ;
#72523 = VERTEX_POINT ( 'NONE', #1815 ) ;
#72524 = ORIENTED_EDGE ( 'NONE', *, *, #18085, .T. ) ;
#72525 = CARTESIAN_POINT ( 'NONE',  ( 21.12055942831636202, -9.126644407798330860, 11.49999999999998934 ) ) ;
#72526 = CARTESIAN_POINT ( 'NONE',  ( -80.52287095715007581, -23.48783264082477018, -1.443836473390091246 ) ) ;
#72527 = ORIENTED_EDGE ( 'NONE', *, *, #17341, .T. ) ;
#72528 = DIRECTION ( 'NONE',  ( -3.773278334444166432E-23, 1.000000000000000000, 0.000000000000000000 ) ) ;
#72529 = CIRCLE ( 'NONE', #28770, 28.45799999999999486 ) ;
#72530 = DIRECTION ( 'NONE',  ( 1.000000000000000000, 3.773278334444167608E-23, 8.201307833595939069E-29 ) ) ;
#72531 = FACE_OUTER_BOUND ( 'NONE', #23315, .T. ) ;
#72533 = ORIENTED_EDGE ( 'NONE', *, *, #28553, .F. ) ;
#72532 = CARTESIAN_POINT ( 'NONE',  ( -18.60337119584764665, 10.53494341765418874, 11.49999999999999645 ) ) ;
#72534 = ORIENTED_EDGE ( 'NONE', *, *, #67091, .F. ) ;
#72535 = CARTESIAN_POINT ( 'NONE',  ( -18.24902840909259538, -12.68162010772806170, 11.49999999999998934 ) ) ;
#72536 = CARTESIAN_POINT ( 'NONE',  ( 13.32396043830641830, 15.83023408377254704, -1.500000000000002220 ) ) ;
#72537 = AXIS2_PLACEMENT_3D ( 'NONE', #15975, #15479, #92602 ) ;
#72538 = ORIENTED_EDGE ( 'NONE', *, *, #65892, .F. ) ;
#72539 = EDGE_CURVE ( 'NONE', #58613, #22171, #85534, .T. ) ;
#72540 = PLANE ( 'NONE',  #38195 ) ;
#72541 = CARTESIAN_POINT ( 'NONE',  ( 2.993365552154886089, -5.876774720514413630, 19.24059921568563425 ) ) ;
#72542 = ORIENTED_EDGE ( 'NONE', *, *, #33507, .F. ) ;
#72543 = CARTESIAN_POINT ( 'NONE',  ( -95.52287095715003318, -24.82558206586148941, 1.605769216559624457 ) ) ;
#72544 = AXIS2_PLACEMENT_3D ( 'NONE', #79795, #26524, #81303 ) ;
#72545 = EDGE_LOOP ( 'NONE', ( #65924, #14859, #69777, #14638 ) ) ;
#72546 = CARTESIAN_POINT ( 'NONE',  ( 14.61581676225068449, -3.316774720514424679, -27.35847991880143226 ) ) ;
#72547 = CARTESIAN_POINT ( 'NONE',  ( -5.376107494350208960, -20.15860285114975525, -1.500000000000002220 ) ) ;
#72548 = CARTESIAN_POINT ( 'NONE',  ( 9.607415760296678542, -19.69187540195887465, 11.49999999999999645 ) ) ;
#72549 = CARTESIAN_POINT ( 'NONE',  ( 3.675000000000004707, 1.999999999999998224, 24.00000000000000000 ) ) ;
#72550 = DIRECTION ( 'NONE',  ( 0.5543250044962501066, 0.000000000000000000, -0.8323003000060928969 ) ) ;
#72551 = CARTESIAN_POINT ( 'NONE',  ( 21.68943130245101258, -6.005725296444199834, -1.500000000000002220 ) ) ;
#72552 = CARTESIAN_POINT ( 'NONE',  ( 13.87900837158347755, -15.70065903812341013, -1.500000000000002220 ) ) ;
#72553 = CARTESIAN_POINT ( 'NONE',  ( -89.40841769935767047, -25.29749010697736367, 3.864033824493484204 ) ) ;
#72554 = DIRECTION ( 'NONE',  ( 0.7512896232465891000, 0.000000000000000000, 0.6599726524652352877 ) ) ;
#72555 = LINE ( 'NONE', #41612, #6999 ) ;
#72556 = ORIENTED_EDGE ( 'NONE', *, *, #6112, .F. ) ;
#72557 = ORIENTED_EDGE ( 'NONE', *, *, #83318, .T. ) ;
#72558 = ORIENTED_EDGE ( 'NONE', *, *, #36265, .T. ) ;
#72559 = CARTESIAN_POINT ( 'NONE',  ( -52.58237442762383296, -24.51314013834315375, 0.6176544820404124003 ) ) ;
#72560 = EDGE_LOOP ( 'NONE', ( #25082, #74116, #43461, #97250, #37761, #11287, #49895, #74331, #87889, #10410, #74541, #71680, #11504, #5248, #90116, #37454, #99693, #84650, #76367, #36588, #91613, #53458, #13094, #27832 ) ) ;
#72561 = EDGE_CURVE ( 'NONE', #34684, #31278, #81680, .T. ) ;
#72562 = CARTESIAN_POINT ( 'NONE',  ( -16.73372362409233105, 13.38858591273363174, -1.500000000000002220 ) ) ;
#72563 = ORIENTED_EDGE ( 'NONE', *, *, #76208, .F. ) ;
#72564 = PLANE ( 'NONE',  #47266 ) ;
#72565 = EDGE_CURVE ( 'NONE', #40450, #3797, #46986, .T. ) ;
#72566 = CARTESIAN_POINT ( 'NONE',  ( 10.44912437418449969, 18.32051524777507723, -1.500000000000002220 ) ) ;
#72567 = CARTESIAN_POINT ( 'NONE',  ( -102.5228709571500900, -23.47593901973090524, -1.443836447538996648 ) ) ;
#72568 = CARTESIAN_POINT ( 'NONE',  ( -92.52287095715006160, -24.65952944569304606, 1.056160979905700570 ) ) ;
#72569 = CARTESIAN_POINT ( 'NONE',  ( -52.62287095715005592, -23.48783264082478794, -1.443836473390070596 ) ) ;
#72570 = CARTESIAN_POINT ( 'NONE',  ( -101.5124433422946737, -24.34968618360934300, 0.1864209137778871928 ) ) ;
#72571 = CARTESIAN_POINT ( 'NONE',  ( -107.5228709571500758, -24.65952944569304961, 1.056160979905704123 ) ) ;
#72572 = CARTESIAN_POINT ( 'NONE',  ( 11.67614657018352453, 18.69773523334854914, -1.500000000000002220 ) ) ;
#72573 = ORIENTED_EDGE ( 'NONE', *, *, #87761, .F. ) ;
#72574 = CARTESIAN_POINT ( 'NONE',  ( -116.5581106647310889, -23.48783264082478439, -1.443836473390061936 ) ) ;
#72575 = DIRECTION ( 'NONE',  ( 0.000000000000000000, 0.000000000000000000, 1.000000000000000000 ) ) ;
#72576 = CARTESIAN_POINT ( 'NONE',  ( -60.48528285801528170, -24.83618233451449697, 1.606449574219535936 ) ) ;
#72577 = AXIS2_PLACEMENT_3D ( 'NONE', #79035, #63850, #49616 ) ;
#72578 = EDGE_CURVE ( 'NONE', #38855, #7487, #15518, .T. ) ;
#72579 = EDGE_CURVE ( 'NONE', #59433, #50558, #30687, .T. ) ;
#72580 = CARTESIAN_POINT ( 'NONE',  ( -29.84334126970346190, -25.10778653237075275, 7.214475432169975555 ) ) ;
#72581 = B_SPLINE_CURVE_WITH_KNOTS ( 'NONE', 3,
 ( #5209, #67132, #64272, #74226 ),
 .UNSPECIFIED., .F., .F.,
 ( 4, 4 ),
 ( 0.000000000000000000, 1.000000000000000000 ),
 .UNSPECIFIED. ) ;
#72582 = CARTESIAN_POINT ( 'NONE',  ( -27.24386298623018021, -24.58417960884006348, 1.680793441616425410 ) ) ;
#72583 = EDGE_CURVE ( 'NONE', #16640, #77030, #3333, .T. ) ;
#72584 = CARTESIAN_POINT ( 'NONE',  ( -56.58953762381672448, -23.48783264082478084, -1.443836473390068820 ) ) ;
#72585 = CARTESIAN_POINT ( 'NONE',  ( -3.453506354162970915, -21.03206338698385736, 11.49999999999998934 ) ) ;
#72586 = DIRECTION ( 'NONE',  ( -3.773278334453079030E-23, 0.9999999999976377785, 2.173523156925978705E-06 ) ) ;
#72587 = CARTESIAN_POINT ( 'NONE',  ( -66.62287095715004170, -23.72747288104469376, -1.053458166803226348 ) ) ;
#72588 = CARTESIAN_POINT ( 'NONE',  ( -64.57975408571323328, -24.66019654487199730, 8.947790411086115725 ) ) ;
#72589 = CARTESIAN_POINT ( 'NONE',  ( -67.55620429048336462, -24.66019654487199020, 8.947790411086131712 ) ) ;
#72590 = CARTESIAN_POINT ( 'NONE',  ( 19.13181028273733375, 12.02906595412573232, -1.500000000000002220 ) ) ;
#72591 = B_SPLINE_SURFACE_WITH_KNOTS ( 'NONE', 3, 3, ( 
 ( #40958, #35350, #71919, #26230 ),
 ( #95241, #33331, #34846, #42966 ),
 ( #64323, #73902, #57204, #65815 ),
 ( #89132, #88138, #49581, #80514 ),
 ( #11006, #72915, #97240, #57692 ),
 ( #3413, #34348, #4401, #19107 ),
 ( #65326, #81019, #11497, #96737 ) ),
 .UNSPECIFIED., .F., .F., .F.,
 ( 4, 3, 4 ),
 ( 4, 4 ),
 ( 0.7945040073713779405, 0.8970133732236067470, 0.9995227390758355535 ),
 ( 0.03212669907356750093, 0.03698063968062436507 ),
 .UNSPECIFIED. ) ;
#72592 = CARTESIAN_POINT ( 'NONE',  ( -112.5228709571500616, -23.47593901973090524, -1.443836447538996426 ) ) ;
#72593 = ORIENTED_EDGE ( 'NONE', *, *, #51852, .F. ) ;
#72594 = CARTESIAN_POINT ( 'NONE',  ( -35.62287095715005592, -24.63345952396256777, 9.038047939301515399 ) ) ;
#72595 = CARTESIAN_POINT ( 'NONE',  ( -120.5895376238167103, -23.47596703998600631, 11.44779298504227683 ) ) ;
#72596 = CARTESIAN_POINT ( 'NONE',  ( 19.74453702311487646, -0.1846442961375113490, 11.49999999999999645 ) ) ;
#72597 = CARTESIAN_POINT ( 'NONE',  ( -32.07722060962684196, -25.34389491264532879, 4.638595615756661239 ) ) ;
#72598 = CARTESIAN_POINT ( 'NONE',  ( 2.499999999999995115, 19.99999999999999645, 2.100000000000000089 ) ) ;
#72599 = EDGE_CURVE ( 'NONE', #3035, #80243, #76259, .T. ) ;
#72600 = ORIENTED_EDGE ( 'NONE', *, *, #4458, .F. ) ;
#72601 = CARTESIAN_POINT ( 'NONE',  ( -42.52287095715005449, -23.47593901973090169, -1.443836447538997092 ) ) ;
#72602 = CARTESIAN_POINT ( 'NONE',  ( -124.4728709571500360, -25.40675522342680637, 5.000950440042752021 ) ) ;
#72603 = CARTESIAN_POINT ( 'NONE',  ( -124.5895423235921271, -24.35071581493544457, 9.817618358456016381 ) ) ;
#72604 = DIRECTION ( 'NONE',  ( 0.000000000000000000, 0.000000000000000000, -1.000000000000000000 ) ) ;
#72605 = CARTESIAN_POINT ( 'NONE',  ( 13.10664265030973930, -5.965225279485574461, -27.62597719988137612 ) ) ;
#72606 = CARTESIAN_POINT ( 'NONE',  ( 8.071512145086499501, -1.028487854913504362, 6.500000000000000000 ) ) ;
#72607 = CARTESIAN_POINT ( 'NONE',  ( 11.16000000000000014, -10.65233964170348635, -1.621096496867198589 ) ) ;
#72608 = CARTESIAN_POINT ( 'NONE',  ( -15.39140670439391378, -12.39996395878027791, 11.49999999999998934 ) ) ;
#72609 = VERTEX_POINT ( 'NONE', #65733 ) ;
#72610 = CARTESIAN_POINT ( 'NONE',  ( -9.470923242388245455, -17.85692771776473364, 11.49999999999999645 ) ) ;
#72611 = CARTESIAN_POINT ( 'NONE',  ( -112.6228709571500559, -23.73934037231757799, 11.05740245334328975 ) ) ;
#72612 = EDGE_CURVE ( 'NONE', #40589, #98594, #63535, .T. ) ;
#72613 = CIRCLE ( 'NONE', #28854, 19.00000000000000000 ) ;
#72614 = EDGE_CURVE ( 'NONE', #51996, #94218, #8953, .T. ) ;
#72615 = ORIENTED_EDGE ( 'NONE', *, *, #24387, .F. ) ;
#72616 = CARTESIAN_POINT ( 'NONE',  ( 26.73860345374794178, 5.356774720514427379, -3.781275721883787355 ) ) ;
#72617 = DIRECTION ( 'NONE',  ( 0.000000000000000000, 0.000000000000000000, 1.000000000000000000 ) ) ;
#72618 = CARTESIAN_POINT ( 'NONE',  ( -59.55620429048338593, -23.48786465467241058, 11.44779295918255180 ) ) ;
#72619 = CARTESIAN_POINT ( 'NONE',  ( -31.55620429048338593, -23.48786465467240347, 11.44779295918255002 ) ) ;
#72620 = VECTOR ( 'NONE', #1278, 1000.000000000000114 ) ;
#72621 = LINE ( 'NONE', #42183, #86180 ) ;
#72622 = CARTESIAN_POINT ( 'NONE',  ( -58.55620429048339304, -24.64898659630528144, 1.056161002820823036 ) ) ;
#72623 = CARTESIAN_POINT ( 'NONE',  ( 15.84714387567644955, -12.28532832577633194, 11.49999999999998934 ) ) ;
#72624 = ADVANCED_FACE ( 'NONE', ( #59109 ), #36261, .F. ) ;
#72625 = DIRECTION ( 'NONE',  ( 1.000000000000000000, 3.773278334444166432E-23, 8.201307841325785021E-29 ) ) ;
#72626 = ORIENTED_EDGE ( 'NONE', *, *, #88042, .T. ) ;
#72627 = EDGE_CURVE ( 'NONE', #84363, #9929, #44881, .T. ) ;
#72628 = EDGE_CURVE ( 'NONE', #62142, #23337, #91035, .T. ) ;
#72629 = VECTOR ( 'NONE', #74343, 1000.000000000000000 ) ;
#72630 = DIRECTION ( 'NONE',  ( -0.000000000000000000, -1.000000000000000000, -0.000000000000000000 ) ) ;
#72631 = B_SPLINE_CURVE_WITH_KNOTS ( 'NONE', 3,
 ( #61652, #92078, #92570, #15449 ),
 .UNSPECIFIED., .F., .F.,
 ( 4, 4 ),
 ( 0.000000000000000000, 9.999999999999592548E-05 ),
 .UNSPECIFIED. ) ;
#72632 = CARTESIAN_POINT ( 'NONE',  ( -96.62287095715005592, -24.64898659630368272, 1.056161002820829697 ) ) ;
#72633 = CARTESIAN_POINT ( 'NONE',  ( -79.44752152392706535, -25.29575941214698531, 5.495406740378385280 ) ) ;
#72634 = LINE ( 'NONE', #3126, #98370 ) ;
#72635 = CARTESIAN_POINT ( 'NONE',  ( -73.53861189177032998, -24.65952944569304606, 1.056160979905700126 ) ) ;
#72636 = CARTESIAN_POINT ( 'NONE',  ( 6.044871794871792048, -5.876774720514402084, 18.16025641025640880 ) ) ;
#72637 = EDGE_CURVE ( 'NONE', #45965, #45491, #71987, .T. ) ;
#72638 = CARTESIAN_POINT ( 'NONE',  ( -49.51010171462829135, -25.25846184752573720, 3.931802542169027248 ) ) ;
#72639 = VERTEX_POINT ( 'NONE', #67225 ) ;
#72640 = CARTESIAN_POINT ( 'NONE',  ( -18.18203184671642703, 9.085611141607108365, 11.49999999999998934 ) ) ;
#72641 = VERTEX_POINT ( 'NONE', #29636 ) ;
#72642 = FACE_OUTER_BOUND ( 'NONE', #62457, .T. ) ;
#72643 = CARTESIAN_POINT ( 'NONE',  ( -127.5222628862546514, -23.48786465467242124, 11.44779295918253226 ) ) ;
#72644 = EDGE_LOOP ( 'NONE', ( #7046, #86584 ) ) ;
#72645 = CARTESIAN_POINT ( 'NONE',  ( -105.6228709571501128, -24.15431212366391378, -0.2830839119428946726 ) ) ;
#72646 = CARTESIAN_POINT ( 'NONE',  ( -49.29494865489761679, -25.12215252155673895, 6.331091545398378706 ) ) ;
#72647 = DIRECTION ( 'NONE',  ( -1.000000000000000000, 0.000000000000000000, -0.000000000000000000 ) ) ;
#72648 = CARTESIAN_POINT ( 'NONE',  ( -9.361133326760958440, -19.03884994183470880, 11.49999999999999645 ) ) ;
#72649 = CARTESIAN_POINT ( 'NONE',  ( -10.67647856527443473, 19.39090429279614369, 11.49999999999998934 ) ) ;
#72650 = CARTESIAN_POINT ( 'NONE',  ( 14.24201292913401140, 14.87178044790754328, 11.49999999999998934 ) ) ;
#72651 = ORIENTED_EDGE ( 'NONE', *, *, #31004, .F. ) ;
#72652 = CARTESIAN_POINT ( 'NONE',  ( -41.53391078925199764, -24.51314013834315375, 0.6176544820404115121 ) ) ;
#72653 = EDGE_LOOP ( 'NONE', ( #60182, #33145, #60096, #38072 ) ) ;
#72654 = CARTESIAN_POINT ( 'NONE',  ( 7.164812103570541879, -6.376774720514422512, 20.85668272347560404 ) ) ;
#72655 = LINE ( 'NONE', #3645, #19417 ) ;
#72656 = ORIENTED_EDGE ( 'NONE', *, *, #55821, .F. ) ;
#72657 = ORIENTED_EDGE ( 'NONE', *, *, #87049, .F. ) ;
#72658 = ORIENTED_EDGE ( 'NONE', *, *, #41023, .T. ) ;
#72659 = CARTESIAN_POINT ( 'NONE',  ( -116.6228709571500275, -24.33927499327854704, 9.819080762295804732 ) ) ;
#72660 = CARTESIAN_POINT ( 'NONE',  ( 6.586338672804227024, -5.876774720514415407, 20.10086663068103618 ) ) ;
#72661 = CARTESIAN_POINT ( 'NONE',  ( 5.326923076923078426, -5.876774720514419847, 20.76772836538461320 ) ) ;
#72662 = CARTESIAN_POINT ( 'NONE',  ( 19.89799572200132971, -5.707369160466581270, -1.500000000000002220 ) ) ;
#72663 = CARTESIAN_POINT ( 'NONE',  ( 7.043455336710909620, -20.48365140995157674, 11.49999999999999645 ) ) ;
#72664 = VERTEX_POINT ( 'NONE', #98138 ) ;
#72665 = DIRECTION ( 'NONE',  ( 0.000000000000000000, 0.000000000000000000, 1.000000000000000000 ) ) ;
#72666 = CARTESIAN_POINT ( 'NONE',  ( -110.7976466536441080, -25.12311862853486133, 2.903749597397971449 ) ) ;
#72667 = CARTESIAN_POINT ( 'NONE',  ( -9.774569144048079750, -20.17623354167628946, 11.49999999999998934 ) ) ;
#72668 = VECTOR ( 'NONE', #70359, 1000.000000000000000 ) ;
#72669 = CARTESIAN_POINT ( 'NONE',  ( 19.75748517575715368, -5.965225279485572685, 28.87153971905864580 ) ) ;
#72670 = CARTESIAN_POINT ( 'NONE',  ( -65.52204162676289911, -23.48783264082477018, -1.443836473390096353 ) ) ;
#72671 = ORIENTED_EDGE ( 'NONE', *, *, #70732, .T. ) ;
#72672 = CARTESIAN_POINT ( 'NONE',  ( 29.59852343658945983, 4.673870278164355518, 28.90818992718861224 ) ) ;
#72673 = CARTESIAN_POINT ( 'NONE',  ( 12.46431485231495806, -4.283161447665844612, -27.85634418129429690 ) ) ;
#72674 = ORIENTED_EDGE ( 'NONE', *, *, #20047, .F. ) ;
#72675 = EDGE_LOOP ( 'NONE', ( #81036, #3174, #85008, #70005 ) ) ;
#72676 = LINE ( 'NONE', #35114, #45789 ) ;
#72677 = ORIENTED_EDGE ( 'NONE', *, *, #29248, .F. ) ;
#72678 = DIRECTION ( 'NONE',  ( 0.000000000000000000, 0.9999999999976377785, 2.173523156925979975E-06 ) ) ;
#72679 = EDGE_CURVE ( 'NONE', #27602, #49448, #28645, .T. ) ;
#72680 = CARTESIAN_POINT ( 'NONE',  ( 13.55612473118199723, -16.30799122071102403, -1.500000000000002220 ) ) ;
#72681 = EDGE_LOOP ( 'NONE', ( #10771, #18908, #61410, #79080 ) ) ;
#72682 = CARTESIAN_POINT ( 'NONE',  ( -68.62287095715008434, -24.51283580621364067, 0.6167428607019829201 ) ) ;
#72683 = EDGE_CURVE ( 'NONE', #19708, #78060, #51488, .T. ) ;
#72684 = CARTESIAN_POINT ( 'NONE',  ( -9.754611696910345131, 19.53525426502628548, -1.500000000000002220 ) ) ;
#72685 = CARTESIAN_POINT ( 'NONE',  ( -103.5172066925842103, -23.96169478059713498, 10.65365249895717881 ) ) ;
#72686 = AXIS2_PLACEMENT_3D ( 'NONE', #44665, #99431, #98935 ) ;
#72687 = CARTESIAN_POINT ( 'NONE',  ( 7.072045900997899537, -6.376774720514427841, 21.62824307385093192 ) ) ;
#72688 = CARTESIAN_POINT ( 'NONE',  ( -35.62287095715002749, -24.51163499207174468, 0.6490370598554239256 ) ) ;
#72689 = CARTESIAN_POINT ( 'NONE',  ( -11.18773875818744656, -18.78983145652188469, -1.500000000000002220 ) ) ;
#72690 = CARTESIAN_POINT ( 'NONE',  ( 7.166040305186291093, -6.376774720514420736, 20.81030863372915718 ) ) ;
#72691 = ORIENTED_EDGE ( 'NONE', *, *, #62184, .T. ) ;
#72692 = CARTESIAN_POINT ( 'NONE',  ( 29.58519688192010832, -4.109013365083094449, 29.12059310601990703 ) ) ;
#72693 = FACE_OUTER_BOUND ( 'NONE', #13009, .T. ) ;
#72694 = EDGE_CURVE ( 'NONE', #49218, #56694, #67723, .T. ) ;
#72695 = EDGE_CURVE ( 'NONE', #91850, #63208, #22796, .T. ) ;
#72696 = ORIENTED_EDGE ( 'NONE', *, *, #34577, .T. ) ;
#72697 = EDGE_CURVE ( 'NONE', #79616, #58859, #32531, .T. ) ;
#72698 = PLANE ( 'NONE',  #25391 ) ;
#72699 = VECTOR ( 'NONE', #84703, 1000.000000000000114 ) ;
#72700 = ORIENTED_EDGE ( 'NONE', *, *, #78461, .F. ) ;
#72701 = DIRECTION ( 'NONE',  ( -0.000000000000000000, 2.173523156925979552E-06, -0.9999999999976378895 ) ) ;
#72702 = EDGE_CURVE ( 'NONE', #14136, #72949, #48982, .T. ) ;
#72703 = CARTESIAN_POINT ( 'NONE',  ( -79.11611000704996854, -25.21083105912962097, 3.409327675794633361 ) ) ;
#72704 = CARTESIAN_POINT ( 'NONE',  ( 6.411417644607832145, 20.24884965431308714, 11.49999999999998934 ) ) ;
#72705 = CARTESIAN_POINT ( 'NONE',  ( 22.81105451610979173, 2.682774720514426559, -18.46691820600746681 ) ) ;
#72706 = CARTESIAN_POINT ( 'NONE',  ( -130.5728709571500588, -23.56000036390796737, 11.50200000000000244 ) ) ;
#72707 = CARTESIAN_POINT ( 'NONE',  ( -4.568292318365942073, -0.3587747205144265483, 30.06720597538392425 ) ) ;
#72708 = CARTESIAN_POINT ( 'NONE',  ( -68.49733487582329872, -24.51314013834315375, 0.6176544820404119562 ) ) ;
#72709 = CARTESIAN_POINT ( 'NONE',  ( -19.08929872761019908, -3.557156390981079053, 11.49999999999998934 ) ) ;
#72710 = CARTESIAN_POINT ( 'NONE',  ( -45.52798609474427138, -24.83618233451449697, 1.606449574219536158 ) ) ;
#72711 = EDGE_LOOP ( 'NONE', ( #37449, #8801, #12299, #8490 ) ) ;
#72712 = CARTESIAN_POINT ( 'NONE',  ( 10.47639735327893362, 16.54961352017854637, 11.49999999999999645 ) ) ;
#72713 = CARTESIAN_POINT ( 'NONE',  ( -5.563047341353722253, -5.876774720514411854, 20.06599527532950589 ) ) ;
#72714 = CARTESIAN_POINT ( 'NONE',  ( 24.71017632900191074, 5.356774720514427379, 1.647607965253217399 ) ) ;
#72715 = ADVANCED_FACE ( 'NONE', ( #27654 ), #43873, .F. ) ;
#72716 = ORIENTED_EDGE ( 'NONE', *, *, #85996, .F. ) ;
#72717 = FACE_BOUND ( 'NONE', #9127, .T. ) ;
#72718 = CARTESIAN_POINT ( 'NONE',  ( -75.62287095715004170, -24.63287334234180292, 0.9662140553045361901 ) ) ;
#72719 = LINE ( 'NONE', #3219, #92541 ) ;
#72720 = CARTESIAN_POINT ( 'NONE',  ( 14.61581670307174008, -2.682774720514426559, -27.35847990810646024 ) ) ;
#72722 = ADVANCED_FACE ( 'NONE', ( #21509 ), #68208, .F. ) ;
#72721 = CARTESIAN_POINT ( 'NONE',  ( 19.69511366699831001, -0.05742560045514189665, -1.500000000000002220 ) ) ;
#72723 = ORIENTED_EDGE ( 'NONE', *, *, #89409, .T. ) ;
#72724 = LINE ( 'NONE', #41269, #95905 ) ;
#72725 = CARTESIAN_POINT ( 'NONE',  ( -0.07435467474217070938, 23.09247799282200475, -1.500000000000002220 ) ) ;
#72726 = EDGE_CURVE ( 'NONE', #56862, #4409, #2978, .T. ) ;
#72727 = PERSON_AND_ORGANIZATION ( #70597, #27821 ) ;
#72728 = ORIENTED_EDGE ( 'NONE', *, *, #3422, .T. ) ;
#72729 = CARTESIAN_POINT ( 'NONE',  ( 3.063121397228215859, -6.376774720514420736, 20.95210102656095685 ) ) ;
#72730 = CARTESIAN_POINT ( 'NONE',  ( -1.743696941008423984, -6.376774720514413630, 19.59984006504825160 ) ) ;
#72731 = LINE ( 'NONE', #31280, #26450 ) ;
#72732 = PLANE ( 'NONE',  #78457 ) ;
#72733 = CARTESIAN_POINT ( 'NONE',  ( 8.160000000000000142, -9.652339641703484574, -1.621096496867199033 ) ) ;
#72734 = VECTOR ( 'NONE', #45176, 1000.000000000000000 ) ;
#72735 = AXIS2_PLACEMENT_3D ( 'NONE', #51228, #51730, #44117 ) ;
#72736 = CARTESIAN_POINT ( 'NONE',  ( -69.45824367449309023, -25.24515144706554182, 5.785093357820605853 ) ) ;
#72737 = B_SPLINE_CURVE_WITH_KNOTS ( 'NONE', 3,
 ( #6513, #68413, #92730, #62821, #23217, #38456 ),
 .UNSPECIFIED., .F., .F.,
 ( 4, 2, 4 ),
 ( 0.000000000000000000, 0.001380764517854760412, 0.002761529035709520824 ),
 .UNSPECIFIED. ) ;
#72738 = CARTESIAN_POINT ( 'NONE',  ( -1.714505518806294145E-16, -7.835183881457442823, 1.399999999999999911 ) ) ;
#72739 = CARTESIAN_POINT ( 'NONE',  ( 19.82558669001425500, -2.195561414069463702, -1.500000000000002220 ) ) ;
#72740 = CARTESIAN_POINT ( 'NONE',  ( -75.49535866980721721, -24.73531770709095312, 8.716586749053512051 ) ) ;
#72741 = CARTESIAN_POINT ( 'NONE',  ( 18.24224480919323810, -7.949361806615760528, -1.500000000000002220 ) ) ;
#72742 = ORIENTED_EDGE ( 'NONE', *, *, #90712, .T. ) ;
#72743 = AXIS2_PLACEMENT_3D ( 'NONE', #8004, #61809, #93734 ) ;
#72744 = CARTESIAN_POINT ( 'NONE',  ( -111.5228709571500616, -29.50247984919015209, -1.443849546365048253 ) ) ;
#72745 = ADVANCED_FACE ( 'NONE', ( #44378 ), #23000, .F. ) ;
#72746 = CARTESIAN_POINT ( 'NONE',  ( 32.16024265030974050, 5.965225279485572685, 14.03360796525321774 ) ) ;
#72747 = CARTESIAN_POINT ( 'NONE',  ( -72.58953762381672448, -24.64898659630367916, 1.056161002820384942 ) ) ;
#72748 = CARTESIAN_POINT ( 'NONE',  ( 9.818046095193736278, -3.316774720514088504, -28.04791984001701621 ) ) ;
#72749 = CARTESIAN_POINT ( 'NONE',  ( -18.04518632387085830, 10.29925911722504317, 11.49999999999999645 ) ) ;
#72750 = CARTESIAN_POINT ( 'NONE',  ( -7.567681410454951241, -6.376774720514411854, 19.71630089903357330 ) ) ;
#72751 = VECTOR ( 'NONE', #69242, 1000.000000000000227 ) ;
#72752 = EDGE_CURVE ( 'NONE', #42444, #56728, #58476, .T. ) ;
#72753 = DIRECTION ( 'NONE',  ( -8.334928612639484546E-17, 1.000000000000000000, -7.321843366904296032E-17 ) ) ;
#72754 = CARTESIAN_POINT ( 'NONE',  ( 22.56601425305882813, -3.627385684441148506, 11.49999999999999645 ) ) ;
#72755 = ORIENTED_EDGE ( 'NONE', *, *, #925, .T. ) ;
#72756 = CARTESIAN_POINT ( 'NONE',  ( -108.6228709571500559, -24.64965695001468404, 8.947790433994176951 ) ) ;
#72757 = DIRECTION ( 'NONE',  ( 3.773278334444167020E-23, -1.000000000000000000, 0.000000000000000000 ) ) ;
#72758 = ORIENTED_EDGE ( 'NONE', *, *, #92864, .T. ) ;
#72759 = VECTOR ( 'NONE', #8093, 1000.000000000000114 ) ;
#72760 = CARTESIAN_POINT ( 'NONE',  ( 20.02926185082240451, -2.967945350358753398, -1.500000000000002220 ) ) ;
#72761 = EDGE_CURVE ( 'NONE', #82528, #76018, #186, .T. ) ;
#72762 = CARTESIAN_POINT ( 'NONE',  ( 7.448826589983275959, -5.876774720514420736, 21.05250386848070221 ) ) ;
#72763 = CARTESIAN_POINT ( 'NONE',  ( 7.462166178408539352, 5.965225279485572685, -27.67315496249664974 ) ) ;
#72764 = DIRECTION ( 'NONE',  ( -0.9822594791677485837, 0.000000000000000000, 0.1875268396392987258 ) ) ;
#72765 = ORIENTED_EDGE ( 'NONE', *, *, #59686, .F. ) ;
#72766 = CARTESIAN_POINT ( 'NONE',  ( -80.35919894935766195, -25.30543142107805465, 4.505481316334992492 ) ) ;
#72767 = CARTESIAN_POINT ( 'NONE',  ( -10.12061615367207601, 3.718318319926830373, 30.49412484105965859 ) ) ;
#72768 = CARTESIAN_POINT ( 'NONE',  ( 12.72590371223024697, 15.41468647733915809, -1.500000000000002220 ) ) ;
#72769 = B_SPLINE_CURVE_WITH_KNOTS ( 'NONE', 3,
 ( #19395, #40742, #10292, #3692 ),
 .UNSPECIFIED., .F., .F.,
 ( 4, 4 ),
 ( 0.000000000000000000, 0.0001000000000000444977 ),
 .UNSPECIFIED. ) ;
#72770 = CARTESIAN_POINT ( 'NONE',  ( 17.97375762979478253, -10.76934015532128797, 11.49999999999999645 ) ) ;
#72771 = CARTESIAN_POINT ( 'NONE',  ( -4.495793269230770939, -5.876774720514410077, 19.27714342948718595 ) ) ;
#72772 = DIRECTION ( 'NONE',  ( 0.000000000000000000, 0.000000000000000000, 1.000000000000000000 ) ) ;
#72773 = CARTESIAN_POINT ( 'NONE',  ( 15.63414672909509839, 15.54323407889855879, 11.49999999999998934 ) ) ;
#72774 = CARTESIAN_POINT ( 'NONE',  ( -2.899999999999996803, 31.80000000000000071, 2.100000000000000089 ) ) ;
#72775 = ORIENTED_EDGE ( 'NONE', *, *, #73135, .T. ) ;
#72776 = DIRECTION ( 'NONE',  ( -3.773278334453079618E-23, 0.9999999999976377785, 2.173523156925979975E-06 ) ) ;
#72777 = PLANE ( 'NONE',  #37926 ) ;
#72778 = DIRECTION ( 'NONE',  ( 0.5543250044962501066, 0.000000000000000000, -0.8323003000060928969 ) ) ;
#72779 = CARTESIAN_POINT ( 'NONE',  ( -31.62374191384759925, -24.65952944569304250, 1.056160979905695463 ) ) ;
#72780 = VERTEX_POINT ( 'NONE', #92526 ) ;
#72781 = ORIENTED_EDGE ( 'NONE', *, *, #13328, .T. ) ;
#72782 = CARTESIAN_POINT ( 'NONE',  ( -118.5562042904834072, -24.66019654487199730, 8.947790411086121054 ) ) ;
#72783 = CARTESIAN_POINT ( 'NONE',  ( -100.4381051993576506, -25.10935802465470701, 2.832404819424185316 ) ) ;
#72784 = DIRECTION ( 'NONE',  ( 0.000000000000000000, 2.173523156925980399E-06, -0.9999999999976378895 ) ) ;
#72785 = CARTESIAN_POINT ( 'NONE',  ( -17.09319154528168383, -11.34935287704045948, -1.500000000000002220 ) ) ;
#72786 = ORIENTED_EDGE ( 'NONE', *, *, #97973, .T. ) ;
#72787 = DIRECTION ( 'NONE',  ( 0.000000000000000000, -1.000000000000000000, -1.020425574104004246E-16 ) ) ;
#72788 = CARTESIAN_POINT ( 'NONE',  ( 22.02124265030973760, 3.456774720514426136, 16.20402280011862217 ) ) ;
#72789 = DIRECTION ( 'NONE',  ( 0.000000000000000000, 0.000000000000000000, 1.000000000000000000 ) ) ;
#72790 = CARTESIAN_POINT ( 'NONE',  ( 18.98964132805693694, -11.70494588174365092, 11.49999999999998934 ) ) ;
#72791 = CARTESIAN_POINT ( 'NONE',  ( -0.05753151201984623569, -22.30520936630598072, 1.095224832288517858 ) ) ;
#72792 = ORIENTED_EDGE ( 'NONE', *, *, #89659, .T. ) ;
#72793 = CARTESIAN_POINT ( 'NONE',  ( -101.6228709571500559, -24.51283580621365132, 0.6167428607019800335 ) ) ;
#72794 = CARTESIAN_POINT ( 'NONE',  ( 3.748501943728875574, -5.876774720514426065, 21.47917144995767558 ) ) ;
#72795 = CARTESIAN_POINT ( 'NONE',  ( 11.47802407633690258, -17.41396394059345454, 11.49999999999998934 ) ) ;
#72796 = ORIENTED_EDGE ( 'NONE', *, *, #19918, .T. ) ;
#72798 = ORIENTED_EDGE ( 'NONE', *, *, #58250, .F. ) ;
#72797 = LINE ( 'NONE', #67190, #60378 ) ;
#72799 = VERTEX_POINT ( 'NONE', #31128 ) ;
#72800 = LINE ( 'NONE', #25618, #37375 ) ;
#72801 = CARTESIAN_POINT ( 'NONE',  ( 18.24537196375281312, 10.48796402029766739, -1.500000000000002220 ) ) ;
#72802 = EDGE_CURVE ( 'NONE', #59928, #8232, #62102, .T. ) ;
#72803 = VERTEX_POINT ( 'NONE', #85415 ) ;
#72804 = CARTESIAN_POINT ( 'NONE',  ( 6.184520403203634942, -6.376774720514426953, -25.32021290018218451 ) ) ;
#72805 = AXIS2_PLACEMENT_3D ( 'NONE', #98196, #66791, #36817 ) ;
#72807 = EDGE_CURVE ( 'NONE', #40031, #19500, #77293, .T. ) ;
#72806 = CARTESIAN_POINT ( 'NONE',  ( -37.52287095715006870, -24.50321055353803601, 9.387540953477520489 ) ) ;
#72808 = PLANE ( 'NONE',  #36759 ) ;
#72809 = VECTOR ( 'NONE', #59340, 1000.000000000000114 ) ;
#72810 = EDGE_CURVE ( 'NONE', #27095, #15127, #93520, .T. ) ;
#72811 = CARTESIAN_POINT ( 'NONE',  ( -101.9195342205254775, -25.03152194789300822, 6.392810880780148253 ) ) ;
#72812 = CARTESIAN_POINT ( 'NONE',  ( 4.143214286797170409, 4.821574250326516875, 3.549999999999996714 ) ) ;
#72813 = CARTESIAN_POINT ( 'NONE',  ( 7.679218611123722837, 20.28660689097963399, -1.500000000000002220 ) ) ;
#72814 = CARTESIAN_POINT ( 'NONE',  ( -81.48149462243461016, -25.24759629374391423, 6.293942980506744611 ) ) ;
#72816 = ORIENTED_EDGE ( 'NONE', *, *, #90792, .T. ) ;
#72815 = CARTESIAN_POINT ( 'NONE',  ( 14.93699691249320693, 16.48547057857716425, 11.49999999999999645 ) ) ;
#72817 = CARTESIAN_POINT ( 'NONE',  ( -51.52657066994672164, -25.24728931607062776, 6.155056572741268717 ) ) ;
#72818 = CARTESIAN_POINT ( 'NONE',  ( -105.5228709571500758, -23.47593901973090524, -1.443836447538996426 ) ) ;
#72819 = DIRECTION ( 'NONE',  ( 0.000000000000000000, 0.000000000000000000, -1.000000000000000000 ) ) ;
#72820 = ORIENTED_EDGE ( 'NONE', *, *, #79158, .T. ) ;
#72821 = EDGE_CURVE ( 'NONE', #6511, #57950, #70703, .T. ) ;
#72823 = VECTOR ( 'NONE', #81896, 1000.000000000000000 ) ;
#72822 = B_SPLINE_CURVE_WITH_KNOTS ( 'NONE', 3,
 ( #93049, #30160, #61134, #54508 ),
 .UNSPECIFIED., .F., .F.,
 ( 4, 4 ),
 ( 2.796599675949392459E-06, 0.0004696118376083021489 ),
 .UNSPECIFIED. ) ;
#72824 = ADVANCED_FACE ( 'NONE', ( #684 ), #39242, .T. ) ;
#72826 = ORIENTED_EDGE ( 'NONE', *, *, #35575, .F. ) ;
#72825 = CARTESIAN_POINT ( 'NONE',  ( -6.602379858799704238, -6.376774720514410077, 19.46575348430202723 ) ) ;
#72827 = AXIS2_PLACEMENT_3D ( 'NONE', #43454, #11987, #35830 ) ;
#72828 = EDGE_LOOP ( 'NONE', ( #1807, #96532, #31990, #57413 ) ) ;
#72829 = AXIS2_PLACEMENT_3D ( 'NONE', #34572, #36056, #19327 ) ;
#72830 = DIRECTION ( 'NONE',  ( -1.000000000000000000, -4.476705744456278313E-16, 0.000000000000000000 ) ) ;
#72831 = CARTESIAN_POINT ( 'NONE',  ( -107.5228709571501042, -24.51283580621451108, 0.6167428607045601918 ) ) ;
#72832 = CARTESIAN_POINT ( 'NONE',  ( 29.73860345376319358, -5.356653620851810516, 18.57591152018007463 ) ) ;
#72833 = ORIENTED_EDGE ( 'NONE', *, *, #54260, .F. ) ;
#72834 = CARTESIAN_POINT ( 'NONE',  ( -130.5728709571500588, -25.32188240763692733, 6.439777313841902107 ) ) ;
#72835 = CARTESIAN_POINT ( 'NONE',  ( -0.1411031551986380028, 22.44022050402121948, -1.500000000000002220 ) ) ;
#72836 = ORIENTED_EDGE ( 'NONE', *, *, #20583, .T. ) ;
#72837 = CARTESIAN_POINT ( 'NONE',  ( -108.8968792378191921, -29.50249917535260380, 7.447779886225679213 ) ) ;
#72838 = CARTESIAN_POINT ( 'NONE',  ( -44.92287095715006018, -23.47593901973090169, -1.443836447538997980 ) ) ;
#72839 = DIRECTION ( 'NONE',  ( 0.000000000000000000, 2.173523156925980399E-06, -0.9999999999976378895 ) ) ;
#72840 = CARTESIAN_POINT ( 'NONE',  ( -29.49875734969026198, -0.3587747205144265483, 2.362022800118626531 ) ) ;
#72841 = CARTESIAN_POINT ( 'NONE',  ( -97.24175110560238977, -25.14081846633248318, 7.291654623549835179 ) ) ;
#72842 = CARTESIAN_POINT ( 'NONE',  ( 12.01011565470214393, -15.49198969801113890, -1.500000000000002220 ) ) ;
#72843 = FACE_OUTER_BOUND ( 'NONE', #64932, .T. ) ;
#72844 = ORIENTED_EDGE ( 'NONE', *, *, #15633, .F. ) ;
#72845 = CARTESIAN_POINT ( 'NONE',  ( -7.320277434469578459, 20.25297033093062282, 11.49999999999998934 ) ) ;
#72846 = CARTESIAN_POINT ( 'NONE',  ( -24.90875734969025501, -6.376774720514426953, 30.51402280011862089 ) ) ;
#72847 = CARTESIAN_POINT ( 'NONE',  ( -80.53911428444936860, -25.30394759708685015, 4.969307535586566793 ) ) ;
#72848 = PLANE ( 'NONE',  #66886 ) ;
#72849 = CARTESIAN_POINT ( 'NONE',  ( -41.86995616089613748, -29.50249213948574933, 4.210700559310249780 ) ) ;
#72850 = CARTESIAN_POINT ( 'NONE',  ( 16.30191990219073972, -16.09819076282585826, -1.500000000000002220 ) ) ;
#72851 = B_SPLINE_CURVE_WITH_KNOTS ( 'NONE', 3,
 ( #98375, #97394, #5042, #34996 ),
 .UNSPECIFIED., .F., .F.,
 ( 4, 4 ),
 ( 3.316619621408722944E-09, 0.002461457897985275343 ),
 .UNSPECIFIED. ) ;
#72852 = DATE_AND_TIME ( #18549, #89389 ) ;
#72853 = DIRECTION ( 'NONE',  ( 0.000000000000000000, -1.000000000000000000, 0.000000000000000000 ) ) ;
#72854 = CARTESIAN_POINT ( 'NONE',  ( 0.8635838190919263857, -3.990505948720459717, 8.999999999999994671 ) ) ;
#72855 = CARTESIAN_POINT ( 'NONE',  ( -11.83016301840747175, -16.26703346747452983, 11.49999999999999645 ) ) ;
#72856 = PLANE ( 'NONE',  #70572 ) ;
#72857 = CARTESIAN_POINT ( 'NONE',  ( -32.59411303382088931, -24.15620529776627734, 10.23563542870661358 ) ) ;
#72858 = B_SPLINE_CURVE_WITH_KNOTS ( 'NONE', 3,
 ( #57648, #48540, #94688, #72868, #9957, #87078 ),
 .UNSPECIFIED., .F., .F.,
 ( 4, 2, 4 ),
 ( 0.000000000000000000, 0.001380764517854768001, 0.002761529035709536003 ),
 .UNSPECIFIED. ) ;
#72859 = DIRECTION ( 'NONE',  ( 0.000000000000000000, 0.000000000000000000, -1.000000000000000000 ) ) ;
#72860 = CARTESIAN_POINT ( 'NONE',  ( 14.78484767477523398, 5.152774720514430307, -28.43034250232788551 ) ) ;
#72861 = CARTESIAN_POINT ( 'NONE',  ( 15.22325621495362391, 3.582999323269832725, -27.23549315679322547 ) ) ;
#72862 = CARTESIAN_POINT ( 'NONE',  ( -19.21288746854601115, 4.878285775029977955, 11.49999999999998934 ) ) ;
#72863 = B_SPLINE_CURVE_WITH_KNOTS ( 'NONE', 3,
 ( #79443, #11437, #71848, #2845, #58619, #3351 ),
 .UNSPECIFIED., .F., .F.,
 ( 4, 2, 4 ),
 ( 1.570887131794638196E-05, 0.001396322306279761940, 0.002776935741241577573 ),
 .UNSPECIFIED. ) ;
#72864 = CARTESIAN_POINT ( 'NONE',  ( -90.62287095715001328, -24.63345952396257843, 9.038047939301508293 ) ) ;
#72865 = CARTESIAN_POINT ( 'NONE',  ( -9.297559507673007317, 17.40068379117045083, -1.500000000000002220 ) ) ;
#72866 = CARTESIAN_POINT ( 'NONE',  ( 29.73860345376319358, 1.477225279485574028, 7.190646357373898680E-15 ) ) ;
#72867 = ITEM_DEFINED_TRANSFORMATION ( 'NONE', 'NONE', #66673,  #37391 ) ;
#72868 = CARTESIAN_POINT ( 'NONE',  ( -103.5228709571500758, -23.94994826722565406, -0.6494450866342691420 ) ) ;
#72869 = CARTESIAN_POINT ( 'NONE',  ( 3.121233215686890272, -6.376774720514404748, 18.93204046835445808 ) ) ;
#72870 = CARTESIAN_POINT ( 'NONE',  ( 17.30552477474510908, -11.17933342135444086, 11.49999999999999645 ) ) ;
#72872 = EDGE_CURVE ( 'NONE', #84333, #23301, #17519, .T. ) ;
#72871 = AXIS2_PLACEMENT_3D ( 'NONE', #80428, #57112, #74317 ) ;
#72873 = CARTESIAN_POINT ( 'NONE',  ( -116.6228709571500559, -29.50250243563736774, 8.947779886222134493 ) ) ;
#72874 = CARTESIAN_POINT ( 'NONE',  ( 12.64511023617726160, -18.80563239904246231, 11.49999999999999645 ) ) ;
#72875 = ORIENTED_EDGE ( 'NONE', *, *, #58225, .T. ) ;
#72876 = ADVANCED_FACE ( 'NONE', ( #77789 ), #14900, .F. ) ;
#72877 = CARTESIAN_POINT ( 'NONE',  ( -69.35973275182155362, -25.25639446185967785, 6.387116080414448227 ) ) ;
#72878 = FACE_OUTER_BOUND ( 'NONE', #32580, .T. ) ;
#72879 = AXIS2_PLACEMENT_3D ( 'NONE', #100048, #75723, #22922 ) ;
#72880 = CARTESIAN_POINT ( 'NONE',  ( -27.55559746109228669, -24.61460113352056567, 8.249645512891413901 ) ) ;
#72881 = CARTESIAN_POINT ( 'NONE',  ( -36.52287095715006870, -23.48783264082477018, -1.443836473390097019 ) ) ;
#72882 = VECTOR ( 'NONE', #13384, 1000.000000000000000 ) ;
#72883 = ORIENTED_EDGE ( 'NONE', *, *, #30405, .T. ) ;
#72884 = CARTESIAN_POINT ( 'NONE',  ( -79.98791220707269645, -25.31596236519360588, 5.033164519372586021 ) ) ;
#72885 = CARTESIAN_POINT ( 'NONE',  ( -21.74551633039419585, 6.958787177381512201, 11.49999999999998934 ) ) ;
#72886 = CARTESIAN_POINT ( 'NONE',  ( 30.61643171304413613, -6.376774720514426953, 27.37433008668288181 ) ) ;
#72887 = AXIS2_PLACEMENT_3D ( 'NONE', #31194, #54545, #60181 ) ;
#72888 = DIRECTION ( 'NONE',  ( -0.6392559695863502256, -6.454799914155189828E-16, -0.7689940216596065081 ) ) ;
#72889 = CARTESIAN_POINT ( 'NONE',  ( -82.55439147425074964, -23.96169478059713143, 10.65365249895718414 ) ) ;
#72890 = CARTESIAN_POINT ( 'NONE',  ( -16.74552829020559130, -14.98668287627115170, 11.49999999999999645 ) ) ;
#72891 = ORIENTED_EDGE ( 'NONE', *, *, #65079, .T. ) ;
#72892 = AXIS2_PLACEMENT_3D ( 'NONE', #48772, #96930, #18799 ) ;
#72893 = B_SPLINE_CURVE_WITH_KNOTS ( 'NONE', 3,
 ( #99895, #85701, #7572, #69474 ),
 .UNSPECIFIED., .F., .F.,
 ( 4, 4 ),
 ( 0.000000000000000000, 9.999999999998897304E-05 ),
 .UNSPECIFIED. ) ;
#72894 = CARTESIAN_POINT ( 'NONE',  ( -69.55126625704997423, -25.15208592601422311, 3.076695591939294427 ) ) ;
#72895 = CARTESIAN_POINT ( 'NONE',  ( -19.44315311050126382, -10.23602577120861667, -1.500000000000002220 ) ) ;
#72896 = CARTESIAN_POINT ( 'NONE',  ( -125.5801350442859246, -25.31825869351653679, 3.539998670762456889 ) ) ;
#72898 = CARTESIAN_POINT ( 'NONE',  ( -111.5146153425688169, -24.51314013834316796, 0.6176544820404207270 ) ) ;
#72897 = AXIS2_PLACEMENT_3D ( 'NONE', #69173, #100093, #30607 ) ;
#72899 = PLANE ( 'NONE',  #83206 ) ;
#72900 = ORIENTED_EDGE ( 'NONE', *, *, #10733, .F. ) ;
#72901 = CARTESIAN_POINT ( 'NONE',  ( -48.56838548480330076, -23.48786465467241058, 11.44779295918254824 ) ) ;
#72902 = FACE_OUTER_BOUND ( 'NONE', #71031, .T. ) ;
#72903 = ORIENTED_EDGE ( 'NONE', *, *, #68919, .T. ) ;
#72904 = CARTESIAN_POINT ( 'NONE',  ( -54.53280603000485627, -24.66019654487199375, 8.947790411086119278 ) ) ;
#72905 = CARTESIAN_POINT ( 'NONE',  ( -14.05295919346176170, -14.94737400546395456, -1.500000000000002220 ) ) ;
#72906 = ORIENTED_EDGE ( 'NONE', *, *, #80119, .F. ) ;
#72907 = ORIENTED_EDGE ( 'NONE', *, *, #23050, .T. ) ;
#72908 = ORIENTED_EDGE ( 'NONE', *, *, #17189, .T. ) ;
#72909 = CARTESIAN_POINT ( 'NONE',  ( 2.955024617976266033, -6.376774720514415407, 20.58370193283586858 ) ) ;
#72910 = CARTESIAN_POINT ( 'NONE',  ( 8.286623624103266097E-13, -23.05000000000000426, -1.500000000000002220 ) ) ;
#72911 = CARTESIAN_POINT ( 'NONE',  ( 14.47945362154702664, 3.630796101029369005, -28.34983287945846087 ) ) ;
#72912 = CARTESIAN_POINT ( 'NONE',  ( 10.94010344783756672, -17.16519937159427656, -1.500000000000002220 ) ) ;
#72913 = ORIENTED_EDGE ( 'NONE', *, *, #50775, .F. ) ;
#72914 = CARTESIAN_POINT ( 'NONE',  ( 22.81105451610979173, -1.477225279485574028, -18.46691820600746681 ) ) ;
#72915 = CARTESIAN_POINT ( 'NONE',  ( -29.60196408342335772, -23.88237758481870188, 10.65365256123546978 ) ) ;
#72916 = ADVANCED_FACE ( 'NONE', ( #8803 ), #54478, .T. ) ;
#72917 = CARTESIAN_POINT ( 'NONE',  ( -105.5543693429755052, -24.15503026093913519, -0.2815557561904565298 ) ) ;
#72918 = CARTESIAN_POINT ( 'NONE',  ( -71.70602904702231228, -25.25855097290165574, 6.253518357416208318 ) ) ;
#72919 = VERTEX_POINT ( 'NONE', #46866 ) ;
#72920 = CARTESIAN_POINT ( 'NONE',  ( -29.19847332116389538, -25.21532038932136643, 4.026235508823390319 ) ) ;
#72921 = CARTESIAN_POINT ( 'NONE',  ( -49.59506520832605503, -25.31573813936321216, 4.856709705808007982 ) ) ;
#72922 = VERTEX_POINT ( 'NONE', #16399 ) ;
#72923 = CARTESIAN_POINT ( 'NONE',  ( -2.730994233912177549, 20.60462238790213618, -1.500000000000002220 ) ) ;
#72924 = ORIENTED_EDGE ( 'NONE', *, *, #93546, .T. ) ;
#72926 = ORIENTED_EDGE ( 'NONE', *, *, #80374, .F. ) ;
#72925 = CARTESIAN_POINT ( 'NONE',  ( -39.64514910329782538, -25.30345942151094007, 4.760327011971625666 ) ) ;
#72927 = DIRECTION ( 'NONE',  ( 0.000000000000000000, 0.000000000000000000, 1.000000000000000000 ) ) ;
#72928 = LINE ( 'NONE', #48603, #94016 ) ;
#72929 = ORIENTED_EDGE ( 'NONE', *, *, #56483, .T. ) ;
#72930 = ORIENTED_EDGE ( 'NONE', *, *, #89197, .T. ) ;
#72931 = CARTESIAN_POINT ( 'NONE',  ( -77.62287095715005592, -29.50250786944525672, 11.44777988621623521 ) ) ;
#72932 = EDGE_CURVE ( 'NONE', #83384, #19254, #26076, .T. ) ;
#72933 = PLANE ( 'NONE',  #52991 ) ;
#72934 = CARTESIAN_POINT ( 'NONE',  ( -71.15736797201716968, -25.31201676987124927, 5.711157391728908017 ) ) ;
#72936 = VERTEX_POINT ( 'NONE', #63103 ) ;
#72935 = CARTESIAN_POINT ( 'NONE',  ( 21.54648482299927181, -4.703075207800759827, 11.49999999999999645 ) ) ;
#72937 = CARTESIAN_POINT ( 'NONE',  ( -50.52287095715007581, -25.00182538069144655, 7.747789668545104647 ) ) ;
#72938 = EDGE_CURVE ( 'NONE', #98879, #65855, #82787, .T. ) ;
#72939 = CARTESIAN_POINT ( 'NONE',  ( 19.13181028273733375, 12.02906595412573232, 11.49999999999998934 ) ) ;
#72940 = EDGE_CURVE ( 'NONE', #21005, #53793, #67130, .T. ) ;
#72942 = VERTEX_POINT ( 'NONE', #32130 ) ;
#72941 = CARTESIAN_POINT ( 'NONE',  ( -70.62287095715005592, -24.14321612903114556, -0.2833117244521698996 ) ) ;
#72943 = ADVANCED_FACE ( 'NONE', ( #55485 ), #86423, .T. ) ;
#72944 = EDGE_LOOP ( 'NONE', ( #38293, #97701, #48848, #26337, #49979 ) ) ;
#72945 = ADVANCED_FACE ( 'NONE', ( #63611 ), #72212, .F. ) ;
#72946 = DIRECTION ( 'NONE',  ( 0.000000000000000000, -2.173523156925979552E-06, 0.9999999999976378895 ) ) ;
#72947 = CIRCLE ( 'NONE', #24324, 130.2784398600581710 ) ;
#72948 = CARTESIAN_POINT ( 'NONE',  ( -36.52287095715006870, -24.64965694238407323, 8.947790433994205372 ) ) ;
#72949 = VERTEX_POINT ( 'NONE', #42283 ) ;
#72950 = CARTESIAN_POINT ( 'NONE',  ( -1.756177585742932479, 21.11346882147791959, -1.500000000000002220 ) ) ;
#72951 = CARTESIAN_POINT ( 'NONE',  ( -78.97085663747836293, -25.27791698645071250, 6.301135832498177436 ) ) ;
#72952 = VECTOR ( 'NONE', #61551, 1000.000000000000000 ) ;
#72953 = CARTESIAN_POINT ( 'NONE',  ( -7.264088518202086675, -5.876774720514411854, 19.78976258633487717 ) ) ;
#72954 = CARTESIAN_POINT ( 'NONE',  ( -39.62287095715005592, -23.47593901973091235, -1.443836447539011525 ) ) ;
#72955 = CARTESIAN_POINT ( 'NONE',  ( -8.951960448472247478, 20.35530821588910300, -1.500000000000002220 ) ) ;
#72956 = CARTESIAN_POINT ( 'NONE',  ( -49.32147450118114307, -25.03220824940797584, 7.186702319186736965 ) ) ;
#72957 = ADVANCED_FACE ( 'NONE', ( #3210 ), #7805, .T. ) ;
#72958 = ORIENTED_EDGE ( 'NONE', *, *, #29005, .F. ) ;
#72959 = PLANE ( 'NONE',  #9274 ) ;
#72960 = FACE_OUTER_BOUND ( 'NONE', #56103, .T. ) ;
#72961 = CIRCLE ( 'NONE', #28963, 2.350000000000000089 ) ;
#72962 = CARTESIAN_POINT ( 'NONE',  ( -36.64924296586449515, -23.96169478059712432, 10.65365249895718591 ) ) ;
#72963 = FACE_OUTER_BOUND ( 'NONE', #84480, .T. ) ;
#72964 = VECTOR ( 'NONE', #88799, 1000.000000000000000 ) ;
#72965 = CARTESIAN_POINT ( 'NONE',  ( -12.17249226084429203, 15.20430173202493940, 11.49999999999998934 ) ) ;
#72966 = VECTOR ( 'NONE', #81629, 1000.000000000000114 ) ;
#72967 = CARTESIAN_POINT ( 'NONE',  ( 21.15477495681221143, 3.540436534888726783, 11.49999999999998934 ) ) ;
#72968 = CARTESIAN_POINT ( 'NONE',  ( -27.26447433122779884, -24.57999507273727247, 1.676005322195218916 ) ) ;
#72969 = CARTESIAN_POINT ( 'NONE',  ( -51.48601377777728771, -24.65952944569304250, 1.056160979905695463 ) ) ;
#72970 = CARTESIAN_POINT ( 'NONE',  ( -77.62998606892628572, -24.34968618360934300, 0.1864209137778811143 ) ) ;
#72971 = B_SPLINE_CURVE_WITH_KNOTS ( 'NONE', 3,
 ( #27646, #65728, #13892, #43376 ),
 .UNSPECIFIED., .F., .F.,
 ( 4, 4 ),
 ( 0.000000000000000000, 1.000000000000000000 ),
 .UNSPECIFIED. ) ;
#72972 = CARTESIAN_POINT ( 'NONE',  ( -2.780358639097238349, 22.57001311929844434, -1.500000000000002220 ) ) ;
#72973 = B_SPLINE_CURVE_WITH_KNOTS ( 'NONE', 3,
 ( #90144, #66331, #20620, #27747, #58697, #57711 ),
 .UNSPECIFIED., .F., .F.,
 ( 4, 2, 4 ),
 ( 0.000000000000000000, 0.001380901958385383774, 0.002761803916770767548 ),
 .UNSPECIFIED. ) ;
#72974 = VECTOR ( 'NONE', #15895, 1000.000000000000114 ) ;
#72975 = CIRCLE ( 'NONE', #98877, 2.040000000000000036 ) ;
#72976 = CARTESIAN_POINT ( 'NONE',  ( -102.5221945332385758, -23.48783264082478084, -1.443836473390064379 ) ) ;
#72977 = CARTESIAN_POINT ( 'NONE',  ( -88.52287095715006160, -29.50247984919015209, -1.443849546365051806 ) ) ;
#72978 = CARTESIAN_POINT ( 'NONE',  ( 4.721227339208565965, -19.33841413273825793, 11.49999999999999645 ) ) ;
#72979 = LINE ( 'NONE', #57268, #34070 ) ;
#72980 = CARTESIAN_POINT ( 'NONE',  ( -39.49832869534071733, -24.15620529776627734, 10.23563542870661180 ) ) ;
#72981 = CARTESIAN_POINT ( 'NONE',  ( 6.660000000000001030, 7.578413286920094194, 5.288828319098143105 ) ) ;
#72982 = ORIENTED_EDGE ( 'NONE', *, *, #48997, .F. ) ;
#72983 = CARTESIAN_POINT ( 'NONE',  ( 32.15269211224249091, 4.540774720514427543, 3.401810532325273417 ) ) ;
#72984 = EDGE_CURVE ( 'NONE', #71754, #7198, #85252, .T. ) ;
#72985 = CARTESIAN_POINT ( 'NONE',  ( -32.40928876965531913, -25.16202561908117730, 2.791798636425737445 ) ) ;
#72986 = CARTESIAN_POINT ( 'NONE',  ( 19.26462925850498920, -9.998780574493274287, -1.500000000000002220 ) ) ;
#72987 = CARTESIAN_POINT ( 'NONE',  ( -1.358974358974355257, -6.376774720514427841, 21.75000000000000711 ) ) ;
#72988 = CARTESIAN_POINT ( 'NONE',  ( -4.924063254364682507, -18.92933890202812464, -1.500000000000002220 ) ) ;
#72989 = CARTESIAN_POINT ( 'NONE',  ( -19.37210865224160017, 5.965225279485592225, -21.60955166348795586 ) ) ;
#72990 = ADVANCED_FACE ( 'NONE', ( #33644 ), #34647, .F. ) ;
#72991 = EDGE_LOOP ( 'NONE', ( #85671, #43819, #87121, #59832, #69210, #1411, #56830, #25467, #57923, #92072, #80829, #76731, #80821, #38865, #23078, #34137, #40821, #22119, #79020, #61008, #10846, #85654, #81146, #26738, #97197, #24057, #71004, #17606, #3662, #72651, #63748, #9358, #32802, #97238, #83271, #5627, #69795, #50650, #16751, #26009, #93334, #76125, #62651, #46214, #30646, #27711 ) ) ;
#72992 = DATE_AND_TIME ( #42048, #29542 ) ;
#72993 = FACE_OUTER_BOUND ( 'NONE', #1, .T. ) ;
#72994 = CARTESIAN_POINT ( 'NONE',  ( -4.302178748239556150, -20.00421716419250373, 11.49999999999999645 ) ) ;
#72995 = CARTESIAN_POINT ( 'NONE',  ( -82.62287095715005592, -23.48783264082478084, -1.443836473390065933 ) ) ;
#72996 = EDGE_CURVE ( 'NONE', #18460, #75143, #44118, .T. ) ;
#72997 = CARTESIAN_POINT ( 'NONE',  ( -89.52287095715011844, -24.33832256527049154, 0.1851278514138623987 ) ) ;
#72998 = ORIENTED_EDGE ( 'NONE', *, *, #54445, .F. ) ;
#72999 = EDGE_CURVE ( 'NONE', #78995, #28435, #35644, .T. ) ;
#73000 = CARTESIAN_POINT ( 'NONE',  ( -62.62287095715004881, -23.48783264082478794, -1.443836473390068820 ) ) ;
#73001 = CARTESIAN_POINT ( 'NONE',  ( 33.61456970919608978, 3.316774720514426900, -11.35828564741662028 ) ) ;
#73002 = DIRECTION ( 'NONE',  ( 0.2488812114211666759, 0.000000000000000000, 0.9685340172660599212 ) ) ;
#73003 = CARTESIAN_POINT ( 'NONE',  ( -63.58953762381673869, -23.47596703998600276, 11.44779298504227505 ) ) ;
#73004 = VERTEX_POINT ( 'NONE', #43261 ) ;
#73005 = DIRECTION ( 'NONE',  ( -3.773278334453079030E-23, 0.9999999999976377785, 2.173523156925979128E-06 ) ) ;
#73006 = B_SPLINE_CURVE_WITH_KNOTS ( 'NONE', 3,
 ( #45813, #39189, #38185, #54428 ),
 .UNSPECIFIED., .F., .F.,
 ( 4, 4 ),
 ( 0.000000000000000000, 9.999999999994735322E-05 ),
 .UNSPECIFIED. ) ;
#73007 = B_SPLINE_CURVE_WITH_KNOTS ( 'NONE', 3,
 ( #93553, #62132, #56527, #47402, #85956, #16433, #86954, #17948 ),
 .UNSPECIFIED., .F., .F.,
 ( 4, 2, 2, 4 ),
 ( 0.000000000000000000, 0.002001079623178227129, 0.003001619434767338959, 0.004002159246356450789 ),
 .UNSPECIFIED. ) ;
#73008 = CARTESIAN_POINT ( 'NONE',  ( -17.45619364963476627, 14.87644265977633573, 11.49999999999999645 ) ) ;
#73009 = CARTESIAN_POINT ( 'NONE',  ( -12.51292883401962541, 18.98408452820241266, 11.49999999999998934 ) ) ;
#73010 = CARTESIAN_POINT ( 'NONE',  ( -71.44728056806559380, -25.14542524405617385, 7.034487670647322055 ) ) ;
#73011 = CARTESIAN_POINT ( 'NONE',  ( 0.000000000000000000, -1.473225279485573802, 0.000000000000000000 ) ) ;
#73012 = CARTESIAN_POINT ( 'NONE',  ( -90.51172207313412343, -24.15503026093913164, -0.2815557561904542538 ) ) ;
#73013 = PLANE ( 'NONE',  #10694 ) ;
#73014 = DIRECTION ( 'NONE',  ( 0.000000000000000000, -0.000000000000000000, -1.000000000000000000 ) ) ;
#73015 = AXIS2_PLACEMENT_3D ( 'NONE', #94503, #64086, #72678 ) ;
#73016 = CARTESIAN_POINT ( 'NONE',  ( 3.414333255021221092, 21.62243999391013105, 11.49999999999998934 ) ) ;
#73017 = CC_DESIGN_PERSON_AND_ORGANIZATION_ASSIGNMENT ( #73713, #4208, ( #92779 ) ) ;
#73018 = CARTESIAN_POINT ( 'NONE',  ( 8.160000000000000142, 8.793627758918228565, -2.994553991265763049 ) ) ;
#73019 = CARTESIAN_POINT ( 'NONE',  ( -26.49532332504551135, -24.82382521439767942, 2.996894461300356305 ) ) ;
#73020 = CARTESIAN_POINT ( 'NONE',  ( 9.150000000000003908, -5.876774720514426953, 11.88602120139451834 ) ) ;
#73021 = CARTESIAN_POINT ( 'NONE',  ( 9.019313479210174123, -0.9107773096390185952, 3.707288619710388478 ) ) ;
#73022 = ORIENTED_EDGE ( 'NONE', *, *, #82964, .F. ) ;
#73023 = CARTESIAN_POINT ( 'NONE',  ( -18.16121111207539940, 9.348575961806686152, -1.500000000000002220 ) ) ;
#73024 = EDGE_LOOP ( 'NONE', ( #38700, #66337, #87624, #47382 ) ) ;
#73025 = ORIENTED_EDGE ( 'NONE', *, *, #45108, .T. ) ;
#73026 = ORIENTED_EDGE ( 'NONE', *, *, #86902, .T. ) ;
#73027 = CARTESIAN_POINT ( 'NONE',  ( 22.09143763772896918, 6.410036269187016522, -1.500000000000002220 ) ) ;
#73028 = CARTESIAN_POINT ( 'NONE',  ( -39.52287095715006870, -23.47596703998600631, 11.44779298504229281 ) ) ;
#73029 = CARTESIAN_POINT ( 'NONE',  ( -17.93149374516376682, -9.230432107326475233, -1.500000000000002220 ) ) ;
#73030 = VERTEX_POINT ( 'NONE', #75184 ) ;
#73031 = CARTESIAN_POINT ( 'NONE',  ( 15.92621150404962016, -6.475225279485573360, -27.29681269571043245 ) ) ;
#73032 = CARTESIAN_POINT ( 'NONE',  ( 8.971512145086503409, -1.028487854913504362, -3.750000000000000000 ) ) ;
#73034 = DIRECTION ( 'NONE',  ( -3.773278334453079030E-23, 0.9999999999976377785, 2.173523156925979128E-06 ) ) ;
#73033 = AXIS2_PLACEMENT_3D ( 'NONE', #90419, #59478, #12285 ) ;
#73035 = DIRECTION ( 'NONE',  ( 3.773278334444166432E-23, -1.000000000000000000, 0.000000000000000000 ) ) ;
#73037 = VERTEX_POINT ( 'NONE', #50872 ) ;
#73036 = CARTESIAN_POINT ( 'NONE',  ( 20.92345209525186078, -4.499874906010187026, 11.49999999999999645 ) ) ;
#73038 = DIRECTION ( 'NONE',  ( 0.7071067811865507924, 0.000000000000000000, -0.7071067811865442421 ) ) ;
#73039 = VECTOR ( 'NONE', #85759, 1000.000000000000227 ) ;
#73040 = VERTEX_POINT ( 'NONE', #81811 ) ;
#73041 = CARTESIAN_POINT ( 'NONE',  ( -9.338385371603758145, -20.21602636099808237, -1.500000000000002220 ) ) ;
#73042 = CARTESIAN_POINT ( 'NONE',  ( -9.011640028862021978, 18.61544202926687674, 11.49999999999998934 ) ) ;
#73043 = CIRCLE ( 'NONE', #85984, 3.570000000000003837 ) ;
#73044 = ORIENTED_EDGE ( 'NONE', *, *, #92917, .F. ) ;
#73045 = B_SPLINE_CURVE_WITH_KNOTS ( 'NONE', 3,
 ( #85644, #92744, #63333, #23228 ),
 .UNSPECIFIED., .F., .F.,
 ( 4, 4 ),
 ( 0.1305932534456737681, 0.1395996847177894684 ),
 .UNSPECIFIED. ) ;
#73046 = LINE ( 'NONE', #43092, #76114 ) ;
#73047 = ORIENTED_EDGE ( 'NONE', *, *, #29367, .F. ) ;
#73048 = B_SPLINE_CURVE_WITH_KNOTS ( 'NONE', 3,
 ( #25156, #2342, #88076, #80956 ),
 .UNSPECIFIED., .F., .F.,
 ( 4, 4 ),
 ( 0.2706932954563583404, 0.2796997267284738742 ),
 .UNSPECIFIED. ) ;
#73049 = CARTESIAN_POINT ( 'NONE',  ( -0.7395115731254272573, 18.09566585216508727, 8.999999999999998224 ) ) ;
#73050 = VERTEX_POINT ( 'NONE', #98014 ) ;
#73051 = CARTESIAN_POINT ( 'NONE',  ( 10.81255391457704640, -3.316774720514425123, -28.05044903510771803 ) ) ;
#73052 = CARTESIAN_POINT ( 'NONE',  ( 0.8316226063609513108, 20.92010288561657205, -1.500000000000002220 ) ) ;
#73053 = EDGE_CURVE ( 'NONE', #9400, #34090, #52562, .T. ) ;
#73054 = CARTESIAN_POINT ( 'NONE',  ( -20.07106029494397248, -8.819774368769808248, 11.49999999999999645 ) ) ;
#73055 = CARTESIAN_POINT ( 'NONE',  ( -26.35118574718723750, -24.77993572289172874, 6.568084281490178533 ) ) ;
#73056 = CARTESIAN_POINT ( 'NONE',  ( 14.32739804834607256, 17.34395043298086847, 11.49999999999998934 ) ) ;
#73057 = CARTESIAN_POINT ( 'NONE',  ( 7.003190781191628744, -19.75400906848480176, -1.500000000000002220 ) ) ;
#73058 = LINE ( 'NONE', #34485, #91889 ) ;
#73059 = DIRECTION ( 'NONE',  ( 0.6599726524652352877, 0.000000000000000000, -0.7512896232465891000 ) ) ;
#73060 = LINE ( 'NONE', #83646, #54099 ) ;
#73061 = ORIENTED_EDGE ( 'NONE', *, *, #63335, .T. ) ;
#73062 = EDGE_CURVE ( 'NONE', #94697, #92089, #35561, .T. ) ;
#73063 = EDGE_LOOP ( 'NONE', ( #24734, #6869, #7715, #75766 ) ) ;
#73064 = ORIENTED_EDGE ( 'NONE', *, *, #18337, .T. ) ;
#73065 = EDGE_CURVE ( 'NONE', #37215, #35231, #98541, .T. ) ;
#73066 = CARTESIAN_POINT ( 'NONE',  ( -44.52287095715006160, -23.48786465467241058, 11.44779295918255180 ) ) ;
#73067 = EDGE_LOOP ( 'NONE', ( #78245, #49840, #24903, #19589 ) ) ;
#73068 = CARTESIAN_POINT ( 'NONE',  ( 19.99361899508246765, -7.638522130635823082, -1.500000000000002220 ) ) ;
#73069 = ORIENTED_EDGE ( 'NONE', *, *, #5196, .F. ) ;
#73070 = CARTESIAN_POINT ( 'NONE',  ( 0.1309051665272248643, -5.876774720514413630, 19.34190049657482291 ) ) ;
#73071 = CARTESIAN_POINT ( 'NONE',  ( -1.999300432013352058, 20.99099883833691749, 11.49999999999998934 ) ) ;
#73072 = CARTESIAN_POINT ( 'NONE',  ( -30.62469739314999373, -24.05799227682217634, 10.47557002954947336 ) ) ;
#73073 = CARTESIAN_POINT ( 'NONE',  ( 2.649863049427662709, -6.376774720514420736, 20.71861240329949538 ) ) ;
#73074 = PLANE ( 'NONE',  #43769 ) ;
#73075 = DIRECTION ( 'NONE',  ( -3.773278334453079030E-23, 0.9999999999976377785, 2.173523156925979128E-06 ) ) ;
#73076 = CARTESIAN_POINT ( 'NONE',  ( -129.6239067399031342, -23.48786465467242124, 11.44779295918253936 ) ) ;
#73077 = CARTESIAN_POINT ( 'NONE',  ( -12.30081598482267680, 18.28176383447183895, -1.500000000000002220 ) ) ;
#73078 = ORIENTED_EDGE ( 'NONE', *, *, #70524, .F. ) ;
#73079 = CARTESIAN_POINT ( 'NONE',  ( -65.63297214418551562, -24.63419186844610920, 9.035850630976922204 ) ) ;
#73080 = EDGE_CURVE ( 'NONE', #15484, #51301, #29535, .T. ) ;
#73081 = CARTESIAN_POINT ( 'NONE',  ( -103.6228709571500559, -29.50250786944525672, 11.44777988621623166 ) ) ;
#73082 = CARTESIAN_POINT ( 'NONE',  ( 9.478389368232452483, -2.682774720514426559, -23.17485683983816003 ) ) ;
#73083 = CARTESIAN_POINT ( 'NONE',  ( -28.41342374310426067, -24.65886721645977531, 1.590605884330587916 ) ) ;
#73084 = CARTESIAN_POINT ( 'NONE',  ( -25.53321325151840426, -24.91491875925870048, 4.756813972840990168 ) ) ;
#73085 = CARTESIAN_POINT ( 'NONE',  ( -47.52287095715006160, -24.64898659630528854, 1.056161002820821038 ) ) ;
#73086 = CARTESIAN_POINT ( 'NONE',  ( 18.61059577090848549, -10.47110149595715711, 11.49999999999998934 ) ) ;
#73087 = DIRECTION ( 'NONE',  ( 0.000000000000000000, -0.9999999999976377785, -2.173523156925979975E-06 ) ) ;
#73088 = CARTESIAN_POINT ( 'NONE',  ( -91.16175232477891655, -25.26266127311081888, 3.981777872396910389 ) ) ;
#73089 = CARTESIAN_POINT ( 'NONE',  ( -64.64156214474047601, -23.96169478059713498, 10.65365249895718058 ) ) ;
#73090 = CARTESIAN_POINT ( 'NONE',  ( -68.58953762381672448, -23.48783264082478439, -1.443836473390067265 ) ) ;
#73091 = CARTESIAN_POINT ( 'NONE',  ( -4.885077187424587741, 22.05487924249641551, -1.500000000000002220 ) ) ;
#73092 = FACE_OUTER_BOUND ( 'NONE', #56308, .T. ) ;
#73093 = VERTEX_POINT ( 'NONE', #97529 ) ;
#73094 = CARTESIAN_POINT ( 'NONE',  ( -75.62287095715004170, -25.00182538069145366, 7.747789668545099317 ) ) ;
#73095 = CARTESIAN_POINT ( 'NONE',  ( -99.58953762381673869, -23.47593901973091235, -1.443836447539001089 ) ) ;
#73096 = CARTESIAN_POINT ( 'NONE',  ( -3.970774856468506364, -19.35638658347046714, 11.49999999999999645 ) ) ;
#73097 = CARTESIAN_POINT ( 'NONE',  ( -45.62287095715004881, -24.99156045073392463, 7.747789690856161648 ) ) ;
#73098 = CARTESIAN_POINT ( 'NONE',  ( -67.52209883245490118, -23.48783264082477018, -1.443836473390094799 ) ) ;
#73099 = ADVANCED_FACE ( 'NONE', ( #58986 ), #67598, .F. ) ;
#73100 = ORIENTED_EDGE ( 'NONE', *, *, #97538, .T. ) ;
#73101 = CARTESIAN_POINT ( 'NONE',  ( -117.6228709571500417, -24.65952944569305316, 1.056160979905706121 ) ) ;
#73102 = CARTESIAN_POINT ( 'NONE',  ( 9.315600972258346602, 5.965225279485572685, 28.35070303307545458 ) ) ;
#73103 = CARTESIAN_POINT ( 'NONE',  ( -6.741682653110981249, -0.3587747205144265483, 30.62569541381301619 ) ) ;
#73104 = CARTESIAN_POINT ( 'NONE',  ( -21.09935167195790839, -4.734744157926700225, -1.500000000000002220 ) ) ;
#73105 = CARTESIAN_POINT ( 'NONE',  ( 5.105333984060716368, 3.311071866383498374, -27.56005651598365347 ) ) ;
#73106 = CARTESIAN_POINT ( 'NONE',  ( -19.00951991574052968, 3.723548053296564575, -1.500000000000002220 ) ) ;
#73107 = CARTESIAN_POINT ( 'NONE',  ( -10.21991166328316325, -3.845527176268170422, 29.42879868625613327 ) ) ;
#73108 = CARTESIAN_POINT ( 'NONE',  ( -81.17551393562025908, -25.07642019275565204, 7.403513165760432280 ) ) ;
#73109 = CARTESIAN_POINT ( 'NONE',  ( -7.851535696030730982, 18.15458241006858131, 11.49999999999998934 ) ) ;
#73110 = EDGE_CURVE ( 'NONE', #100015, #6511, #86333, .T. ) ;
#73111 = VECTOR ( 'NONE', #66250, 1000.000000000000114 ) ;
#73112 = ORIENTED_EDGE ( 'NONE', *, *, #75476, .T. ) ;
#73113 = CARTESIAN_POINT ( 'NONE',  ( 20.23811035156253979, -1.552196809741442696, 11.49999999999999645 ) ) ;
#73114 = CARTESIAN_POINT ( 'NONE',  ( -7.138063944469604571, -5.876774720514409189, 19.21974929698718881 ) ) ;
#73115 = EDGE_CURVE ( 'NONE', #13904, #27148, #4035, .T. ) ;
#73116 = VERTEX_POINT ( 'NONE', #5183 ) ;
#73117 = CARTESIAN_POINT ( 'NONE',  ( -67.52287095715007581, -23.96177878511310055, 10.65340807706329329 ) ) ;
#73118 = DIRECTION ( 'NONE',  ( 0.000000000000000000, 0.000000000000000000, -1.000000000000000000 ) ) ;
#73119 = LINE ( 'NONE', #80723, #93014 ) ;
#73120 = CARTESIAN_POINT ( 'NONE',  ( -122.6228709571500417, -23.47596703998600631, 11.44779298504227860 ) ) ;
#73121 = DIRECTION ( 'NONE',  ( 1.000000000000000000, 0.000000000000000000, 0.000000000000000000 ) ) ;
#73122 = LINE ( 'NONE', #80221, #23513 ) ;
#73123 = CARTESIAN_POINT ( 'NONE',  ( -1.415466703587968667, 19.98303252902060834, 11.49999999999998934 ) ) ;
#73124 = FACE_OUTER_BOUND ( 'NONE', #67944, .T. ) ;
#73125 = ORIENTED_EDGE ( 'NONE', *, *, #47645, .T. ) ;
#73126 = FACE_OUTER_BOUND ( 'NONE', #87136, .T. ) ;
#73127 = PLANE ( 'NONE',  #33194 ) ;
#73128 = CARTESIAN_POINT ( 'NONE',  ( -80.29320949403980023, -25.30554951654463736, 4.971011992112520872 ) ) ;
#73129 = CARTESIAN_POINT ( 'NONE',  ( -51.62287095715005592, -29.50250786944525672, 11.44777988621624054 ) ) ;
#73130 = CARTESIAN_POINT ( 'NONE',  ( -73.59659251472847075, -23.96119346886880663, -0.6495511937832115779 ) ) ;
#73131 = EDGE_CURVE ( 'NONE', #16349, #59175, #13777, .T. ) ;
#73132 = CYLINDRICAL_SURFACE ( 'NONE', #31596, 3.349999999999998757 ) ;
#73133 = CARTESIAN_POINT ( 'NONE',  ( -50.02720224525958770, -25.12100811749006724, 7.112893600995336740 ) ) ;
#73134 = ORIENTED_EDGE ( 'NONE', *, *, #34939, .T. ) ;
#73135 = EDGE_CURVE ( 'NONE', #33464, #49490, #74307, .T. ) ;
#73136 = CARTESIAN_POINT ( 'NONE',  ( -17.48930418531667996, -10.34094407820366612, 11.49999999999998934 ) ) ;
#73137 = VERTEX_POINT ( 'NONE', #36630 ) ;
#73138 = CARTESIAN_POINT ( 'NONE',  ( -3.987988226355533072, 22.59150145119509290, 11.49999999999998934 ) ) ;
#73139 = CARTESIAN_POINT ( 'NONE',  ( 31.67047468188955150, 5.333900073052421753, 28.72484383265714314 ) ) ;
#73140 = CARTESIAN_POINT ( 'NONE',  ( -127.6238337642146803, -24.35071581493543746, 9.817618358456011052 ) ) ;
#73142 = VERTEX_POINT ( 'NONE', #61481 ) ;
#73141 = EDGE_CURVE ( 'NONE', #98739, #49798, #89925, .T. ) ;
#73143 = CARTESIAN_POINT ( 'NONE',  ( -50.62287095715005592, -29.50249982740957577, 7.747779886224967605 ) ) ;
#73144 = ADVANCED_FACE ( 'NONE', ( #70584 ), #37628, .F. ) ;
#73145 = CARTESIAN_POINT ( 'NONE',  ( -49.31927893949910668, -25.12215271391963611, 6.419594345602365415 ) ) ;
#73146 = CARTESIAN_POINT ( 'NONE',  ( 9.383883476483161346, 17.86611652351680846, 0.000000000000000000 ) ) ;
#73147 = CARTESIAN_POINT ( 'NONE',  ( -17.82860346875387947, 11.52481846644873187, 11.49999999999999645 ) ) ;
#73148 = CARTESIAN_POINT ( 'NONE',  ( 10.50125231818214289, 19.49540335892314502, -1.500000000000002220 ) ) ;
#73149 = VECTOR ( 'NONE', #84563, 1000.000000000000000 ) ;
#73150 = CARTESIAN_POINT ( 'NONE',  ( 9.149160795417088821, -18.46424698110740437, -1.500000000000002220 ) ) ;
#73151 = ORIENTED_EDGE ( 'NONE', *, *, #82188, .F. ) ;
#73152 = CARTESIAN_POINT ( 'NONE',  ( -94.52287095715006160, -23.48786465467242479, 11.44779295918254292 ) ) ;
#73153 = VERTEX_POINT ( 'NONE', #45252 ) ;
#73154 = CARTESIAN_POINT ( 'NONE',  ( -54.54196740513740593, -24.34968618360932879, 0.1864209137778771175 ) ) ;
#73155 = DIRECTION ( 'NONE',  ( -3.773278334453080206E-23, 0.9999999999976377785, 2.173523156925979975E-06 ) ) ;
#73156 = VERTEX_POINT ( 'NONE', #39629 ) ;
#73157 = ORIENTED_EDGE ( 'NONE', *, *, #37780, .F. ) ;
#73158 = ORIENTED_EDGE ( 'NONE', *, *, #92154, .F. ) ;
#73159 = PLANE ( 'NONE',  #64864 ) ;
#73160 = CARTESIAN_POINT ( 'NONE',  ( -81.48149462243461016, -25.24685308744633261, 6.293942982122115559 ) ) ;
#73161 = CARTESIAN_POINT ( 'NONE',  ( 5.344006250707635353, -5.876774720514418071, 20.55781796641452885 ) ) ;
#73162 = CARTESIAN_POINT ( 'NONE',  ( -20.13249939377427111, -5.111880259578561514, -1.500000000000002220 ) ) ;
#73163 = EDGE_CURVE ( 'NONE', #34608, #67104, #78177, .T. ) ;
#73164 = CARTESIAN_POINT ( 'NONE',  ( -6.179238894844691465, -20.81818906610659425, 11.49999999999999645 ) ) ;
#73165 = ORIENTED_EDGE ( 'NONE', *, *, #9626, .T. ) ;
#73166 = CARTESIAN_POINT ( 'NONE',  ( -99.11920994418380815, -25.30018492339840108, 5.369493761298492096 ) ) ;
#73167 = CARTESIAN_POINT ( 'NONE',  ( -111.7095396657709756, -25.25156236136107779, 3.853968145065129747 ) ) ;
#73168 = CARTESIAN_POINT ( 'NONE',  ( 22.28251467978060063, -2.329348454117679879, 11.49999999999998934 ) ) ;
#73169 = DIRECTION ( 'NONE',  ( -3.773278334453079618E-23, 0.9999999999976377785, 2.173523156925979975E-06 ) ) ;
#73170 = FACE_OUTER_BOUND ( 'NONE', #22455, .T. ) ;
#73171 = ORIENTED_EDGE ( 'NONE', *, *, #59050, .T. ) ;
#73172 = LINE ( 'NONE', #34610, #40429 ) ;
#73173 = AXIS2_PLACEMENT_3D ( 'NONE', #16686, #49167, #9078 ) ;
#73174 = CARTESIAN_POINT ( 'NONE',  ( 7.160000000000000142, 8.786681894035815787, 6.233837718258663507 ) ) ;
#73175 = LOCAL_TIME ( 0, 54, 15.00000000000000000, #95179 ) ;
#73176 = ORIENTED_EDGE ( 'NONE', *, *, #98386, .F. ) ;
#73177 = ORIENTED_EDGE ( 'NONE', *, *, #81684, .T. ) ;
#73179 = EDGE_CURVE ( 'NONE', #17861, #41986, #63360, .T. ) ;
#73178 = CARTESIAN_POINT ( 'NONE',  ( -87.62287095715002749, -23.94994826722515668, -0.6494450866351715312 ) ) ;
#73180 = ORIENTED_EDGE ( 'NONE', *, *, #73946, .F. ) ;
#73181 = CARTESIAN_POINT ( 'NONE',  ( -10.79823215447539653, -18.26288818932900071, -1.500000000000002220 ) ) ;
#73182 = ADVANCED_FACE ( 'NONE', ( #38626 ), #14780, .T. ) ;
#73183 = EDGE_LOOP ( 'NONE', ( #6497, #52802, #35112, #96106, #63723, #2104, #58926, #90881, #8031, #8283, #81118, #56807, #95124, #31910, #92387, #72, #33527, #99226, #29457, #41860, #56208, #11513, #2371, #48358, #69439, #12209, #18640, #379, #56347, #85227, #42869, #9493, #19521, #51306, #38190, #95014, #50551, #91178, #82981, #88265, #48172, #92506, #39582, #56278, #24970, #59544, #48500, #25370, #10362, #45832, #20824, #82773, #57191, #60810, #29688, #2251, #5862, #55806, #72533, #75953, #86364, #13093, #90850, #87110, #31875, #22077, #682, #93134, #77936, #65134, #38623, #95744, #73554, #64336, #7381, #36036, #93345, #28871, #49493, #4005, #33694, #94725, #85132, #71646, #92876, #6010, #77686, #76601, #64984, #61388, #54447, #93350, #29506, #94998, #35115, #85510, #44376, #73906, #58951, #55303, #45347, #21360, #37939, #72129, #5417, #78261, #72292, #30461, #46289, #66426, #43633, #32196, #94158, #47221, #87266, #11091, #62792, #66698, #27839, #26449, #87520, #28630, #75997, #30615, #24478, #57197, #25758, #73727, #86461, #64565, #40736, #91872, #75294, #55936, #39744, #48678, #20519, #88998, #11488, #91608, #66245, #34814, #58182, #44076, #19680, #50319, #29687, #41876, #14615, #55563, #97045, #65780, #21181, #65579, #88768, #85936, #7358, #34868, #91922, #63309, #41436, #6870, #77044, #60339, #19150, #39768, #81160, #15236, #72425, #89589, #66684, #87975, #14345, #12536, #30853, #78507, #100241, #2682, #98556, #62405, #34975, #37840, #3430, #605, #50378, #14782, #13884, #92968, #43687, #26100, #71315, #56716, #33038, #48833, #49075, #43700, #55772, #14514, #136, #77676, #61544, #98906 ) ) ;
#73184 = CARTESIAN_POINT ( 'NONE',  ( -88.55825198115908847, -23.73766607897670156, -1.055555164236456678 ) ) ;
#73185 = CARTESIAN_POINT ( 'NONE',  ( 12.52028139621776326, 17.89958603277719718, 11.49999999999998934 ) ) ;
#73186 = CARTESIAN_POINT ( 'NONE',  ( -103.5600759584140889, -23.48786465467241058, 11.44779295918254292 ) ) ;
#73187 = FACE_OUTER_BOUND ( 'NONE', #25411, .T. ) ;
#73188 = CARTESIAN_POINT ( 'NONE',  ( -20.27875734969026311, 6.143225279485574397, 21.75402280011862644 ) ) ;
#73189 = CARTESIAN_POINT ( 'NONE',  ( -18.37190169643047355, -11.86832528159398237, -1.500000000000002220 ) ) ;
#73190 = DIRECTION ( 'NONE',  ( 0.1875268396392987258, 0.000000000000000000, 0.9822594791677485837 ) ) ;
#73191 = ORIENTED_EDGE ( 'NONE', *, *, #8472, .F. ) ;
#73192 = CARTESIAN_POINT ( 'NONE',  ( -24.90875734969025501, -5.965225279485572685, 30.00402280011862288 ) ) ;
#73193 = CARTESIAN_POINT ( 'NONE',  ( -73.52287095715007581, -24.64898659630528854, 1.056161002820824368 ) ) ;
#73194 = EDGE_CURVE ( 'NONE', #4626, #14296, #55228, .T. ) ;
#73195 = EDGE_CURVE ( 'NONE', #68291, #96886, #45745, .T. ) ;
#73196 = B_SPLINE_CURVE_WITH_KNOTS ( 'NONE', 3,
 ( #33890, #35884, #66854, #95786 ),
 .UNSPECIFIED., .F., .F.,
 ( 4, 4 ),
 ( 0.000000000000000000, 9.999999999999592548E-05 ),
 .UNSPECIFIED. ) ;
#73197 = ORIENTED_EDGE ( 'NONE', *, *, #53122, .F. ) ;
#73198 = CARTESIAN_POINT ( 'NONE',  ( -30.58903781818379741, -24.99239904628540643, 7.801777447997523041 ) ) ;
#73199 = EDGE_CURVE ( 'NONE', #88129, #9489, #91406, .T. ) ;
#73200 = ORIENTED_EDGE ( 'NONE', *, *, #52219, .T. ) ;
#73201 = PLANE ( 'NONE',  #40444 ) ;
#73202 = CARTESIAN_POINT ( 'NONE',  ( -30.65075255989291492, -23.47618869255534690, -1.443836447538997314 ) ) ;
#73203 = CARTESIAN_POINT ( 'NONE',  ( -20.86817740539179056, 4.147639786170328691, 11.49999999999998934 ) ) ;
#73204 = DIRECTION ( 'NONE',  ( 0.000000000000000000, 2.173523156925980399E-06, -0.9999999999976378895 ) ) ;
#73205 = FACE_OUTER_BOUND ( 'NONE', #74527, .T. ) ;
#73206 = CARTESIAN_POINT ( 'NONE',  ( -85.58930583537424752, -24.52300882791530157, 0.6510814631126254914 ) ) ;
#73207 = CARTESIAN_POINT ( 'NONE',  ( -24.90875734969025501, -6.376774720514426953, 26.43402280011862615 ) ) ;
#73208 = CARTESIAN_POINT ( 'NONE',  ( -18.32239908988104204, -6.426282940459683068, -1.500000000000002220 ) ) ;
#73209 = AXIS2_PLACEMENT_3D ( 'NONE', #2308, #74305, #20014 ) ;
#73210 = CARTESIAN_POINT ( 'NONE',  ( -117.5170211865436727, -24.51419770103158768, 9.386484678747166299 ) ) ;
#73211 = ORIENTED_EDGE ( 'NONE', *, *, #1770, .F. ) ;
#73212 = CARTESIAN_POINT ( 'NONE',  ( 16.94836550497923966, -9.742303593519430649, 11.49999999999999645 ) ) ;
#73213 = CARTESIAN_POINT ( 'NONE',  ( -5.576690828732316696, -6.376774720514417183, 20.34213149456667935 ) ) ;
#73214 = CARTESIAN_POINT ( 'NONE',  ( -29.58500155169703660, -25.10124537647697451, 6.766630343226909261 ) ) ;
#73215 = ORIENTED_EDGE ( 'NONE', *, *, #19012, .T. ) ;
#73216 = FACE_OUTER_BOUND ( 'NONE', #52060, .T. ) ;
#73217 = CARTESIAN_POINT ( 'NONE',  ( -32.58953762381672448, -23.48786465467240347, 11.44779295918255535 ) ) ;
#73218 = CARTESIAN_POINT ( 'NONE',  ( -80.58953762381673869, -23.47596703998600276, 11.44779298504227683 ) ) ;
#73219 = FACE_OUTER_BOUND ( 'NONE', #95383, .T. ) ;
#73220 = CARTESIAN_POINT ( 'NONE',  ( 16.89532177248590372, -10.13005384644002227, 11.49999999999998934 ) ) ;
#73221 = ORIENTED_EDGE ( 'NONE', *, *, #72702, .T. ) ;
#73222 = VECTOR ( 'NONE', #21301, 1000.000000000000114 ) ;
#73223 = CARTESIAN_POINT ( 'NONE',  ( -94.62287095715004170, -24.33832256527048088, 0.1851278514138620657 ) ) ;
#73224 = CARTESIAN_POINT ( 'NONE',  ( 2.911360383046243783, -5.876774720514418071, 20.24673073119071276 ) ) ;
#73225 = B_SPLINE_CURVE_WITH_KNOTS ( 'NONE', 3,
 ( #40653, #18310, #64518, #77307 ),
 .UNSPECIFIED., .F., .F.,
 ( 4, 4 ),
 ( 2.775557561562891351E-17, 0.0001000000000000167286 ),
 .UNSPECIFIED. ) ;
#73226 = APPROVAL_ROLE ( '' ) ;
#73227 = EDGE_LOOP ( 'NONE', ( #9615, #31227, #50691, #86887 ) ) ;
#73228 = CARTESIAN_POINT ( 'NONE',  ( -4.621320343559618848, 12.50000000000004974, 0.000000000000000000 ) ) ;
#73229 = CARTESIAN_POINT ( 'NONE',  ( 32.40199294184732537, 5.965225279485572685, -12.82361242714782712 ) ) ;
#73230 = CARTESIAN_POINT ( 'NONE',  ( -47.63367723631196071, -24.34968618360933590, 0.1864209137778879144 ) ) ;
#73231 = CARTESIAN_POINT ( 'NONE',  ( -97.55776846943201974, -23.73791477778912196, 11.05961554403170410 ) ) ;
#73232 = CARTESIAN_POINT ( 'NONE',  ( -45.62287095715004881, -29.50250786944525672, 11.44777988621624054 ) ) ;
#73233 = CARTESIAN_POINT ( 'NONE',  ( -69.34303308397305443, -25.24515236888725056, 6.209207408895393243 ) ) ;
#73234 = LINE ( 'NONE', #72738, #52656 ) ;
#73235 = CARTESIAN_POINT ( 'NONE',  ( -17.52048005523606022, -9.576713672051738513, -1.500000000000002220 ) ) ;
#73236 = CARTESIAN_POINT ( 'NONE',  ( -0.07697111846721775563, -22.05354838441670040, 9.879314768251401091 ) ) ;
#73237 = CARTESIAN_POINT ( 'NONE',  ( 15.94990109002195489, -11.90149544800030590, -1.500000000000002220 ) ) ;
#73238 = ORIENTED_EDGE ( 'NONE', *, *, #579, .F. ) ;
#73239 = CARTESIAN_POINT ( 'NONE',  ( -71.52287095715007581, -24.64898659630528854, 1.056161002820824368 ) ) ;
#73240 = VECTOR ( 'NONE', #5462, 1000.000000000000114 ) ;
#73241 = CC_DESIGN_APPROVAL ( #100233, ( #21418 ) ) ;
#73242 = DIRECTION ( 'NONE',  ( 0.000000000000000000, 0.000000000000000000, -1.000000000000000000 ) ) ;
#73243 = CARTESIAN_POINT ( 'NONE',  ( 11.51813299235546673, -6.376774720514426953, -25.01561358505534471 ) ) ;
#73244 = CARTESIAN_POINT ( 'NONE',  ( 16.81283763619640936, 12.23492182941471107, 11.49999999999999645 ) ) ;
#73245 = CARTESIAN_POINT ( 'NONE',  ( -7.586742644780859912, -5.876774720514413630, 19.78730719034165020 ) ) ;
#73246 = CARTESIAN_POINT ( 'NONE',  ( -59.92287095715005307, -23.47593901973090169, -1.443836447538997536 ) ) ;
#73247 = CARTESIAN_POINT ( 'NONE',  ( -15.22011711465338912, -17.00649957279452451, 11.49999999999999645 ) ) ;
#73249 = ADVANCED_FACE ( 'NONE', ( #54869 ), #32018, .F. ) ;
#73248 = VERTEX_POINT ( 'NONE', #84294 ) ;
#73250 = PLANE ( 'NONE',  #85173 ) ;
#73251 = DIRECTION ( 'NONE',  ( 0.000000000000000000, -1.000000000000000000, 0.000000000000000000 ) ) ;
#73252 = ORIENTED_EDGE ( 'NONE', *, *, #67527, .T. ) ;
#73253 = CARTESIAN_POINT ( 'NONE',  ( 15.52975653788041122, 12.98207780544785628, -1.500000000000002220 ) ) ;
#73254 = DIRECTION ( 'NONE',  ( -1.000000000000000000, -3.773278334444166432E-23, -8.201307841325785021E-29 ) ) ;
#73255 = CARTESIAN_POINT ( 'NONE',  ( 9.843544857143434967, 6.475225279485573360, -27.49819965379373343 ) ) ;
#73256 = EDGE_CURVE ( 'NONE', #15801, #91381, #83998, .T. ) ;
#73257 = ADVANCED_FACE ( 'NONE', ( #30008 ), #100002, .T. ) ;
#73258 = CARTESIAN_POINT ( 'NONE',  ( -84.52287095715004739, -24.50216790748206463, 0.6166512839542488411 ) ) ;
#73259 = EDGE_CURVE ( 'NONE', #16731, #95088, #566, .T. ) ;
#73260 = ORIENTED_EDGE ( 'NONE', *, *, #61577, .T. ) ;
#73261 = CARTESIAN_POINT ( 'NONE',  ( -101.9507253916653440, -29.50249654204571215, 6.236241424690079249 ) ) ;
#73262 = CARTESIAN_POINT ( 'NONE',  ( -125.6228709571500843, -25.00158670708909625, 2.256160236439166855 ) ) ;
#73263 = CARTESIAN_POINT ( 'NONE',  ( 3.179702300980958185, 19.78100630842630281, -1.500000000000002220 ) ) ;
#73264 = CARTESIAN_POINT ( 'NONE',  ( -19.58807393344005376, -7.628504261335002923, 11.49999999999999645 ) ) ;
#73265 = EDGE_CURVE ( 'NONE', #3225, #80003, #71444, .T. ) ;
#73266 = DIRECTION ( 'NONE',  ( -1.000000000000000000, 0.000000000000000000, -0.000000000000000000 ) ) ;
#73267 = CARTESIAN_POINT ( 'NONE',  ( -79.52287095715006160, -24.64965694238575011, 8.947790433994198267 ) ) ;
#73268 = CARTESIAN_POINT ( 'NONE',  ( 17.21905055353458991, -13.78536315820828229, -1.500000000000002220 ) ) ;
#73269 = FACE_OUTER_BOUND ( 'NONE', #17814, .T. ) ;
#73270 = VECTOR ( 'NONE', #65731, 1000.000000000000000 ) ;
#73271 = DIRECTION ( 'NONE',  ( 0.000000000000000000, -0.9999999999976377785, -2.173523156925979975E-06 ) ) ;
#73272 = FACE_OUTER_BOUND ( 'NONE', #52035, .T. ) ;
#73273 = CARTESIAN_POINT ( 'NONE',  ( -89.81226385320383088, -25.27880950044345454, 5.947789066509452383 ) ) ;
#73274 = CARTESIAN_POINT ( 'NONE',  ( -31.65060625173388331, -23.96119346886880663, -0.6495511937832003646 ) ) ;
#73275 = EDGE_LOOP ( 'NONE', ( #40696, #66798, #75132, #73514 ) ) ;
#73276 = EDGE_LOOP ( 'NONE', ( #8077, #5212 ) ) ;
#73277 = LINE ( 'NONE', #82864, #55133 ) ;
#73278 = CARTESIAN_POINT ( 'NONE',  ( -61.24303308397303880, -25.03284409833926105, 7.563174216509380265 ) ) ;
#73279 = CARTESIAN_POINT ( 'NONE',  ( -51.52287095715006870, -24.64898659630367206, 1.056161002820821038 ) ) ;
#73280 = CARTESIAN_POINT ( 'NONE',  ( 3.385237411341575964, -20.22741857368478335, -1.500000000000002220 ) ) ;
#73281 = EDGE_CURVE ( 'NONE', #6893, #33865, #8873, .T. ) ;
#73282 = VERTEX_POINT ( 'NONE', #30512 ) ;
#73283 = FACE_OUTER_BOUND ( 'NONE', #41070, .T. ) ;
#73284 = FACE_OUTER_BOUND ( 'NONE', #99944, .T. ) ;
#73285 = CARTESIAN_POINT ( 'NONE',  ( -83.52287095715007581, -24.51283580621365488, 0.6167428607019708187 ) ) ;
#73286 = CARTESIAN_POINT ( 'NONE',  ( -18.97848940637192428, 11.77069306843248064, -1.500000000000002220 ) ) ;
#73287 = CARTESIAN_POINT ( 'NONE',  ( 32.54003107466018463, -4.047905215973556459, -1.500050581001865169 ) ) ;
#73288 = CARTESIAN_POINT ( 'NONE',  ( -124.6228709571500417, -23.96127896941633750, -0.6493128931037770446 ) ) ;
#73289 = ADVANCED_FACE ( 'NONE', ( #25409, #11187, #17803 ), #64509, .F. ) ;
#73290 = ORIENTED_EDGE ( 'NONE', *, *, #18343, .F. ) ;
#73291 = CARTESIAN_POINT ( 'NONE',  ( 33.61456970919605425, -3.316774720514426900, -11.35828564741663449 ) ) ;
#73292 = DIRECTION ( 'NONE',  ( 0.000000000000000000, 0.9999999999976377785, 2.173523156925979128E-06 ) ) ;
#73293 = VECTOR ( 'NONE', #22646, 1000.000000000000000 ) ;
#73294 = CARTESIAN_POINT ( 'NONE',  ( -20.80165436122882383, -1.723964017131293103, -1.500000000000002220 ) ) ;
#73295 = CIRCLE ( 'NONE', #61921, 2.249999999999998668 ) ;
#73296 = EDGE_LOOP ( 'NONE', ( #72758, #79807, #46089, #80857 ) ) ;
#73299 = ORIENTED_EDGE ( 'NONE', *, *, #34657, .F. ) ;
#73298 = ADVANCED_FACE ( 'NONE', ( #25910 ), #87814, .F. ) ;
#73297 = CARTESIAN_POINT ( 'NONE',  ( -39.38343800729271038, -25.18497175702170665, 3.293004123648116455 ) ) ;
#73300 = ORIENTED_EDGE ( 'NONE', *, *, #63293, .F. ) ;
#73301 = CARTESIAN_POINT ( 'NONE',  ( -69.62994293422308090, -25.03149333592383385, 7.382559687064914833 ) ) ;
#73302 = CARTESIAN_POINT ( 'NONE',  ( -0.5131542516139314669, 21.03015271272555253, -1.500000000000002220 ) ) ;
#73303 = ORIENTED_EDGE ( 'NONE', *, *, #55227, .T. ) ;
#73304 = CARTESIAN_POINT ( 'NONE',  ( -7.160000000000000142, 0.1579206558577708475, 5.788828319098143105 ) ) ;
#73305 = LINE ( 'NONE', #74779, #4491 ) ;
#73306 = CARTESIAN_POINT ( 'NONE',  ( -120.5196203229499616, -24.15602025860899360, 10.28564288303534902 ) ) ;
#73307 = CARTESIAN_POINT ( 'NONE',  ( -28.62287095715004881, -23.31954350884483773, -1.443835782653508426 ) ) ;
#73308 = CARTESIAN_POINT ( 'NONE',  ( -49.62091712621314343, -25.14804027490129457, 3.048647684539328662 ) ) ;
#73309 = CARTESIAN_POINT ( 'NONE',  ( -17.90551237062050305, -12.20792721910736667, -1.500000000000002220 ) ) ;
#73310 = LINE ( 'NONE', #18509, #20591 ) ;
#73312 = ORIENTED_EDGE ( 'NONE', *, *, #51159, .F. ) ;
#73311 = CARTESIAN_POINT ( 'NONE',  ( 22.17158117043571863, -1.905908075979310334, 11.49999999999999645 ) ) ;
#73313 = CARTESIAN_POINT ( 'NONE',  ( -51.44586644541745812, -25.31441856498040011, 5.815367604029775705 ) ) ;
#73314 = CARTESIAN_POINT ( 'NONE',  ( 6.963174204274080736, -6.376774720514415407, 20.29202897614545975 ) ) ;
#73315 = CARTESIAN_POINT ( 'NONE',  ( -101.2228709571500644, -23.47593901973090169, -1.443836447538996870 ) ) ;
#73317 = ORIENTED_EDGE ( 'NONE', *, *, #59769, .T. ) ;
#73316 = EDGE_CURVE ( 'NONE', #32133, #80860, #51292, .T. ) ;
#73318 = EDGE_CURVE ( 'NONE', #497, #92630, #11526, .T. ) ;
#73320 = EDGE_LOOP ( 'NONE', ( #47946, #14805, #38784, #73770 ) ) ;
#73319 = CARTESIAN_POINT ( 'NONE',  ( -105.5228709571500758, -23.47596703998600631, 11.44779298504228038 ) ) ;
#73321 = VECTOR ( 'NONE', #13409, 1000.000000000000227 ) ;
#73322 = EDGE_LOOP ( 'NONE', ( #22197, #41615, #23873, #28347 ) ) ;
#73323 = APPROVAL_PERSON_ORGANIZATION ( #97545, #90973, #11811 ) ;
#73324 = DIRECTION ( 'NONE',  ( -3.773278334453079030E-23, 0.9999999999976377785, 2.173523156925979128E-06 ) ) ;
#73325 = FACE_OUTER_BOUND ( 'NONE', #78233, .T. ) ;
#73326 = CARTESIAN_POINT ( 'NONE',  ( -48.62287095715005592, -24.51283580621362646, 0.6167428607019825870 ) ) ;
#73327 = CARTESIAN_POINT ( 'NONE',  ( -32.62287095715004881, -24.65952944569304250, 1.056160979905691688 ) ) ;
#73328 = ORIENTED_EDGE ( 'NONE', *, *, #4696, .F. ) ;
#73329 = CARTESIAN_POINT ( 'NONE',  ( -130.5728709571501156, -23.71408096108764596, -1.258868304936411109 ) ) ;
#73330 = CARTESIAN_POINT ( 'NONE',  ( 22.29217321540274099, 2.676729263222305644, -1.500000000000002220 ) ) ;
#73331 = VECTOR ( 'NONE', #40835, 1000.000000000000000 ) ;
#73332 = ORIENTED_EDGE ( 'NONE', *, *, #71447, .T. ) ;
#73333 = FACE_OUTER_BOUND ( 'NONE', #1435, .T. ) ;
#73334 = CARTESIAN_POINT ( 'NONE',  ( -6.499999999999992895, 3.983606557377048940, 3.319672131147540561 ) ) ;
#73335 = CARTESIAN_POINT ( 'NONE',  ( 5.109298100551870725, 5.356774720514425603, -27.55941679637891895 ) ) ;
#73336 = CARTESIAN_POINT ( 'NONE',  ( -125.5228709571501184, -23.85196035787549462, -0.8779234886354203571 ) ) ;
#73337 = CARTESIAN_POINT ( 'NONE',  ( -97.24911545764794596, -24.57215472537218659, 9.174899246800713115 ) ) ;
#73338 = CARTESIAN_POINT ( 'NONE',  ( -7.889300446747370188, -17.95381117360125955, 11.49999999999998934 ) ) ;
#73339 = B_SPLINE_SURFACE_WITH_KNOTS ( 'NONE', 3, 3, ( 
 ( #60, #22373, #53357, #70069 ),
 ( #85290, #54357, #84285, #61473 ),
 ( #8174, #46742, #38112, #21874 ),
 ( #7164, #13767, #99993, #92396 ),
 ( #77166, #44745, #15777, #37619 ),
 ( #23374, #91897, #29499, #83289 ),
 ( #75666, #31003, #7670, #45735 ) ),
 .UNSPECIFIED., .F., .F., .F.,
 ( 4, 3, 4 ),
 ( 4, 4 ),
 ( 0.7945040050992236980, 0.8970133687736496775, 0.9995227324480755460 ),
 ( 0.2295523296736148022, 0.2306710308168615775 ),
 .UNSPECIFIED. ) ;
#73340 = DIRECTION ( 'NONE',  ( 0.000000000000000000, 1.000000000000000000, 1.478457507934778393E-16 ) ) ;
#73341 = ORIENTED_EDGE ( 'NONE', *, *, #2051, .F. ) ;
#73342 = CARTESIAN_POINT ( 'NONE',  ( -21.46803524902295024, 1.580295693706654347, 11.49999999999998934 ) ) ;
#73343 = CARTESIAN_POINT ( 'NONE',  ( 7.462166178408539352, -5.965225279485572685, -27.67315496249664974 ) ) ;
#73344 = CARTESIAN_POINT ( 'NONE',  ( -71.08634551208074015, -25.25639530652865616, 6.775733508723637222 ) ) ;
#73345 = CARTESIAN_POINT ( 'NONE',  ( -33.62287095715005592, -29.50248528299804818, 1.056150453629029817 ) ) ;
#73346 = CARTESIAN_POINT ( 'NONE',  ( -108.6228709571500701, -23.48783264082478794, -1.443836473390060604 ) ) ;
#73347 = CARTESIAN_POINT ( 'NONE',  ( -1.334576548209915225, -22.92891363262047832, -1.500000000000002220 ) ) ;
#73348 = AXIS2_PLACEMENT_3D ( 'NONE', #54122, #15531, #10934 ) ;
#73349 = DATE_AND_TIME ( #32776, #73175 ) ;
#73350 = CARTESIAN_POINT ( 'NONE',  ( -29.49875734969026198, -0.3587747205144265483, 10.11402280011862587 ) ) ;
#73351 = PLANE ( 'NONE',  #84717 ) ;
#73352 = CARTESIAN_POINT ( 'NONE',  ( 18.81927703376926786, -7.057843677351100631, 11.49999999999999645 ) ) ;
#73353 = CARTESIAN_POINT ( 'NONE',  ( 5.095029512766671154, 3.302735871364486098, -27.56177443937556859 ) ) ;
#73354 = CARTESIAN_POINT ( 'NONE',  ( -32.63551089020518958, -24.35071581493542681, 9.817618358456035921 ) ) ;
#73355 = PRODUCT_DEFINITION_SHAPE ( 'NONE', 'NONE',  #100421 ) ;
#73356 = FACE_OUTER_BOUND ( 'NONE', #81050, .T. ) ;
#73357 = CARTESIAN_POINT ( 'NONE',  ( -65.62287095715005592, -23.84047902841601640, -0.8780736468305807563 ) ) ;
#73358 = DIRECTION ( 'NONE',  ( 0.000000000000000000, 0.000000000000000000, -1.000000000000000000 ) ) ;
#73359 = CARTESIAN_POINT ( 'NONE',  ( -9.893332137849947472, -17.22304987741864579, 11.49999999999998934 ) ) ;
#73360 = CARTESIAN_POINT ( 'NONE',  ( -57.62287095715004881, -29.50248528299804818, 1.056150453629034924 ) ) ;
#73361 = CARTESIAN_POINT ( 'NONE',  ( -14.12090166725071327, 13.77431136191591143, -1.500000000000002220 ) ) ;
#73362 = CARTESIAN_POINT ( 'NONE',  ( 15.99960863614630391, -3.577630190450220571, -27.91116951066582175 ) ) ;
#73363 = COORDINATED_UNIVERSAL_TIME_OFFSET ( 0, 0, .AHEAD. ) ;
#73364 = VECTOR ( 'NONE', #41273, 1000.000000000000000 ) ;
#73365 = UNCERTAINTY_MEASURE_WITH_UNIT (LENGTH_MEASURE( 1.000000000000000082E-05 ), #89951, 'distance_accuracy_value', 'NONE');
#73366 = CARTESIAN_POINT ( 'NONE',  ( 15.30669619680802995, 3.489325088183165224, -28.51986054853846753 ) ) ;
#73367 = FACE_OUTER_BOUND ( 'NONE', #18498, .T. ) ;
#73368 = CARTESIAN_POINT ( 'NONE',  ( 19.39738937107077632, -6.937168198526852514, 11.49999999999999645 ) ) ;
#73369 = DIRECTION ( 'NONE',  ( 0.000000000000000000, -1.000000000000000000, 0.000000000000000000 ) ) ;
#73370 = CARTESIAN_POINT ( 'NONE',  ( -14.08738070862771963, 17.71811851510361535, 11.49999999999999645 ) ) ;
#73371 = EDGE_LOOP ( 'NONE', ( #61089, #74188, #68673, #38596, #24994, #7006 ) ) ;
#73372 = CARTESIAN_POINT ( 'NONE',  ( -69.50411869601543913, -25.12219058395973903, 6.704350939376936047 ) ) ;
#73374 = EDGE_CURVE ( 'NONE', #55933, #92378, #40140, .T. ) ;
#73373 = CARTESIAN_POINT ( 'NONE',  ( -50.38822539166535108, -25.31267346029541088, 4.736250531364077254 ) ) ;
#73375 = ADVANCED_FACE ( 'NONE', ( #62992 ), #34028, .T. ) ;
#73376 = CARTESIAN_POINT ( 'NONE',  ( -26.85174826923451974, -24.61460070623850882, 8.053060507491462516 ) ) ;
#73377 = EDGE_CURVE ( 'NONE', #68707, #40883, #7609, .T. ) ;
#73378 = DIRECTION ( 'NONE',  ( 0.000000000000000000, -0.9999999999976377785, -2.173523156925979552E-06 ) ) ;
#73379 = EDGE_CURVE ( 'NONE', #93213, #35233, #10137, .T. ) ;
#73380 = VERTEX_POINT ( 'NONE', #26415 ) ;
#73381 = B_SPLINE_CURVE_WITH_KNOTS ( 'NONE', 3,
 ( #22628, #59224, #43991, #68331, #91653, #53617, #74923, #21141, #29764, #60730, #22132, #6922, #45996, #5924 ),
 .UNSPECIFIED., .F., .F.,
 ( 4, 2, 2, 2, 2, 2, 4 ),
 ( 0.000000000000000000, 0.0002566272901473193595, 0.0005132545802946387190, 0.001026509160589279390, 0.001539763740883919735, 0.001796391031031241209, 0.002053018321178562682 ),
 .UNSPECIFIED. ) ;
#73382 = ORIENTED_EDGE ( 'NONE', *, *, #13099, .T. ) ;
#73383 = AXIS2_PLACEMENT_3D ( 'NONE', #49275, #56887, #34533 ) ;
#73384 = CARTESIAN_POINT ( 'NONE',  ( -98.52287095715006160, -23.47596703998600631, 11.44779298504228215 ) ) ;
#73385 = CARTESIAN_POINT ( 'NONE',  ( -22.87863416751641310, 0.2071024363326711970, 11.49999999999998934 ) ) ;
#73386 = CARTESIAN_POINT ( 'NONE',  ( -105.5895376238167245, -24.99132157543166954, 2.256160258750668390 ) ) ;
#73387 = CARTESIAN_POINT ( 'NONE',  ( -113.6281207077734479, -23.96169478059713853, 10.65365249895717348 ) ) ;
#73388 = CARTESIAN_POINT ( 'NONE',  ( -32.52287095715006160, -23.48783264083359867, -1.443836473376375329 ) ) ;
#73389 = DIRECTION ( 'NONE',  ( -3.773278334453079618E-23, 0.9999999999976377785, 2.173523156925979975E-06 ) ) ;
#73390 = CARTESIAN_POINT ( 'NONE',  ( -10.06026007034034464, -20.14757889648583244, 11.49999999999999645 ) ) ;
#73391 = VERTEX_POINT ( 'NONE', #87304 ) ;
#73392 = CARTESIAN_POINT ( 'NONE',  ( -89.81226385320383088, -25.23397913219354649, 6.409327625488847602 ) ) ;
#73393 = CARTESIAN_POINT ( 'NONE',  ( 20.57779966680088890, -7.652443150423321683, -1.500000000000002220 ) ) ;
#73394 = CARTESIAN_POINT ( 'NONE',  ( -44.52203580682488848, -23.48786465467240347, 11.44779295918255357 ) ) ;
#73395 = CARTESIAN_POINT ( 'NONE',  ( -29.14051086615235420, -25.21724692324598394, 6.215525031367211461 ) ) ;
#73396 = VECTOR ( 'NONE', #68481, 1000.000000000000000 ) ;
#73397 = ORIENTED_EDGE ( 'NONE', *, *, #74802, .T. ) ;
#73398 = CARTESIAN_POINT ( 'NONE',  ( -63.62287095715007723, -23.47596703998600631, 11.44779298504227683 ) ) ;
#73399 = CARTESIAN_POINT ( 'NONE',  ( -111.6228709571500275, -24.33832256526968862, 0.1851278514119932828 ) ) ;
#73400 = ORIENTED_EDGE ( 'NONE', *, *, #92201, .T. ) ;
#73401 = CARTESIAN_POINT ( 'NONE',  ( -29.52287095715006870, -23.40099448348795264, -1.443836171194820883 ) ) ;
#73402 = CARTESIAN_POINT ( 'NONE',  ( -17.91610926057384034, -10.00117247862695358, 11.49999999999998934 ) ) ;
#73403 = ORIENTED_EDGE ( 'NONE', *, *, #37008, .F. ) ;
#73404 = VERTEX_POINT ( 'NONE', #9179 ) ;
#73405 = VECTOR ( 'NONE', #4410, 1000.000000000000000 ) ;
#73406 = ORIENTED_EDGE ( 'NONE', *, *, #77253, .T. ) ;
#73407 = CARTESIAN_POINT ( 'NONE',  ( -126.5228709571500332, -24.50216790748206108, 0.6166512839542589441 ) ) ;
#73408 = CARTESIAN_POINT ( 'NONE',  ( 14.65057173600216345, 17.85730367728733725, 11.49999999999998934 ) ) ;
#73409 = CARTESIAN_POINT ( 'NONE',  ( -104.6328494754281877, -23.73791477778912196, 11.05961554403170410 ) ) ;
#73410 = CARTESIAN_POINT ( 'NONE',  ( -17.41452279269062586, 10.58001483151439004, -1.500000000000002220 ) ) ;
#73411 = ORIENTED_EDGE ( 'NONE', *, *, #50244, .F. ) ;
#73412 = DIRECTION ( 'NONE',  ( 0.9903949459893286456, -0.09776975748869043414, 0.09776975748869007332 ) ) ;
#73413 = CARTESIAN_POINT ( 'NONE',  ( -88.62287095714999907, -23.96127896941631619, -0.6493128931037803753 ) ) ;
#73414 = CARTESIAN_POINT ( 'NONE',  ( -10.24059822343752479, -5.876774720514426953, -2.394817856121274864E-14 ) ) ;
#73415 = CARTESIAN_POINT ( 'NONE',  ( -57.55620429048338593, -23.48783264082478439, -1.443836473390068376 ) ) ;
#73416 = ORIENTED_EDGE ( 'NONE', *, *, #59058, .F. ) ;
#73417 = DIRECTION ( 'NONE',  ( 0.000000000000000000, 0.000000000000000000, 1.000000000000000000 ) ) ;
#73418 = CARTESIAN_POINT ( 'NONE',  ( -61.64687923781919210, -25.21083105912962452, 3.409327675794633361 ) ) ;
#73419 = ORIENTED_EDGE ( 'NONE', *, *, #52435, .F. ) ;
#73420 = CARTESIAN_POINT ( 'NONE',  ( 5.906898857431191807, -19.90033995357616092, -1.500000000000002220 ) ) ;
#73421 = ORIENTED_EDGE ( 'NONE', *, *, #8996, .F. ) ;
#73423 = ORIENTED_EDGE ( 'NONE', *, *, #34254, .T. ) ;
#73422 = CARTESIAN_POINT ( 'NONE',  ( -101.5221917989304359, -23.48783264082477373, -1.443836473390089248 ) ) ;
#73424 = B_SPLINE_SURFACE_WITH_KNOTS ( 'NONE', 3, 3, ( 
 ( #21551, #53532, #83457, #7326 ),
 ( #84456, #13945, #79341, #64152 ),
 ( #7832, #9835, #23540, #38782 ),
 ( #16437, #39775, #9328, #25053 ),
 ( #40788, #24553, #54518, #77827 ),
 ( #85450, #8837, #86459, #8334 ),
 ( #69743, #85961, #39280, #47405 ) ),
 .UNSPECIFIED., .F., .F., .F.,
 ( 4, 3, 4 ),
 ( 4, 4 ),
 ( 0.0004766839783824127277, 0.1029713700210899280, 0.2054660560637974476 ),
 ( 0.2395549359311070492, 0.2406781906944148730 ),
 .UNSPECIFIED. ) ;
#73425 = B_SPLINE_CURVE_WITH_KNOTS ( 'NONE', 3,
 ( #46234, #29998, #76166, #6665 ),
 .UNSPECIFIED., .F., .F.,
 ( 4, 4 ),
 ( 0.7810577342095665898, 0.7900641654816820125 ),
 .UNSPECIFIED. ) ;
#73426 = CARTESIAN_POINT ( 'NONE',  ( -25.92875734969025814, -3.316774720514426456, 0.7300228001186309656 ) ) ;
#73427 = DIRECTION ( 'NONE',  ( 0.000000000000000000, 0.000000000000000000, -1.000000000000000000 ) ) ;
#73428 = ORIENTED_EDGE ( 'NONE', *, *, #64519, .T. ) ;
#73429 = ORIENTED_EDGE ( 'NONE', *, *, #62735, .T. ) ;
#73430 = DIRECTION ( 'NONE',  ( -3.773278334453080206E-23, 0.9999999999976377785, 2.173523156925979552E-06 ) ) ;
#73431 = CARTESIAN_POINT ( 'NONE',  ( 5.996070682796505125, 3.316774720514426900, -27.41631156547456882 ) ) ;
#73432 = CARTESIAN_POINT ( 'NONE',  ( -70.65140973383547873, -25.24515049886350582, 5.348842177717589408 ) ) ;
#73434 = ORIENTED_EDGE ( 'NONE', *, *, #78181, .F. ) ;
#73433 = CARTESIAN_POINT ( 'NONE',  ( -17.89045161427552699, -12.92718102017995641, 11.49999999999999645 ) ) ;
#73435 = CARTESIAN_POINT ( 'NONE',  ( -103.5172116781898382, -23.96119346886881019, -0.6495511937832079141 ) ) ;
#73436 = AXIS2_PLACEMENT_3D ( 'NONE', #61944, #70044, #93368 ) ;
#73437 = CARTESIAN_POINT ( 'NONE',  ( -21.91535228782390732, -5.629186751109307885, -1.500000000000002220 ) ) ;
#73438 = ADVANCED_FACE ( 'NONE', ( #80199 ), #71093, .T. ) ;
#73440 = ORIENTED_EDGE ( 'NONE', *, *, #61618, .F. ) ;
#73439 = CARTESIAN_POINT ( 'NONE',  ( -99.19451705248940243, -25.30269465406787788, 5.270746443602242870 ) ) ;
#73441 = VECTOR ( 'NONE', #55523, 1000.000000000000114 ) ;
#73442 = VERTEX_POINT ( 'NONE', #32522 ) ;
#73443 = CARTESIAN_POINT ( 'NONE',  ( -88.52287095715009002, -23.73934037231757088, 11.05740245334328442 ) ) ;
#73444 = EDGE_CURVE ( 'NONE', #63576, #75985, #82730, .T. ) ;
#73445 = CARTESIAN_POINT ( 'NONE',  ( -86.55620429048336462, -23.48783264082478084, -1.443836473390063269 ) ) ;
#73446 = VERTEX_POINT ( 'NONE', #73097 ) ;
#73447 = CARTESIAN_POINT ( 'NONE',  ( -7.741094375770895653, -19.69850519626218599, -1.500000000000002220 ) ) ;
#73448 = CARTESIAN_POINT ( 'NONE',  ( -6.905879715866854340, -5.876774720514411854, 19.48240003225459560 ) ) ;
#73449 = CARTESIAN_POINT ( 'NONE',  ( -41.58505200082024089, -25.30574842329748719, 5.038258840064731459 ) ) ;
#73450 = CARTESIAN_POINT ( 'NONE',  ( 6.212073114426278408, 21.40951068830820958, -1.500000000000002220 ) ) ;
#73451 = CARTESIAN_POINT ( 'NONE',  ( -50.34609605362255280, -25.03220906408855484, 7.561522611969397900 ) ) ;
#73452 = ORIENTED_EDGE ( 'NONE', *, *, #70732, .F. ) ;
#73453 = CARTESIAN_POINT ( 'NONE',  ( -112.5228709571500758, -23.73907113217711284, -1.053371485780540739 ) ) ;
#73454 = DIRECTION ( 'NONE',  ( -1.000000000000000000, 0.000000000000000000, 0.000000000000000000 ) ) ;
#73455 = LINE ( 'NONE', #89178, #915 ) ;
#73456 = CARTESIAN_POINT ( 'NONE',  ( 9.543201319291914093E-14, -5.876774720514426953, 18.21871304725679508 ) ) ;
#73457 = VECTOR ( 'NONE', #55387, 1000.000000000000000 ) ;
#73458 = CARTESIAN_POINT ( 'NONE',  ( -6.230579426152004885, -18.48807627814308674, 11.49999999999998934 ) ) ;
#73459 = CARTESIAN_POINT ( 'NONE',  ( 17.68986881342592454, -12.14045624799103962, 11.49999999999998934 ) ) ;
#73460 = CARTESIAN_POINT ( 'NONE',  ( -0.9257915630711897048, -6.376774720514410077, 19.25892998154168012 ) ) ;
#73461 = DIRECTION ( 'NONE',  ( 0.000000000000000000, 0.9999999999976377785, 2.173523156925979128E-06 ) ) ;
#73462 = FACE_OUTER_BOUND ( 'NONE', #26460, .T. ) ;
#73463 = CARTESIAN_POINT ( 'NONE',  ( -16.48365427610503886, -15.78576583860491489, -1.500000000000002220 ) ) ;
#73464 = DIRECTION ( 'NONE',  ( -2.183067293009317184E-16, -0.9999999665734575771, -0.0002585596332611191095 ) ) ;
#73465 = CARTESIAN_POINT ( 'NONE',  ( -102.5550617024446183, -23.96119346886881729, -0.6495511937831880411 ) ) ;
#73466 = LINE ( 'NONE', #13045, #60578 ) ;
#73467 = CARTESIAN_POINT ( 'NONE',  ( 7.348632388941331861, 18.53259892055224611, 11.49999999999999645 ) ) ;
#73468 = CARTESIAN_POINT ( 'NONE',  ( -101.6228709571500275, -23.73934037231757799, 11.05740245334328087 ) ) ;
#73469 = AXIS2_PLACEMENT_3D ( 'NONE', #25903, #74084, #12165 ) ;
#73470 = CARTESIAN_POINT ( 'NONE',  ( -39.48564304424269977, -24.51419770103158413, 9.386484678747189392 ) ) ;
#73471 = CARTESIAN_POINT ( 'NONE',  ( -48.52204688060093929, -23.48783264082477729, -1.443836473390069264 ) ) ;
#73472 = ORIENTED_EDGE ( 'NONE', *, *, #34884, .T. ) ;
#73473 = LINE ( 'NONE', #97306, #13680 ) ;
#73474 = CARTESIAN_POINT ( 'NONE',  ( -33.01384891882022288, -24.87219037988794312, 1.747789950295619787 ) ) ;
#73475 = CARTESIAN_POINT ( 'NONE',  ( 16.47784684176308545, -14.13017478139203220, 11.49999999999998934 ) ) ;
#73476 = CARTESIAN_POINT ( 'NONE',  ( -50.60270360225540998, -25.04428781446249275, 7.557560453701762881 ) ) ;
#73477 = CARTESIAN_POINT ( 'NONE',  ( -10.41718274906430786, -16.55731393670301088, -1.500000000000002220 ) ) ;
#73478 = CARTESIAN_POINT ( 'NONE',  ( -55.59972936617020878, -24.15602025860896518, 10.28564288303535257 ) ) ;
#73479 = DIRECTION ( 'NONE',  ( 3.773278334444167608E-23, -1.000000000000000000, 0.000000000000000000 ) ) ;
#73480 = CARTESIAN_POINT ( 'NONE',  ( -18.82070947631147106, 8.064391923812276985, 11.49999999999999645 ) ) ;
#73481 = CARTESIAN_POINT ( 'NONE',  ( 14.61581670307174008, -6.475225279485573360, -27.35847990810646024 ) ) ;
#73482 = FACE_OUTER_BOUND ( 'NONE', #7793, .T. ) ;
#73483 = VERTEX_POINT ( 'NONE', #3587 ) ;
#73484 = LINE ( 'NONE', #20184, #574 ) ;
#73485 = CARTESIAN_POINT ( 'NONE',  ( -69.52287095715006160, -29.50248528299804818, 1.056150453629036701 ) ) ;
#73487 = EDGE_CURVE ( 'NONE', #24258, #92190, #55879, .T. ) ;
#73486 = CARTESIAN_POINT ( 'NONE',  ( -45.57257061460039438, -23.48786465467240347, 11.44779295918255002 ) ) ;
#73488 = CARTESIAN_POINT ( 'NONE',  ( -109.5537054002563622, -24.15543982623907482, -0.2315651400026587370 ) ) ;
#73489 = VECTOR ( 'NONE', #67088, 1000.000000000000114 ) ;
#73491 = ORIENTED_EDGE ( 'NONE', *, *, #34187, .F. ) ;
#73490 = EDGE_CURVE ( 'NONE', #26321, #87025, #79190, .T. ) ;
#73492 = FACE_OUTER_BOUND ( 'NONE', #75507, .T. ) ;
#73493 = EDGE_CURVE ( 'NONE', #17738, #80017, #72101, .T. ) ;
#73494 = CARTESIAN_POINT ( 'NONE',  ( 22.51966570110743149, 4.691836548664650053, 11.49999999999999645 ) ) ;
#73495 = CARTESIAN_POINT ( 'NONE',  ( 0.6941480231959694658, 22.73124288027050710, 11.49999999999998934 ) ) ;
#73496 = CARTESIAN_POINT ( 'NONE',  ( 4.854822496258163866, -6.376774720514422512, 20.96950945262037891 ) ) ;
#73497 = B_SPLINE_CURVE_WITH_KNOTS ( 'NONE', 3,
 ( #72157, #77730, #31574, #33584 ),
 .UNSPECIFIED., .F., .F.,
 ( 4, 4 ),
 ( 0.000000000000000000, 1.000000000000000000 ),
 .UNSPECIFIED. ) ;
#73498 = VECTOR ( 'NONE', #2387, 1000.000000000000000 ) ;
#73499 = ADVANCED_FACE ( 'NONE', ( #82187 ), #58374, .T. ) ;
#73500 = CARTESIAN_POINT ( 'NONE',  ( 16.30000000000000071, 2.247226876435393361E-15, -18.35000000000000142 ) ) ;
#73501 = CARTESIAN_POINT ( 'NONE',  ( -97.62287095715005592, -23.47593901973091235, -1.443836447539001089 ) ) ;
#73502 = CARTESIAN_POINT ( 'NONE',  ( -54.52287095715006870, -24.65952944569304606, 1.056160979905693686 ) ) ;
#73503 = ADVANCED_FACE ( 'NONE', ( #43143 ), #66989, .F. ) ;
#73504 = CARTESIAN_POINT ( 'NONE',  ( -70.07703791455010389, -25.13739033695690850, 7.077244113302262996 ) ) ;
#73505 = CARTESIAN_POINT ( 'NONE',  ( -12.54888962926113827, 17.92887824059606672, -1.500000000000002220 ) ) ;
#73506 = DIRECTION ( 'NONE',  ( 0.000000000000000000, -1.000000000000000000, -1.020425574104004246E-16 ) ) ;
#73507 = B_SPLINE_CURVE_WITH_KNOTS ( 'NONE', 3,
 ( #95715, #73386, #65790, #65297 ),
 .UNSPECIFIED., .F., .F.,
 ( 4, 4 ),
 ( 0.000000000000000000, 9.999999999997510880E-05 ),
 .UNSPECIFIED. ) ;
#73508 = DIRECTION ( 'NONE',  ( 0.000000000000000000, 0.000000000000000000, -1.000000000000000000 ) ) ;
#73509 = FACE_OUTER_BOUND ( 'NONE', #3053, .T. ) ;
#73510 = DIRECTION ( 'NONE',  ( 0.7071067811865513475, 0.7071067811865435759, 0.000000000000000000 ) ) ;
#73511 = ORIENTED_EDGE ( 'NONE', *, *, #47191, .F. ) ;
#73512 = CARTESIAN_POINT ( 'NONE',  ( 0.5039804632396667206, -20.40334623801319580, 11.49999999999998934 ) ) ;
#73513 = ORIENTED_EDGE ( 'NONE', *, *, #26054, .T. ) ;
#73514 = ORIENTED_EDGE ( 'NONE', *, *, #55984, .F. ) ;
#73515 = ORIENTED_EDGE ( 'NONE', *, *, #77141, .T. ) ;
#73516 = B_SPLINE_CURVE_WITH_KNOTS ( 'NONE', 3,
 ( #56918, #42690, #12207, #89350 ),
 .UNSPECIFIED., .F., .F.,
 ( 4, 4 ),
 ( 2.202873842868165974E-11, 0.001051771062785959547 ),
 .UNSPECIFIED. ) ;
#73518 = EDGE_CURVE ( 'NONE', #78484, #36722, #41604, .T. ) ;
#73517 = VERTEX_POINT ( 'NONE', #75064 ) ;
#73519 = CARTESIAN_POINT ( 'NONE',  ( -9.967090755842360039, -20.75144515299163217, 11.49999999999998934 ) ) ;
#73520 = LINE ( 'NONE', #4010, #63263 ) ;
#73521 = CARTESIAN_POINT ( 'NONE',  ( 0.4983251850863967269, 20.17815531296474418, -1.500000000000002220 ) ) ;
#73522 = ORIENTED_EDGE ( 'NONE', *, *, #50403, .F. ) ;
#73523 = DIRECTION ( 'NONE',  ( -3.773278334453079030E-23, 0.9999999999976377785, 2.173523156925979128E-06 ) ) ;
#73524 = DIRECTION ( 'NONE',  ( 0.000000000000000000, 0.000000000000000000, -1.000000000000000000 ) ) ;
#73525 = CARTESIAN_POINT ( 'NONE',  ( 32.06540688909007741, 6.475225279485573360, -12.44045471929204716 ) ) ;
#73526 = CARTESIAN_POINT ( 'NONE',  ( -53.51455889064216365, -23.73791477778911840, 11.05961554403170766 ) ) ;
#73528 = EDGE_LOOP ( 'NONE', ( #39833, #60232, #73191, #13595 ) ) ;
#73527 = CARTESIAN_POINT ( 'NONE',  ( -15.71168838272081558, 14.50144224353281786, 11.49999999999999645 ) ) ;
#73529 = CARTESIAN_POINT ( 'NONE',  ( 6.480733632922428988, -5.876774720514425177, 21.47849199606610782 ) ) ;
#73530 = ORIENTED_EDGE ( 'NONE', *, *, #53059, .F. ) ;
#73531 = CARTESIAN_POINT ( 'NONE',  ( -13.70410651198969809, -17.55484038775568933, 11.49999999999998934 ) ) ;
#73532 = CARTESIAN_POINT ( 'NONE',  ( 4.906390264955167169, 20.09725327650800608, 11.49999999999998934 ) ) ;
#73534 = ORIENTED_EDGE ( 'NONE', *, *, #8697, .F. ) ;
#73533 = AXIS2_PLACEMENT_3D ( 'NONE', #12413, #28648, #99139 ) ;
#73535 = CARTESIAN_POINT ( 'NONE',  ( 3.362850247043494001, -5.876774720514404748, 18.65880685207958223 ) ) ;
#73536 = ORIENTED_EDGE ( 'NONE', *, *, #65289, .T. ) ;
#73537 = CARTESIAN_POINT ( 'NONE',  ( 29.80070917940689768, 3.316774720514426456, 27.39560796525317343 ) ) ;
#73538 = ORIENTED_EDGE ( 'NONE', *, *, #96787, .F. ) ;
#73539 = VECTOR ( 'NONE', #95792, 1000.000000000000114 ) ;
#73540 = CARTESIAN_POINT ( 'NONE',  ( 10.11589461582716076, -3.316774720514427344, -28.03692668899584106 ) ) ;
#73541 = CARTESIAN_POINT ( 'NONE',  ( -12.80012119340476140, -16.60591428456014640, -1.500000000000002220 ) ) ;
#73543 = EDGE_CURVE ( 'NONE', #57983, #86, #27415, .T. ) ;
#73542 = CARTESIAN_POINT ( 'NONE',  ( -17.33335002049248530, 13.43749923854009509, 11.49999999999999645 ) ) ;
#73544 = CARTESIAN_POINT ( 'NONE',  ( -73.54977362450368616, -24.15620529776628089, 10.23563542870660470 ) ) ;
#73545 = CARTESIAN_POINT ( 'NONE',  ( -10.06026007034034464, -20.14757889648583244, 11.49999999999998934 ) ) ;
#73546 = CARTESIAN_POINT ( 'NONE',  ( 2.313481123293766206, -20.83243486019555135, 11.49999999999998934 ) ) ;
#73547 = CARTESIAN_POINT ( 'NONE',  ( -26.18848782724420232, -24.97067017990783455, 5.990951028626401609 ) ) ;
#73548 = CARTESIAN_POINT ( 'NONE',  ( 5.641025641025643189, -6.376774720514420736, 20.78665865384615330 ) ) ;
#73549 = EDGE_CURVE ( 'NONE', #69058, #81283, #12674, .T. ) ;
#73550 = FACE_OUTER_BOUND ( 'NONE', #75679, .T. ) ;
#73551 = CARTESIAN_POINT ( 'NONE',  ( -68.55620429048340725, -23.47593901973091235, -1.443836447539006196 ) ) ;
#73552 = VERTEX_POINT ( 'NONE', #82685 ) ;
#73553 = ORIENTED_EDGE ( 'NONE', *, *, #39782, .T. ) ;
#73554 = ORIENTED_EDGE ( 'NONE', *, *, #8433, .F. ) ;
#73555 = B_SPLINE_CURVE_WITH_KNOTS ( 'NONE', 3,
 ( #16081, #91700, #23187, #54173 ),
 .UNSPECIFIED., .F., .F.,
 ( 4, 4 ),
 ( 0.3300215848131905494, 0.3390280160853059721 ),
 .UNSPECIFIED. ) ;
#73556 = CARTESIAN_POINT ( 'NONE',  ( -44.52287095715007581, -23.73934037231757088, 11.05740245334329330 ) ) ;
#73557 = VERTEX_POINT ( 'NONE', #96922 ) ;
#73558 = CARTESIAN_POINT ( 'NONE',  ( 17.37860173834871347, 12.56526366372364301, -1.500000000000002220 ) ) ;
#73559 = EDGE_CURVE ( 'NONE', #33217, #25851, #74091, .T. ) ;
#73560 = CARTESIAN_POINT ( 'NONE',  ( -26.09764047488493333, -24.96011088229958830, 5.074688329380741436 ) ) ;
#73561 = ORIENTED_EDGE ( 'NONE', *, *, #61400, .T. ) ;
#73562 = CARTESIAN_POINT ( 'NONE',  ( 20.91448408463407205, 2.778442817847782020, -1.500000000000002220 ) ) ;
#73563 = CARTESIAN_POINT ( 'NONE',  ( -63.52287095715006160, -24.65952944569304606, 1.056160979905695463 ) ) ;
#73564 = CARTESIAN_POINT ( 'NONE',  ( 3.769931535195356620, -6.376774720514429617, 21.83933825178638699 ) ) ;
#73565 = DIRECTION ( 'NONE',  ( -1.000000000000000000, 0.000000000000000000, 0.000000000000000000 ) ) ;
#73566 = CARTESIAN_POINT ( 'NONE',  ( -101.5888365374433278, -24.34968618360934300, 0.1864209137778871650 ) ) ;
#73567 = CARTESIAN_POINT ( 'NONE',  ( -129.5896345871542508, -24.51419770103158058, 9.386484678747178734 ) ) ;
#73568 = CARTESIAN_POINT ( 'NONE',  ( 10.71795340210964120, -19.33932934982082585, -1.500000000000002220 ) ) ;
#73569 = ORIENTED_EDGE ( 'NONE', *, *, #62733, .T. ) ;
#73570 = FACE_OUTER_BOUND ( 'NONE', #41283, .T. ) ;
#73571 = EDGE_CURVE ( 'NONE', #86922, #91581, #28396, .T. ) ;
#73572 = AXIS2_PLACEMENT_3D ( 'NONE', #92449, #60536, #91450 ) ;
#73573 = CARTESIAN_POINT ( 'NONE',  ( -48.52287095715006160, -23.48786465467241769, 11.44779295918255002 ) ) ;
#73574 = CARTESIAN_POINT ( 'NONE',  ( -41.02425807142757463, -25.31624721201647432, 5.449276950507639938 ) ) ;
#73575 = CARTESIAN_POINT ( 'NONE',  ( -62.58330144089487135, -24.51419770103156281, 9.386484678747184063 ) ) ;
#73576 = AXIS2_PLACEMENT_3D ( 'NONE', #80378, #4258, #74748 ) ;
#73577 = CARTESIAN_POINT ( 'NONE',  ( 8.160000000000000142, -10.15233964170348457, 0.003711184059992174607 ) ) ;
#73578 = CARTESIAN_POINT ( 'NONE',  ( -11.21157863559261791, -18.18922556752850994, 11.49999999999998934 ) ) ;
#73579 = CARTESIAN_POINT ( 'NONE',  ( -69.11883240928005989, -25.16874515868137863, 6.888629470625632578 ) ) ;
#73580 = CARTESIAN_POINT ( 'NONE',  ( -49.88568991126719254, -25.30060005375480969, 6.009289253917325269 ) ) ;
#73581 = CARTESIAN_POINT ( 'NONE',  ( -64.50490266001314410, -24.15620529776628445, 10.23563542870660115 ) ) ;
#73582 = PLANE ( 'NONE',  #73469 ) ;
#73583 = CC_DESIGN_PERSON_AND_ORGANIZATION_ASSIGNMENT ( #64901, #89206, ( #14993 ) ) ;
#73584 = CARTESIAN_POINT ( 'NONE',  ( 19.88857169258762170, 10.62688394266798930, -1.500000000000002220 ) ) ;
#73585 = DIRECTION ( 'NONE',  ( -3.773278334453079618E-23, 0.9999999999976377785, 2.173523156925979975E-06 ) ) ;
#73586 = EDGE_LOOP ( 'NONE', ( #72930, #80177, #45835, #63945 ) ) ;
#73587 = CARTESIAN_POINT ( 'NONE',  ( -50.44907891876609796, -25.31399901078718884, 5.199047781166664883 ) ) ;
#73588 = CARTESIAN_POINT ( 'NONE',  ( -47.62287095715004881, -24.64965695001467694, 8.947790433994185832 ) ) ;
#73589 = CARTESIAN_POINT ( 'NONE',  ( -14.27994306655487300, -13.59162091658854798, 11.49999999999999645 ) ) ;
#73590 = CARTESIAN_POINT ( 'NONE',  ( -59.62287095715008434, -24.34917612406837861, 0.1852690917426605965 ) ) ;
#73591 = CARTESIAN_POINT ( 'NONE',  ( -67.59255334188506481, -24.15543982623906771, -0.2315651400026651485 ) ) ;
#73592 = ORIENTED_EDGE ( 'NONE', *, *, #31333, .T. ) ;
#73593 = DIRECTION ( 'NONE',  ( -1.000000000000000000, -0.000000000000000000, -0.000000000000000000 ) ) ;
#73594 = CARTESIAN_POINT ( 'NONE',  ( -29.54861811807234417, -24.60094191855587553, 3.015636009103882298 ) ) ;
#73595 = CARTESIAN_POINT ( 'NONE',  ( -75.52287095715007581, -23.48786465467241769, 11.44779295918254469 ) ) ;
#73596 = CARTESIAN_POINT ( 'NONE',  ( -4.285004571687458963, -21.18589511591401831, 11.49999999999998934 ) ) ;
#73597 = DIRECTION ( 'NONE',  ( 0.000000000000000000, 2.173523156925980399E-06, -0.9999999999976378895 ) ) ;
#73598 = CARTESIAN_POINT ( 'NONE',  ( 3.017506814366913481, 19.14668354085002733, -1.500000000000002220 ) ) ;
#73599 = PLANE ( 'NONE',  #59406 ) ;
#73600 = B_SPLINE_CURVE_WITH_KNOTS ( 'NONE', 3,
 ( #36164, #60012, #67128, #52886, #22407, #83825 ),
 .UNSPECIFIED., .F., .F.,
 ( 4, 2, 4 ),
 ( 0.000000000000000000, 0.001380901958385393315, 0.002761803916770786630 ),
 .UNSPECIFIED. ) ;
#73601 = CARTESIAN_POINT ( 'NONE',  ( -73.52287095715007581, -23.47596703998600631, 11.44779298504228748 ) ) ;
#73602 = CARTESIAN_POINT ( 'NONE',  ( 10.99584971316270732, 16.45119811332560289, 11.49999999999998934 ) ) ;
#73603 = ORIENTED_EDGE ( 'NONE', *, *, #21348, .T. ) ;
#73604 = CARTESIAN_POINT ( 'NONE',  ( 18.19722386731275066, -8.884848157732822216, 11.49999999999999645 ) ) ;
#73605 = CARTESIAN_POINT ( 'NONE',  ( 12.46200043076872888, 4.205547148226783882, -28.02060279727989922 ) ) ;
#73606 = B_SPLINE_CURVE_WITH_KNOTS ( 'NONE', 3,
 ( #88419, #66604, #88919, #97516, #19390, #18891 ),
 .UNSPECIFIED., .F., .F.,
 ( 4, 2, 4 ),
 ( 0.000000000000000000, 0.001380901958385383774, 0.002761803916770767548 ),
 .UNSPECIFIED. ) ;
#73607 = ORIENTED_EDGE ( 'NONE', *, *, #40634, .T. ) ;
#73608 = B_SPLINE_SURFACE_WITH_KNOTS ( 'NONE', 3, 3, ( 
 ( #38423, #30812, #61281, #92204 ),
 ( #16575, #22679, #15577, #100294 ),
 ( #61777, #92696, #77469, #7969 ),
 ( #38922, #866, #85591, #69876 ),
 ( #62276, #359, #31307, #31819 ),
 ( #62788, #86097, #78472, #42447 ),
 ( #49554, #57664, #9474, #18089 ) ),
 .UNSPECIFIED., .F., .F., .F.,
 ( 4, 3, 4 ),
 ( 4, 4 ),
 ( 0.0004766839783815382645, 0.1029713700210893729, 0.2054660560637971978 ),
 ( 0.5596363591768273027, 0.5609072989206914661 ),
 .UNSPECIFIED. ) ;
#73609 = LINE ( 'NONE', #89334, #49136 ) ;
#73610 = DIRECTION ( 'NONE',  ( -3.773278334453080206E-23, 0.9999999999976377785, 2.173523156925979975E-06 ) ) ;
#73611 = CARTESIAN_POINT ( 'NONE',  ( -75.55620429048340725, -23.48783264082478794, -1.443836473390065489 ) ) ;
#73612 = CARTESIAN_POINT ( 'NONE',  ( -62.62287095715004881, -23.48786465467241058, 11.44779295918254824 ) ) ;
#73613 = CARTESIAN_POINT ( 'NONE',  ( -58.58953762381673158, -24.64898659630367916, 1.056161002820381611 ) ) ;
#73615 = ADVANCED_FACE ( 'NONE', ( #66504 ), #36510, .F. ) ;
#73614 = CARTESIAN_POINT ( 'NONE',  ( 15.05167116458888010, 13.23127732593390959, 11.49999999999998934 ) ) ;
#73616 = DIRECTION ( 'NONE',  ( 0.09824042138329590335, -0.9951627101165079203, -3.519298150595267883E-15 ) ) ;
#73617 = ORIENTED_EDGE ( 'NONE', *, *, #48878, .F. ) ;
#73618 = CARTESIAN_POINT ( 'NONE',  ( 27.53860345374808105, 1.477225279485574028, 0.000000000000000000 ) ) ;
#73619 = EDGE_CURVE ( 'NONE', #64351, #94960, #47710, .T. ) ;
#73620 = LINE ( 'NONE', #37049, #96366 ) ;
#73621 = CARTESIAN_POINT ( 'NONE',  ( -100.5895376238167245, -24.99156044556203327, 7.747789690856173195 ) ) ;
#73622 = EDGE_CURVE ( 'NONE', #29598, #12228, #20277, .T. ) ;
#73623 = DIRECTION ( 'NONE',  ( 0.000000000000000000, 0.9999999999976377785, 2.173523156925979128E-06 ) ) ;
#73624 = CARTESIAN_POINT ( 'NONE',  ( -73.63047822457768632, -24.34968618360933590, 0.1864209137778805869 ) ) ;
#73625 = VECTOR ( 'NONE', #79711, 1000.000000000000000 ) ;
#73626 = CARTESIAN_POINT ( 'NONE',  ( 0.000000000000000000, -2.682774720514426559, 0.000000000000000000 ) ) ;
#73627 = CARTESIAN_POINT ( 'NONE',  ( -93.58953762381671027, -24.64898659630367916, 1.056161002820387829 ) ) ;
#73628 = ORIENTED_EDGE ( 'NONE', *, *, #56485, .T. ) ;
#73629 = CARTESIAN_POINT ( 'NONE',  ( -8.236308187080631171, 18.58821751820538637, 11.49999999999998934 ) ) ;
#73630 = ORIENTED_EDGE ( 'NONE', *, *, #11007, .F. ) ;
#73631 = EDGE_CURVE ( 'NONE', #96474, #63904, #14763, .T. ) ;
#73632 = CARTESIAN_POINT ( 'NONE',  ( -9.675568039816649701, -20.77828039667204862, 11.49999999999998934 ) ) ;
#73633 = CARTESIAN_POINT ( 'NONE',  ( -32.65033202046554806, -23.96119346886880663, -0.6495511937831992544 ) ) ;
#73634 = AXIS2_PLACEMENT_3D ( 'NONE', #39455, #95240, #1898 ) ;
#73635 = EDGE_LOOP ( 'NONE', ( #70818, #55207, #92573, #90519 ) ) ;
#73636 = CARTESIAN_POINT ( 'NONE',  ( 33.74607884027702909, -0.3587747205144265483, -4.999864028243830916 ) ) ;
#73637 = CARTESIAN_POINT ( 'NONE',  ( 15.14729487507453243, 3.547625430422813420, -27.26914648819303721 ) ) ;
#73638 = FACE_OUTER_BOUND ( 'NONE', #1521, .T. ) ;
#73639 = CARTESIAN_POINT ( 'NONE',  ( -18.66175431467001999, 10.11895122522205526, 11.49999999999999645 ) ) ;
#73640 = CARTESIAN_POINT ( 'NONE',  ( -20.56814720681451902, 8.302189128749821734, 11.49999999999998934 ) ) ;
#73641 = B_SPLINE_CURVE_WITH_KNOTS ( 'NONE', 3,
 ( #98022, #74210, #13287, #37136 ),
 .UNSPECIFIED., .F., .F.,
 ( 4, 4 ),
 ( 0.6709791297726001025, 0.6799855610447156362 ),
 .UNSPECIFIED. ) ;
#73642 = CARTESIAN_POINT ( 'NONE',  ( 1.511266892140219920, 20.53031905857337591, 11.49999999999998934 ) ) ;
#73643 = ORIENTED_EDGE ( 'NONE', *, *, #46484, .F. ) ;
#73644 = CARTESIAN_POINT ( 'NONE',  ( -41.61684277447768920, -23.48783264082477729, -1.443836473390075925 ) ) ;
#73645 = ORIENTED_EDGE ( 'NONE', *, *, #41534, .T. ) ;
#73646 = CARTESIAN_POINT ( 'NONE',  ( -54.56007898073282547, -23.73766607897669800, -1.055555164236461785 ) ) ;
#73647 = LINE ( 'NONE', #11246, #29123 ) ;
#73648 = EDGE_LOOP ( 'NONE', ( #21660, #85261, #28366, #95418 ) ) ;
#73649 = ORIENTED_EDGE ( 'NONE', *, *, #96289, .F. ) ;
#73650 = VERTEX_POINT ( 'NONE', #81700 ) ;
#73651 = DIRECTION ( 'NONE',  ( 0.8368789961609479633, -1.189760341428526303E-06, 0.5473879298844910313 ) ) ;
#73652 = CARTESIAN_POINT ( 'NONE',  ( -28.57383146581955202, -24.50354187648331816, 8.947790409070465856 ) ) ;
#73653 = CARTESIAN_POINT ( 'NONE',  ( 14.52861783435694676, -3.922795597833769410, -28.30212872328112539 ) ) ;
#73654 = CARTESIAN_POINT ( 'NONE',  ( -9.565632364391108311, -18.43008791299702764, -1.500000000000002220 ) ) ;
#73655 = CARTESIAN_POINT ( 'NONE',  ( 20.36105213711617878, 7.643125777291208678, 11.49999999999999645 ) ) ;
#73656 = ORIENTED_EDGE ( 'NONE', *, *, #91967, .T. ) ;
#73657 = CARTESIAN_POINT ( 'NONE',  ( -113.6228709571500701, -23.73934037231757799, 11.05740245334328264 ) ) ;
#73658 = CARTESIAN_POINT ( 'NONE',  ( -28.52287095715005805, -23.32378116302990279, 11.44779301262222049 ) ) ;
#73659 = CARTESIAN_POINT ( 'NONE',  ( -21.98280116189361877, -4.439423430357301470, 11.49999999999998934 ) ) ;
#73660 = CARTESIAN_POINT ( 'NONE',  ( 5.641025641025643189, -5.876774720514419847, 20.78665865384615330 ) ) ;
#73661 = CARTESIAN_POINT ( 'NONE',  ( 10.75273025779354796, -5.876774720514426953, 23.03521261039436752 ) ) ;
#73663 = ORIENTED_EDGE ( 'NONE', *, *, #86679, .F. ) ;
#73662 = EDGE_CURVE ( 'NONE', #76914, #24236, #35030, .T. ) ;
#73664 = CARTESIAN_POINT ( 'NONE',  ( -98.52287095715007581, -23.72773821059536914, 11.05748984161097503 ) ) ;
#73665 = LINE ( 'NONE', #35611, #74999 ) ;
#73666 = AXIS2_PLACEMENT_3D ( 'NONE', #74944, #83563, #75947 ) ;
#73667 = ORIENTED_EDGE ( 'NONE', *, *, #77957, .F. ) ;
#73668 = VERTEX_POINT ( 'NONE', #12172 ) ;
#73669 = CARTESIAN_POINT ( 'NONE',  ( 12.92500000000000426, 1.999999999999999556, 19.19609335255483984 ) ) ;
#73670 = EDGE_CURVE ( 'NONE', #78496, #21581, #44634, .T. ) ;
#73671 = ORIENTED_EDGE ( 'NONE', *, *, #70695, .T. ) ;
#73672 = CARTESIAN_POINT ( 'NONE',  ( 20.09692647535021948, 7.048664716645152595, -1.500000000000002220 ) ) ;
#73673 = ORIENTED_EDGE ( 'NONE', *, *, #64893, .T. ) ;
#73674 = DIRECTION ( 'NONE',  ( 0.000000000000000000, 0.000000000000000000, -1.000000000000000000 ) ) ;
#73675 = CARTESIAN_POINT ( 'NONE',  ( 21.45948982579844255, -4.128456637845983934, 11.49999999999998934 ) ) ;
#73676 = CARTESIAN_POINT ( 'NONE',  ( -6.660000000000001030, -10.15233964170348457, 0.003711184059992174607 ) ) ;
#73677 = CARTESIAN_POINT ( 'NONE',  ( -10.49914784070103124, -20.09245350529190688, -1.500000000000002220 ) ) ;
#73678 = CARTESIAN_POINT ( 'NONE',  ( -41.30067620550419605, -25.28892508720148413, 3.692502541096877700 ) ) ;
#73679 = CARTESIAN_POINT ( 'NONE',  ( 5.627902640648289712, -5.876774720514414518, 20.02890049923285787 ) ) ;
#73680 = CARTESIAN_POINT ( 'NONE',  ( -8.129759772327192380, 20.32010563749377141, -1.500000000000002220 ) ) ;
#73681 = CARTESIAN_POINT ( 'NONE',  ( -62.52287095715006160, -29.50248528299804818, 1.056150453629034924 ) ) ;
#73682 = VERTEX_POINT ( 'NONE', #21275 ) ;
#73683 = CARTESIAN_POINT ( 'NONE',  ( -39.56136241089613037, -29.50249502162446902, 5.536722193922502200 ) ) ;
#73684 = FACE_OUTER_BOUND ( 'NONE', #30100, .T. ) ;
#73685 = VERTEX_POINT ( 'NONE', #66002 ) ;
#73686 = CARTESIAN_POINT ( 'NONE',  ( 5.271800844963591359, 3.316774720514426456, -28.56638892015329034 ) ) ;
#73687 = ORIENTED_EDGE ( 'NONE', *, *, #93926, .F. ) ;
#73688 = CARTESIAN_POINT ( 'NONE',  ( 13.82660648177921914, 6.475225279485573360, -27.21585177491302332 ) ) ;
#73689 = FACE_OUTER_BOUND ( 'NONE', #8117, .T. ) ;
#73690 = CARTESIAN_POINT ( 'NONE',  ( 4.782327729912362990, -20.71560727227588927, -1.500000000000002220 ) ) ;
#73691 = DIRECTION ( 'NONE',  ( -4.335561085774420994E-16, -0.000000000000000000, 1.000000000000000000 ) ) ;
#73692 = CARTESIAN_POINT ( 'NONE',  ( -26.63407156546748311, -24.97064516063613482, 2.799621320528929314 ) ) ;
#73693 = AXIS2_PLACEMENT_3D ( 'NONE', #61273, #99309, #45045 ) ;
#73694 = EDGE_CURVE ( 'NONE', #40376, #86483, #56163, .T. ) ;
#73695 = CARTESIAN_POINT ( 'NONE',  ( -85.62828706649705168, -24.73486907724918282, 1.287355809206962576 ) ) ;
#73696 = CARTESIAN_POINT ( 'NONE',  ( -68.58388308116877852, -24.51314013834315375, 0.6176544820404133995 ) ) ;
#73697 = CARTESIAN_POINT ( 'NONE',  ( -39.62287095715007723, -24.35013146730202038, 9.818937971375113705 ) ) ;
#73698 = VERTEX_POINT ( 'NONE', #42656 ) ;
#73699 = CARTESIAN_POINT ( 'NONE',  ( 15.26536572251939461, -12.21375333317339695, 11.49999999999999645 ) ) ;
#73700 = CARTESIAN_POINT ( 'NONE',  ( -99.49761415653327390, -25.31438896437989783, 4.819718821452458890 ) ) ;
#73701 = CARTESIAN_POINT ( 'NONE',  ( -27.70544111104076990, -24.64017222881049207, 8.251826729410561612 ) ) ;
#73702 = ORIENTED_EDGE ( 'NONE', *, *, #64051, .T. ) ;
#73703 = AXIS2_PLACEMENT_3D ( 'NONE', #4418, #95757, #97255 ) ;
#73704 = LINE ( 'NONE', #4198, #3708 ) ;
#73705 = EDGE_CURVE ( 'NONE', #43884, #44101, #23647, .T. ) ;
#73706 = CARTESIAN_POINT ( 'NONE',  ( -99.85057463794808541, -25.31439564997497627, 5.344630366307050018 ) ) ;
#73707 = DIRECTION ( 'NONE',  ( 0.000000000000000000, 0.000000000000000000, -1.000000000000000000 ) ) ;
#73708 = CARTESIAN_POINT ( 'NONE',  ( -81.34205133964172774, -25.03156002429774674, 7.294265505898619217 ) ) ;
#73709 = CARTESIAN_POINT ( 'NONE',  ( -11.91260469445801995, 15.66180005371307260, 11.49999999999998934 ) ) ;
#73710 = VERTEX_POINT ( 'NONE', #7930 ) ;
#73711 = DIRECTION ( 'NONE',  ( 0.000000000000000000, 0.000000000000000000, -1.000000000000000000 ) ) ;
#73712 = CARTESIAN_POINT ( 'NONE',  ( -111.5228709571500616, -23.47593901973090524, -1.443836447538996204 ) ) ;
#73713 = PERSON_AND_ORGANIZATION ( #70597, #27821 ) ;
#73714 = VERTEX_POINT ( 'NONE', #32771 ) ;
#73715 = CARTESIAN_POINT ( 'NONE',  ( 30.61643171304413613, -6.475225279485573360, 27.37433008668288181 ) ) ;
#73716 = CARTESIAN_POINT ( 'NONE',  ( -125.9228709571500531, -23.47593901973090169, -1.443836447538996426 ) ) ;
#73717 = CARTESIAN_POINT ( 'NONE',  ( -55.57061825219870599, -23.48783264082475952, -1.443836473390099462 ) ) ;
#73718 = CARTESIAN_POINT ( 'NONE',  ( -118.5181944844509445, -24.34968618360933945, 0.1864209137778906622 ) ) ;
#73719 = CARTESIAN_POINT ( 'NONE',  ( -79.92040109509791534, -25.14083923594767356, 2.947789366383930520 ) ) ;
#73720 = CARTESIAN_POINT ( 'NONE',  ( -69.34374060353803770, -25.31201778562015647, 6.178485698096741530 ) ) ;
#73721 = CARTESIAN_POINT ( 'NONE',  ( -98.62287095715005592, -29.50250243563736774, 8.947779886222138046 ) ) ;
#73723 = EDGE_CURVE ( 'NONE', #39562, #32487, #99613, .T. ) ;
#73722 = CARTESIAN_POINT ( 'NONE',  ( 19.80199147212610811, 2.383747631481649254, 11.49999999999998934 ) ) ;
#73724 = B_SPLINE_CURVE_WITH_KNOTS ( 'NONE', 3,
 ( #88824, #49771, #64513, #3590 ),
 .UNSPECIFIED., .F., .F.,
 ( 4, 4 ),
 ( 0.000000000000000000, 0.001530649038461520672 ),
 .UNSPECIFIED. ) ;
#73725 = CARTESIAN_POINT ( 'NONE',  ( -0.03593141581049384692, -22.58483958596433183, 1.674192380102054178 ) ) ;
#73726 = CARTESIAN_POINT ( 'NONE',  ( 4.721227339208565965, -19.33841413273825793, -1.500000000000002220 ) ) ;
#73727 = ORIENTED_EDGE ( 'NONE', *, *, #42529, .F. ) ;
#73728 = CARTESIAN_POINT ( 'NONE',  ( -29.52287095715006515, -23.38906523657919578, -1.443836447538998424 ) ) ;
#73729 = CARTESIAN_POINT ( 'NONE',  ( -29.52287095715006160, -24.57685061924431835, 8.947790457046968626 ) ) ;
#73730 = TOROIDAL_SURFACE ( 'NONE', #70485, 1.020000000000000018, 2.040000000000000036 ) ;
#73731 = CARTESIAN_POINT ( 'NONE',  ( 9.777643287007670381, -6.376774720514424288, -24.98776412748719977 ) ) ;
#73732 = CARTESIAN_POINT ( 'NONE',  ( -26.33488822642538452, -24.89212854592702584, 6.524121854850513991 ) ) ;
#73733 = CARTESIAN_POINT ( 'NONE',  ( 22.81105451610979173, 6.475225279485573360, -18.46691820600746681 ) ) ;
#73734 = EDGE_CURVE ( 'NONE', #58437, #41257, #22155, .T. ) ;
#73735 = DIRECTION ( 'NONE',  ( -0.000000000000000000, 1.000000000000000000, 1.084202172485504557E-16 ) ) ;
#73736 = ORIENTED_EDGE ( 'NONE', *, *, #22168, .T. ) ;
#73737 = CARTESIAN_POINT ( 'NONE',  ( 2.499999999999994671, 18.99999999999977618, 2.100000000000000089 ) ) ;
#73738 = EDGE_CURVE ( 'NONE', #4330, #44716, #94669, .T. ) ;
#73739 = CARTESIAN_POINT ( 'NONE',  ( -127.5208720400457452, -24.65952944569305316, 1.056160979905707009 ) ) ;
#73740 = ORIENTED_EDGE ( 'NONE', *, *, #28629, .T. ) ;
#73741 = CARTESIAN_POINT ( 'NONE',  ( 18.82617747125253871, -7.458514806974097411, -1.500000000000002220 ) ) ;
#73742 = CARTESIAN_POINT ( 'NONE',  ( 7.176111537430461595, -6.376774720514424288, 21.53668079471899333 ) ) ;
#73743 = EDGE_CURVE ( 'NONE', #75990, #32056, #62237, .T. ) ;
#73744 = CARTESIAN_POINT ( 'NONE',  ( -108.5228709571500758, -23.48783264083353473, -1.443836473376470586 ) ) ;
#73745 = EDGE_CURVE ( 'NONE', #87999, #56219, #79143, .T. ) ;
#73746 = PLANE ( 'NONE',  #89792 ) ;
#73747 = ORIENTED_EDGE ( 'NONE', *, *, #23061, .F. ) ;
#73748 = CARTESIAN_POINT ( 'NONE',  ( -79.88644693265914043, -25.30805915561094466, 4.573105107165710947 ) ) ;
#73749 = CARTESIAN_POINT ( 'NONE',  ( -2.196420576317535289, -5.876774720514409189, 19.14926908420044782 ) ) ;
#73750 = CARTESIAN_POINT ( 'NONE',  ( -19.74138705131307248, -3.616033589355840849, -1.500000000000002220 ) ) ;
#73751 = CARTESIAN_POINT ( 'NONE',  ( -14.96386864383857329, 14.77685607883014640, 11.49999999999999645 ) ) ;
#73752 = CARTESIAN_POINT ( 'NONE',  ( 30.56047832681635867, 2.297196155479663826, 24.67598410064777070 ) ) ;
#73753 = CARTESIAN_POINT ( 'NONE',  ( -70.65050809644763774, -23.85049219812685806, 10.88485053497527311 ) ) ;
#73754 = CARTESIAN_POINT ( 'NONE',  ( 15.76968270297436625, 15.47746201419723100, 11.49999999999998934 ) ) ;
#73755 = VECTOR ( 'NONE', #75107, 1000.000000000000000 ) ;
#73756 = CARTESIAN_POINT ( 'NONE',  ( 8.443068886831737174, 5.148414450533975284, -25.96590744588278454 ) ) ;
#73757 = CARTESIAN_POINT ( 'NONE',  ( -55.55620429048338593, -24.99132157543166244, 2.256160258750668834 ) ) ;
#73758 = DIRECTION ( 'NONE',  ( -0.000000000000000000, -1.000000000000000000, -0.000000000000000000 ) ) ;
#73759 = ORIENTED_EDGE ( 'NONE', *, *, #41919, .T. ) ;
#73760 = CARTESIAN_POINT ( 'NONE',  ( -72.55406320783903595, -23.96119346886880663, -0.6495511937832121330 ) ) ;
#73761 = PLANE ( 'NONE',  #97210 ) ;
#73762 = ORIENTED_EDGE ( 'NONE', *, *, #70192, .F. ) ;
#73763 = ORIENTED_EDGE ( 'NONE', *, *, #46492, .T. ) ;
#73764 = CARTESIAN_POINT ( 'NONE',  ( -63.62287095715004881, -29.50247984919015209, -1.443849546365056913 ) ) ;
#73765 = DIRECTION ( 'NONE',  ( 0.000000000000000000, 0.000000000000000000, -1.000000000000000000 ) ) ;
#73766 = CARTESIAN_POINT ( 'NONE',  ( -76.64820446010540422, -23.48783264082477373, -1.443836473390089026 ) ) ;
#73767 = CARTESIAN_POINT ( 'NONE',  ( 20.22723401096548201, -3.897675682603606084, -1.500000000000002220 ) ) ;
#73768 = AXIS2_PLACEMENT_3D ( 'NONE', #7889, #60205, #91624 ) ;
#73769 = CARTESIAN_POINT ( 'NONE',  ( -5.740839400147730309, 20.75665450205591966, 11.49999999999999645 ) ) ;
#73770 = ORIENTED_EDGE ( 'NONE', *, *, #78568, .F. ) ;
#73771 = DIRECTION ( 'NONE',  ( -1.084136044942898696E-16, -0.000000000000000000, 1.000000000000000000 ) ) ;
#73772 = CARTESIAN_POINT ( 'NONE',  ( 7.139069293134643779, -5.876774720514421624, 20.58118917620081945 ) ) ;
#73773 = FACE_OUTER_BOUND ( 'NONE', #47569, .T. ) ;
#73774 = CARTESIAN_POINT ( 'NONE',  ( 13.23790625878087468, -17.95846084735695314, -1.500000000000002220 ) ) ;
#73775 = VECTOR ( 'NONE', #81004, 1000.000000000000114 ) ;
#73776 = CARTESIAN_POINT ( 'NONE',  ( 29.75286985256398253, -5.302859984505953861, 26.69689370802097272 ) ) ;
#73777 = LINE ( 'NONE', #58563, #51310 ) ;
#73778 = ORIENTED_EDGE ( 'NONE', *, *, #57979, .F. ) ;
#73779 = CARTESIAN_POINT ( 'NONE',  ( -32.62287095715005592, -24.50321055353805022, 9.387540953477529371 ) ) ;
#73780 = DIRECTION ( 'NONE',  ( -0.9952638024365005887, 0.000000000000000000, -0.09721092304694052555 ) ) ;
#73781 = CARTESIAN_POINT ( 'NONE',  ( 19.25983760003161294, 7.974354923662064998, -1.500000000000002220 ) ) ;
#73782 = VERTEX_POINT ( 'NONE', #100253 ) ;
#73784 = ORIENTED_EDGE ( 'NONE', *, *, #52858, .F. ) ;
#73783 = CARTESIAN_POINT ( 'NONE',  ( 15.32643653063178668, -2.682774720514426559, -27.14485409495428314 ) ) ;
#73785 = ORIENTED_EDGE ( 'NONE', *, *, #96407, .F. ) ;
#73786 = EDGE_CURVE ( 'NONE', #98742, #37689, #822, .T. ) ;
#73787 = PLANE ( 'NONE',  #53608 ) ;
#73788 = CARTESIAN_POINT ( 'NONE',  ( 21.06685942672242362, 1.161445541649065882, -1.500000000000002220 ) ) ;
#73789 = EDGE_LOOP ( 'NONE', ( #61066, #14371, #92834, #27850 ) ) ;
#73790 = CARTESIAN_POINT ( 'NONE',  ( -96.52287095715007581, -23.47593901973090524, -1.443836447538996648 ) ) ;
#73791 = CARTESIAN_POINT ( 'NONE',  ( -49.51651934166289237, -25.30545405216991028, 5.068386278593029814 ) ) ;
#73792 = CARTESIAN_POINT ( 'NONE',  ( -120.6279584262366456, -23.85049219812686871, 10.88485053497526778 ) ) ;
#73793 = B_SPLINE_CURVE_WITH_KNOTS ( 'NONE', 3,
 ( #56100, #41877, #70817, #55600, #3325, #62716 ),
 .UNSPECIFIED., .F., .F.,
 ( 4, 2, 4 ),
 ( 0.000000000000000000, 0.001380764517853251419, 0.002761529035706502839 ),
 .UNSPECIFIED. ) ;
#73794 = DIRECTION ( 'NONE',  ( 1.000000000000000000, 0.000000000000000000, 0.000000000000000000 ) ) ;
#73795 = B_SPLINE_CURVE_WITH_KNOTS ( 'NONE', 3,
 ( #99478, #29974, #83265, #53832 ),
 .UNSPECIFIED., .F., .F.,
 ( 4, 4 ),
 ( 0.000000000000000000, 9.999999999998206125E-05 ),
 .UNSPECIFIED. ) ;
#73796 = CARTESIAN_POINT ( 'NONE',  ( -129.6228709571500701, -24.33927499327855415, 9.819080762295811837 ) ) ;
#73797 = CARTESIAN_POINT ( 'NONE',  ( -18.79206335510377102, -10.79472360063173397, -1.500000000000002220 ) ) ;
#73798 = DIRECTION ( 'NONE',  ( -0.000000000000000000, 1.000000000000000000, -0.000000000000000000 ) ) ;
#73800 = ORIENTED_EDGE ( 'NONE', *, *, #67580, .F. ) ;
#73799 = CARTESIAN_POINT ( 'NONE',  ( -20.07822104958740539, -9.643837532803976487, 11.49999999999999645 ) ) ;
#73801 = CARTESIAN_POINT ( 'NONE',  ( -76.62287095715007013, -23.47593901973091235, -1.443836447539004642 ) ) ;
#73802 = CARTESIAN_POINT ( 'NONE',  ( -3.843380766603781584, 14.10245355761374775, 0.000000000000000000 ) ) ;
#73803 = DIRECTION ( 'NONE',  ( 0.000000000000000000, 0.9999999999976377785, 2.173523156925979128E-06 ) ) ;
#73804 = ORIENTED_EDGE ( 'NONE', *, *, #21257, .T. ) ;
#73806 = ORIENTED_EDGE ( 'NONE', *, *, #39555, .F. ) ;
#73805 = CARTESIAN_POINT ( 'NONE',  ( -40.62287095715004881, -24.52232992886363760, 0.6492154411906044809 ) ) ;
#73807 = ORIENTED_EDGE ( 'NONE', *, *, #49730, .T. ) ;
#73808 = VECTOR ( 'NONE', #52904, 1000.000000000000000 ) ;
#73809 = CARTESIAN_POINT ( 'NONE',  ( -100.7114214627874844, -25.13701171212321839, 7.079427678575232363 ) ) ;
#73810 = CARTESIAN_POINT ( 'NONE',  ( 15.99960863614631101, -3.577630190450212577, -27.91116951066581819 ) ) ;
#73811 = EDGE_CURVE ( 'NONE', #4166, #93720, #17318, .T. ) ;
#73812 = CARTESIAN_POINT ( 'NONE',  ( 31.48454476783385658, 4.132774720514426292, -1.134026763942596494 ) ) ;
#73813 = CARTESIAN_POINT ( 'NONE',  ( -38.52287095715009713, -24.33832256527048088, 0.1851278514138572362 ) ) ;
#73814 = ORIENTED_EDGE ( 'NONE', *, *, #25652, .T. ) ;
#73815 = CARTESIAN_POINT ( 'NONE',  ( -130.5728709571500588, -25.24367434374222086, 7.008680551007247850 ) ) ;
#73816 = CARTESIAN_POINT ( 'NONE',  ( 21.09243369641204069, 7.689775423913054908, -1.500000000000002220 ) ) ;
#73817 = EDGE_CURVE ( 'NONE', #35826, #75060, #17043, .T. ) ;
#73818 = VERTEX_POINT ( 'NONE', #77925 ) ;
#73819 = CARTESIAN_POINT ( 'NONE',  ( -100.3502092750176047, -25.04369193928073045, 7.560303740803074213 ) ) ;
#73820 = CARTESIAN_POINT ( 'NONE',  ( -101.5575535147763162, -23.73791477778911840, 11.05961554403170588 ) ) ;
#73821 = CARTESIAN_POINT ( 'NONE',  ( 8.309867465290103894, 5.356774720514426491, -25.05695269341429920 ) ) ;
#73822 = EDGE_CURVE ( 'NONE', #65645, #20807, #30772, .T. ) ;
#73823 = EDGE_CURVE ( 'NONE', #7140, #20070, #14980, .T. ) ;
#73824 = DIRECTION ( 'NONE',  ( 0.000000000000000000, -0.000000000000000000, 1.000000000000000000 ) ) ;
#73825 = EDGE_CURVE ( 'NONE', #53278, #57950, #14783, .T. ) ;
#73826 = CARTESIAN_POINT ( 'NONE',  ( -130.5728709571500588, -24.57215472537219014, 9.174899246800711339 ) ) ;
#73827 = CARTESIAN_POINT ( 'NONE',  ( -9.247272915838292917, -17.29429475886123768, 11.49999999999998934 ) ) ;
#73828 = B_SPLINE_CURVE_WITH_KNOTS ( 'NONE', 3,
 ( #28893, #90796, #13155, #82178 ),
 .UNSPECIFIED., .F., .F.,
 ( 4, 4 ),
 ( 0.000000000000000000, 9.999999999998897304E-05 ),
 .UNSPECIFIED. ) ;
#73829 = DIRECTION ( 'NONE',  ( 0.000000000000000000, -2.173523156925979552E-06, 0.9999999999976378895 ) ) ;
#73831 = ADVANCED_FACE ( 'NONE', ( #24154 ), #9428, .F. ) ;
#73830 = ORIENTED_EDGE ( 'NONE', *, *, #92480, .T. ) ;
#73832 = CARTESIAN_POINT ( 'NONE',  ( 16.61460563260716583, 13.71664681387569118, -1.500000000000002220 ) ) ;
#73833 = CARTESIAN_POINT ( 'NONE',  ( -7.326923076923074873, -6.376774720514427841, 21.75000000000001066 ) ) ;
#73834 = FACE_OUTER_BOUND ( 'NONE', #31198, .T. ) ;
#73835 = DIRECTION ( 'NONE',  ( -0.000000000000000000, 1.000000000000000000, -0.000000000000000000 ) ) ;
#73836 = DIRECTION ( 'NONE',  ( 2.567145104890970367E-18, -0.9999999999976378895, -2.173523156893722419E-06 ) ) ;
#73837 = CARTESIAN_POINT ( 'NONE',  ( 22.26416322464526232, -5.798680748638591176, -1.500000000000002220 ) ) ;
#73838 = AXIS2_PLACEMENT_3D ( 'NONE', #41952, #35332, #90109 ) ;
#73839 = DATE_AND_TIME ( #66753, #71583 ) ;
#73840 = CARTESIAN_POINT ( 'NONE',  ( -107.5228709571500758, -29.50248528299804818, 1.056150453629043584 ) ) ;
#73841 = CARTESIAN_POINT ( 'NONE',  ( -49.58723797677291856, -24.34968618360933590, 0.1864209137778799763 ) ) ;
#73842 = CARTESIAN_POINT ( 'NONE',  ( -7.807601069497579260, -18.53474111305376937, 11.49999999999999645 ) ) ;
#73843 = CARTESIAN_POINT ( 'NONE',  ( -39.62287095715005592, -29.50248528299804818, 1.056150453629031594 ) ) ;
#73844 = CARTESIAN_POINT ( 'NONE',  ( -89.62287095715004170, -24.65952944569305316, 1.056160979905700348 ) ) ;
#73846 = CARTESIAN_POINT ( 'NONE',  ( -20.27875734969026311, -4.543225279485573864, 24.00402280011862288 ) ) ;
#73845 = CIRCLE ( 'NONE', #5746, 91.74549126261076992 ) ;
#73847 = CARTESIAN_POINT ( 'NONE',  ( 11.86515846156731335, 3.316774720514427788, -28.09350142571734921 ) ) ;
#73848 = CARTESIAN_POINT ( 'NONE',  ( 14.73162737928355170, 3.582999323269832725, -27.37940951657878941 ) ) ;
#73849 = ADVANCED_FACE ( 'NONE', ( #92660 ), #23139, .T. ) ;
#73851 = EDGE_CURVE ( 'NONE', #76974, #38439, #90903, .T. ) ;
#73850 = CARTESIAN_POINT ( 'NONE',  ( -18.79335158860655142, 6.462138572525057967, 11.49999999999998934 ) ) ;
#73852 = AXIS2_PLACEMENT_3D ( 'NONE', #76975, #7469, #44048 ) ;
#73853 = CARTESIAN_POINT ( 'NONE',  ( -113.5190820818342132, -23.96119346886881019, -0.6495511937832028071 ) ) ;
#73854 = CARTESIAN_POINT ( 'NONE',  ( 15.33752688427012778, 12.42672799324400934, -1.500000000000002220 ) ) ;
#73855 = VECTOR ( 'NONE', #41803, 1000.000000000000227 ) ;
#73856 = CARTESIAN_POINT ( 'NONE',  ( -90.30662908837275893, -25.33592526241815790, 4.020882415642697438 ) ) ;
#73857 = PERSON_AND_ORGANIZATION_ROLE ( 'classification_officer' ) ;
#73858 = CARTESIAN_POINT ( 'NONE',  ( -0.7827064370038755436, -6.376774720514410077, 19.55912026249540148 ) ) ;
#73859 = CARTESIAN_POINT ( 'NONE',  ( 2.904396343079095111, -6.376774720514415407, 19.95793242748194984 ) ) ;
#73860 = CARTESIAN_POINT ( 'NONE',  ( 14.37238272058661259, 14.81585024043302035, 11.49999999999999645 ) ) ;
#73861 = EDGE_CURVE ( 'NONE', #3020, #31972, #47169, .T. ) ;
#73862 = LINE ( 'NONE', #65284, #49673 ) ;
#73863 = CARTESIAN_POINT ( 'NONE',  ( -1.322449806865925614, 22.60218017400935864, 11.49999999999999645 ) ) ;
#73864 = VERTEX_POINT ( 'NONE', #10942 ) ;
#73865 = CARTESIAN_POINT ( 'NONE',  ( -129.6228709571500133, -23.48783264082478794, -1.443836473390056607 ) ) ;
#73866 = PLANE ( 'NONE',  #53335 ) ;
#73867 = LINE ( 'NONE', #87601, #41916 ) ;
#73868 = EDGE_CURVE ( 'NONE', #16956, #50557, #24480, .T. ) ;
#73869 = FACE_OUTER_BOUND ( 'NONE', #76750, .T. ) ;
#73870 = ORIENTED_EDGE ( 'NONE', *, *, #4350, .F. ) ;
#73871 = ADVANCED_FACE ( 'NONE', ( #19044 ), #49013, .T. ) ;
#73872 = VERTEX_POINT ( 'NONE', #41908 ) ;
#73873 = CARTESIAN_POINT ( 'NONE',  ( -99.31360333396543183, -25.23370691691098600, 6.322973554867211021 ) ) ;
#73874 = CARTESIAN_POINT ( 'NONE',  ( -4.526818761702180893, -22.41603498850323817, 11.49999999999998934 ) ) ;
#73876 = EDGE_CURVE ( 'NONE', #21078, #96665, #87563, .T. ) ;
#73875 = DIRECTION ( 'NONE',  ( 0.000000000000000000, 0.000000000000000000, -1.000000000000000000 ) ) ;
#73877 = CARTESIAN_POINT ( 'NONE',  ( -19.35566633068252074, -9.524217769563914970, -1.500000000000002220 ) ) ;
#73878 = CARTESIAN_POINT ( 'NONE',  ( 15.58962545129235799, -6.475225279485573360, -26.91365498785467025 ) ) ;
#73879 = LINE ( 'NONE', #4869, #46864 ) ;
#73880 = B_SPLINE_CURVE_WITH_KNOTS ( 'NONE', 3,
 ( #57133, #58617, #33776, #65747 ),
 .UNSPECIFIED., .F., .F.,
 ( 4, 4 ),
 ( 0.8894174519954087810, 0.8904181990361742516 ),
 .UNSPECIFIED. ) ;
#73881 = CARTESIAN_POINT ( 'NONE',  ( -1.585881643086899606, 22.48459252949185228, 11.49999999999999645 ) ) ;
#73882 = EDGE_LOOP ( 'NONE', ( #17728, #19996, #184, #87758 ) ) ;
#73883 = CARTESIAN_POINT ( 'NONE',  ( -43.62370908719063323, -24.65952944569304606, 1.056160979905693909 ) ) ;
#73884 = CARTESIAN_POINT ( 'NONE',  ( 0.3405503412851532130, 21.98688381012616233, 11.49999999999998934 ) ) ;
#73885 = CARTESIAN_POINT ( 'NONE',  ( -111.5172671840988983, -24.15543982623907482, -0.2315651400026575712 ) ) ;
#73886 = DIRECTION ( 'NONE',  ( -0.000000000000000000, 2.173523156925979552E-06, -0.9999999999976378895 ) ) ;
#73887 = ORIENTED_EDGE ( 'NONE', *, *, #66769, .T. ) ;
#73888 = EDGE_CURVE ( 'NONE', #60977, #82121, #72863, .T. ) ;
#73889 = CARTESIAN_POINT ( 'NONE',  ( -63.62287095715004881, -24.64965695001468404, 8.947790433994185832 ) ) ;
#73890 = CARTESIAN_POINT ( 'NONE',  ( 13.36367879947601445, -5.876774720514426953, 20.00000000000000355 ) ) ;
#73891 = ORIENTED_EDGE ( 'NONE', *, *, #99137, .F. ) ;
#73892 = CARTESIAN_POINT ( 'NONE',  ( -77.62287095715005592, -24.64898659630367916, 1.056161002820826145 ) ) ;
#73893 = VERTEX_POINT ( 'NONE', #34286 ) ;
#73894 = VERTEX_POINT ( 'NONE', #50503 ) ;
#73895 = ORIENTED_EDGE ( 'NONE', *, *, #55396, .F. ) ;
#73896 = LINE ( 'NONE', #58672, #24262 ) ;
#73897 = DIRECTION ( 'NONE',  ( 0.000000000000000000, 0.000000000000000000, -1.000000000000000000 ) ) ;
#73898 = CARTESIAN_POINT ( 'NONE',  ( -64.52287095715006160, -23.47596703998600631, 11.44779298504228926 ) ) ;
#73899 = CARTESIAN_POINT ( 'NONE',  ( 0.5039804632396667206, -20.40334623801319580, -1.500000000000002220 ) ) ;
#73900 = VERTEX_POINT ( 'NONE', #88569 ) ;
#73901 = CARTESIAN_POINT ( 'NONE',  ( -0.9540731552372990754, -5.876774720514412742, 19.74568812963596542 ) ) ;
#73902 = CARTESIAN_POINT ( 'NONE',  ( -29.58658507105814195, -24.27136956112387267, 9.817618405055078767 ) ) ;
#73903 = AXIS2_PLACEMENT_3D ( 'NONE', #29167, #74836, #43414 ) ;
#73904 = LINE ( 'NONE', #36343, #46490 ) ;
#73905 = CARTESIAN_POINT ( 'NONE',  ( -71.18291627536595456, -25.25855322842343753, 7.291244491205598699 ) ) ;
#73906 = ORIENTED_EDGE ( 'NONE', *, *, #1330, .F. ) ;
#73907 = CARTESIAN_POINT ( 'NONE',  ( -28.10168127693285101, -24.76880867787903284, 2.337527702696277743 ) ) ;
#73908 = CARTESIAN_POINT ( 'NONE',  ( -33.58953762381673158, -24.65952944569304250, 1.056160979905696351 ) ) ;
#73909 = EDGE_LOOP ( 'NONE', ( #42806, #27489, #72167, #24239 ) ) ;
#73910 = CARTESIAN_POINT ( 'NONE',  ( -4.307737697753418082, 20.33289072680551968, 11.49999999999998934 ) ) ;
#73911 = ORIENTED_EDGE ( 'NONE', *, *, #24894, .T. ) ;
#73913 = VERTEX_POINT ( 'NONE', #73346 ) ;
#73912 = PLANE ( 'NONE',  #29637 ) ;
#73914 = VECTOR ( 'NONE', #29199, 1000.000000000000114 ) ;
#73915 = B_SPLINE_CURVE_WITH_KNOTS ( 'NONE', 3,
 ( #77283, #54974, #9280, #14891, #38232, #40245 ),
 .UNSPECIFIED., .F., .F.,
 ( 4, 2, 4 ),
 ( 1.570755371634170283E-05, 0.001396183895866089054, 0.002776660238015836446 ),
 .UNSPECIFIED. ) ;
#73916 = DIRECTION ( 'NONE',  ( -0.000000000000000000, 2.173523156925979552E-06, -0.9999999999976378895 ) ) ;
#73917 = CARTESIAN_POINT ( 'NONE',  ( 22.33191539159815164, 4.132774720514426292, -16.26852658953823649 ) ) ;
#73918 = ORIENTED_EDGE ( 'NONE', *, *, #99643, .T. ) ;
#73919 = EDGE_LOOP ( 'NONE', ( #65472, #13974, #4008, #88420 ) ) ;
#73920 = AXIS2_PLACEMENT_3D ( 'NONE', #54347, #16765, #94396 ) ;
#73921 = B_SPLINE_CURVE_WITH_KNOTS ( 'NONE', 3,
 ( #3787, #65698, #41340, #26110, #73779, #18989 ),
 .UNSPECIFIED., .F., .F.,
 ( 4, 2, 4 ),
 ( 0.000000000000000000, 0.001380901958385381606, 0.002761803916770763211 ),
 .UNSPECIFIED. ) ;
#73922 = LINE ( 'NONE', #59203, #34886 ) ;
#73923 = CARTESIAN_POINT ( 'NONE',  ( -77.62287095715005592, -24.64965695001468404, 8.947790433994182280 ) ) ;
#73924 = AXIS2_PLACEMENT_3D ( 'NONE', #19914, #96546, #18918 ) ;
#73925 = CARTESIAN_POINT ( 'NONE',  ( -101.1944152955115186, -25.17323144036708626, 6.858246026757193192 ) ) ;
#73926 = CARTESIAN_POINT ( 'NONE',  ( -43.56914089629323428, -23.48786465467240347, 11.44779295918255180 ) ) ;
#73928 = ORIENTED_EDGE ( 'NONE', *, *, #58245, .T. ) ;
#73927 = CARTESIAN_POINT ( 'NONE',  ( 10.35204687333978057, 19.51823071965408829, 11.49999999999999645 ) ) ;
#73929 = AXIS2_PLACEMENT_3D ( 'NONE', #45747, #83800, #20897 ) ;
#73930 = PLANE ( 'NONE',  #65115 ) ;
#73931 = CARTESIAN_POINT ( 'NONE',  ( -13.31036990564671818, -18.29084955798148471, -1.500000000000002220 ) ) ;
#73932 = AXIS2_PLACEMENT_3D ( 'NONE', #82597, #44037, #12583 ) ;
#73934 = VERTEX_POINT ( 'NONE', #33778 ) ;
#73933 = CARTESIAN_POINT ( 'NONE',  ( -115.6262966384274620, -24.52399227489127043, 9.353111116836528183 ) ) ;
#73935 = ORIENTED_EDGE ( 'NONE', *, *, #61725, .F. ) ;
#73936 = CARTESIAN_POINT ( 'NONE',  ( -10.21560369921944833, -5.622950887248190810, 29.47514638292475553 ) ) ;
#73937 = B_SPLINE_CURVE_WITH_KNOTS ( 'NONE', 3,
 ( #94942, #88338, #25429, #42677, #24921 ),
 .UNSPECIFIED., .F., .F.,
 ( 4, 1, 4 ),
 ( 0.1431656576382807078, 0.2545924338564266032, 0.2890741368561012825 ),
 .UNSPECIFIED. ) ;
#73938 = EDGE_CURVE ( 'NONE', #42281, #98946, #81459, .T. ) ;
#73939 = CARTESIAN_POINT ( 'NONE',  ( -82.62287095715005592, -29.50247984919015209, -1.443849546365053582 ) ) ;
#73940 = ORIENTED_EDGE ( 'NONE', *, *, #23902, .F. ) ;
#73941 = CARTESIAN_POINT ( 'NONE',  ( -12.03079493616482765, -17.41531974249929249, 11.49999999999998934 ) ) ;
#73942 = EDGE_CURVE ( 'NONE', #25637, #52065, #97433, .T. ) ;
#73943 = CARTESIAN_POINT ( 'NONE',  ( 5.328346181807287252, -5.876774720514418959, 20.81670806933143680 ) ) ;
#73944 = CARTESIAN_POINT ( 'NONE',  ( -80.62287095715007013, -24.63345952396257488, 9.038047939301510070 ) ) ;
#73945 = CARTESIAN_POINT ( 'NONE',  ( 19.83320176327591255, -10.20924650237717835, -1.500000000000002220 ) ) ;
#73946 = EDGE_CURVE ( 'NONE', #68625, #30205, #65258, .T. ) ;
#73947 = CARTESIAN_POINT ( 'NONE',  ( 29.73828978136053891, -4.772774720514425972, -4.021765098496577373 ) ) ;
#73948 = EDGE_CURVE ( 'NONE', #52488, #6180, #89563, .T. ) ;
#73949 = ORIENTED_EDGE ( 'NONE', *, *, #300, .F. ) ;
#73950 = DIRECTION ( 'NONE',  ( 0.000000000000000000, -1.408054769461694189E-16, 1.000000000000000000 ) ) ;
#73951 = PLANE ( 'NONE',  #89724 ) ;
#73952 = ADVANCED_FACE ( 'NONE', ( #80953 ), #42416, .T. ) ;
#73953 = EDGE_CURVE ( 'NONE', #74213, #55518, #10432, .T. ) ;
#73954 = DIRECTION ( 'NONE',  ( 0.000000000000000000, 0.000000000000000000, 1.000000000000000000 ) ) ;
#73955 = CARTESIAN_POINT ( 'NONE',  ( -83.52287095715006160, -24.64965694238407323, 8.947790433994198267 ) ) ;
#73956 = CARTESIAN_POINT ( 'NONE',  ( 1.133552453683672745, -19.47370032599940615, 11.49999999999998934 ) ) ;
#73957 = CARTESIAN_POINT ( 'NONE',  ( 15.63241172484657682, -14.69700884395465934, 11.49999999999998934 ) ) ;
#73958 = CARTESIAN_POINT ( 'NONE',  ( -26.06135888742384665, -24.57999700124051756, 2.563275948977453922 ) ) ;
#73959 = CARTESIAN_POINT ( 'NONE',  ( -107.6228709571500701, -23.48786465467241769, 11.44779295918253936 ) ) ;
#73960 = CARTESIAN_POINT ( 'NONE',  ( -77.55022051755103973, -24.15543982623907482, -0.2315651400026658147 ) ) ;
#73961 = CARTESIAN_POINT ( 'NONE',  ( 17.57702471007113232, 14.52005670271990034, -1.500000000000002220 ) ) ;
#73962 = PERSON_AND_ORGANIZATION ( #70597, #27821 ) ;
#73963 = CARTESIAN_POINT ( 'NONE',  ( -106.5947057434380554, -23.73791477778912551, 11.05961554403169878 ) ) ;
#73964 = CARTESIAN_POINT ( 'NONE',  ( -8.160000000000000142, -10.65233964170348635, -1.621096496867198589 ) ) ;
#73965 = CARTESIAN_POINT ( 'NONE',  ( -16.62890364678930410, -10.96057169749504645, 11.49999999999999645 ) ) ;
#73966 = CARTESIAN_POINT ( 'NONE',  ( -104.5154284841441950, -24.15543982623907482, -0.2315651400026580709 ) ) ;
#73967 = CARTESIAN_POINT ( 'NONE',  ( 8.971512145086503409, -2.028487854913501032, 5.500000000000000000 ) ) ;
#73968 = CARTESIAN_POINT ( 'NONE',  ( -128.5895376238167103, -24.66019654487200086, 8.947790411086117501 ) ) ;
#73969 = ORIENTED_EDGE ( 'NONE', *, *, #52786, .T. ) ;
#73970 = CARTESIAN_POINT ( 'NONE',  ( -118.6228709571500701, -23.47596703998600631, 11.44779298504227683 ) ) ;
#73971 = EDGE_CURVE ( 'NONE', #13108, #70610, #95177, .T. ) ;
#73972 = CARTESIAN_POINT ( 'NONE',  ( -31.80983992280592787, -25.31516574674648368, 3.894478520810415567 ) ) ;
#73973 = CARTESIAN_POINT ( 'NONE',  ( -9.282276271697774916, -19.63344595494797673, -1.500000000000002220 ) ) ;
#73974 = CARTESIAN_POINT ( 'NONE',  ( -10.16634758543296613, -6.475225279485573360, 30.00402280011862288 ) ) ;
#73975 = CARTESIAN_POINT ( 'NONE',  ( -5.499840656826012975, 18.73951620154120334, -1.500000000000002220 ) ) ;
#73976 = VECTOR ( 'NONE', #97666, 1000.000000000000000 ) ;
#73977 = CARTESIAN_POINT ( 'NONE',  ( -55.64835622778738156, -24.15602025860896518, 10.28564288303535257 ) ) ;
#73978 = B_SPLINE_CURVE_WITH_KNOTS ( 'NONE', 3,
 ( #43750, #36133, #59980, #67103 ),
 .UNSPECIFIED., .F., .F.,
 ( 4, 4 ),
 ( 0.000000000000000000, 9.999999999998897304E-05 ),
 .UNSPECIFIED. ) ;
#73979 = EDGE_CURVE ( 'NONE', #27949, #38058, #27670, .T. ) ;
#73980 = VERTEX_POINT ( 'NONE', #42900 ) ;
#73981 = APPROVAL_DATE_TIME ( #91926, #93371 ) ;
#73982 = CARTESIAN_POINT ( 'NONE',  ( 0.02224039135773677595, -0.3828044741864776723, -0.3828044741864797262 ) ) ;
#73983 = CARTESIAN_POINT ( 'NONE',  ( 2.691128592823461840, 20.25793168094256202, 11.49999999999999645 ) ) ;
#73984 = CARTESIAN_POINT ( 'NONE',  ( -9.150000000000000355, -5.876774720514426953, -15.69999999999999929 ) ) ;
#73985 = AXIS2_PLACEMENT_3D ( 'NONE', #50294, #89840, #73623 ) ;
#73986 = PLANE ( 'NONE',  #44802 ) ;
#73987 = EDGE_LOOP ( 'NONE', ( #91998, #18592, #33708, #87116 ) ) ;
#73988 = DIRECTION ( 'NONE',  ( 0.000000000000000000, -0.9999999999976377785, -2.173523156925979128E-06 ) ) ;
#73989 = CARTESIAN_POINT ( 'NONE',  ( 1.305682803664691249, -5.965225279485572685, 29.57950906855421991 ) ) ;
#73990 = AXIS2_PLACEMENT_3D ( 'NONE', #28445, #96971, #81746 ) ;
#73991 = CARTESIAN_POINT ( 'NONE',  ( 31.52236416363829363, -4.132774720514426292, -3.023391441407382807 ) ) ;
#73992 = VECTOR ( 'NONE', #2781, 1000.000000000000000 ) ;
#73993 = B_SPLINE_CURVE_WITH_KNOTS ( 'NONE', 3,
 ( #17623, #24723, #40468, #1908 ),
 .UNSPECIFIED., .F., .F.,
 ( 4, 4 ),
 ( 0.000000000000000000, 9.999999999999592548E-05 ),
 .UNSPECIFIED. ) ;
#73994 = DIRECTION ( 'NONE',  ( -3.773278334453079618E-23, 0.9999999999976377785, 2.173523156925978705E-06 ) ) ;
#73995 = VERTEX_POINT ( 'NONE', #4335 ) ;
#73996 = DIRECTION ( 'NONE',  ( 0.000000000000000000, -1.000000000000000000, 0.000000000000000000 ) ) ;
#73997 = VECTOR ( 'NONE', #99175, 1000.000000000000114 ) ;
#73998 = EDGE_CURVE ( 'NONE', #27719, #74013, #57135, .T. ) ;
#73999 = CARTESIAN_POINT ( 'NONE',  ( 9.898807498884217182, 20.75630955806377287, 11.49999999999999645 ) ) ;
#74000 = CARTESIAN_POINT ( 'NONE',  ( -20.37646751746074969, -10.17465561509698979, -1.500000000000002220 ) ) ;
#74001 = CARTESIAN_POINT ( 'NONE',  ( -110.5858253176389212, -25.00182538069147498, 7.747789668545046027 ) ) ;
#74002 = CARTESIAN_POINT ( 'NONE',  ( 3.750000000000001776, 26.59999999999999432, 0.000000000000000000 ) ) ;
#74003 = LINE ( 'NONE', #59784, #88951 ) ;
#74004 = CARTESIAN_POINT ( 'NONE',  ( -49.62287095715005592, -24.64898659630528499, 1.056161002820821038 ) ) ;
#74005 = CARTESIAN_POINT ( 'NONE',  ( -54.52287095715006870, -23.48786465467240347, 11.44779295918255002 ) ) ;
#74006 = EDGE_CURVE ( 'NONE', #18475, #96754, #49516, .T. ) ;
#74007 = CARTESIAN_POINT ( 'NONE',  ( -21.73523922981167189, -2.474665994198115726, -1.500000000000002220 ) ) ;
#74008 = CARTESIAN_POINT ( 'NONE',  ( 29.73860345376319358, -1.477225279485574028, -8.849814207987163783 ) ) ;
#74009 = PLANE ( 'NONE',  #43637 ) ;
#74010 = CARTESIAN_POINT ( 'NONE',  ( 13.91401389203221406, 5.356774720514425603, 158.0376437107427137 ) ) ;
#74011 = ORIENTED_EDGE ( 'NONE', *, *, #22848, .F. ) ;
#74012 = CARTESIAN_POINT ( 'NONE',  ( -15.93830457579706739, -12.76012858937699335, 11.49999999999998934 ) ) ;
#74013 = VERTEX_POINT ( 'NONE', #74823 ) ;
#74014 = ORIENTED_EDGE ( 'NONE', *, *, #4027, .T. ) ;
#74015 = ORIENTED_EDGE ( 'NONE', *, *, #29498, .F. ) ;
#74016 = ORIENTED_EDGE ( 'NONE', *, *, #70596, .T. ) ;
#74017 = CARTESIAN_POINT ( 'NONE',  ( 22.18053613645642841, 6.281410551025238043, -1.500000000000002220 ) ) ;
#74018 = CARTESIAN_POINT ( 'NONE',  ( -80.52287095715006160, -23.85196035786901092, -0.8779234886475191235 ) ) ;
#74019 = CARTESIAN_POINT ( 'NONE',  ( -8.513533612778267923, 18.29693335657625042, -1.500000000000002220 ) ) ;
#74020 = EDGE_LOOP ( 'NONE', ( #79001, #55411, #55031, #67170 ) ) ;
#74021 = AXIS2_PLACEMENT_3D ( 'NONE', #37213, #68164, #67679 ) ;
#74022 = CARTESIAN_POINT ( 'NONE',  ( -98.62287095715007013, -23.47596703998600631, 11.44779298504227860 ) ) ;
#74023 = CARTESIAN_POINT ( 'NONE',  ( -40.94688081444584782, -25.03284417894045788, 7.563176522466704910 ) ) ;
#74024 = LINE ( 'NONE', #26847, #64154 ) ;
#74025 = DIRECTION ( 'NONE',  ( -0.000000000000000000, -0.000000000000000000, -1.000000000000000000 ) ) ;
#74027 = ORIENTED_EDGE ( 'NONE', *, *, #9163, .T. ) ;
#74026 = CARTESIAN_POINT ( 'NONE',  ( 18.17913347391500523, 11.28257676469832660, 11.49999999999999645 ) ) ;
#74028 = LINE ( 'NONE', #4523, #1475 ) ;
#74029 = VERTEX_POINT ( 'NONE', #66751 ) ;
#74030 = CIRCLE ( 'NONE', #12451, 0.3000000000000016542 ) ;
#74031 = CARTESIAN_POINT ( 'NONE',  ( -13.70410651198969809, -17.55484038775568933, -1.500000000000002220 ) ) ;
#74032 = B_SPLINE_CURVE_WITH_KNOTS ( 'NONE', 3,
 ( #30843, #9005, #47584, #39958 ),
 .UNSPECIFIED., .F., .F.,
 ( 4, 4 ),
 ( 0.000000000000000000, 0.0001000000000000167422 ),
 .UNSPECIFIED. ) ;
#74033 = CARTESIAN_POINT ( 'NONE',  ( 20.68991284688621946, 0.5745778482356619365, -1.500000000000002220 ) ) ;
#74034 = VERTEX_POINT ( 'NONE', #6318 ) ;
#74035 = FACE_OUTER_BOUND ( 'NONE', #73320, .T. ) ;
#74036 = ORIENTED_EDGE ( 'NONE', *, *, #94187, .T. ) ;
#74037 = CARTESIAN_POINT ( 'NONE',  ( -56.52287095715007581, -23.72747288104470087, -1.053458166803226570 ) ) ;
#74038 = ORIENTED_EDGE ( 'NONE', *, *, #47858, .T. ) ;
#74039 = CARTESIAN_POINT ( 'NONE',  ( 11.80640562518893866, 6.475225279485576024, -27.06722565682295567 ) ) ;
#74040 = CARTESIAN_POINT ( 'NONE',  ( 2.438461900574103502, 20.79476225230834174, -1.500000000000002220 ) ) ;
#74041 = CARTESIAN_POINT ( 'NONE',  ( -16.30586240431254197, 14.59307310709210626, 11.49999999999999645 ) ) ;
#74042 = CARTESIAN_POINT ( 'NONE',  ( -37.53288840155523332, -24.51419770103156637, 9.386484678747175181 ) ) ;
#74043 = CARTESIAN_POINT ( 'NONE',  ( 9.939345090160914609, -20.19931669485651682, -1.500000000000002220 ) ) ;
#74044 = AXIS2_PLACEMENT_3D ( 'NONE', #94779, #26274, #3454 ) ;
#74045 = CARTESIAN_POINT ( 'NONE',  ( 13.96602909953038640, 15.60522523583095200, -1.500000000000002220 ) ) ;
#74046 = CARTESIAN_POINT ( 'NONE',  ( -26.09636659181000695, -24.97066789626643413, 4.940287549524292388 ) ) ;
#74047 = CARTESIAN_POINT ( 'NONE',  ( 5.697397333356354565, -6.376774720514418959, 20.51730809691671809 ) ) ;
#74048 = CARTESIAN_POINT ( 'NONE',  ( -119.6264748175326105, -23.96169478059714564, 10.65365249895717170 ) ) ;
#74049 = CARTESIAN_POINT ( 'NONE',  ( 0.000000000000000000, -1.473225279485573802, 4.300000000000000711 ) ) ;
#74050 = ORIENTED_EDGE ( 'NONE', *, *, #96031, .T. ) ;
#74051 = VERTEX_POINT ( 'NONE', #13420 ) ;
#74052 = EDGE_LOOP ( 'NONE', ( #50714, #10341, #9902, #79334 ) ) ;
#74053 = CARTESIAN_POINT ( 'NONE',  ( -91.52287095715006160, -29.50250243563736774, 8.947779886222139822 ) ) ;
#74054 = ORIENTED_EDGE ( 'NONE', *, *, #69521, .T. ) ;
#74055 = AXIS2_PLACEMENT_3D ( 'NONE', #64174, #2760, #2259 ) ;
#74056 = CARTESIAN_POINT ( 'NONE',  ( 5.910897418159350103, -20.63055655796343757, -1.500000000000002220 ) ) ;
#74057 = ADVANCED_FACE ( 'NONE', ( #35781 ), #30480, .T. ) ;
#74058 = CARTESIAN_POINT ( 'NONE',  ( -51.93149462243455616, -25.25905089634592571, 6.174051128686508072 ) ) ;
#74060 = VERTEX_POINT ( 'NONE', #6810 ) ;
#74059 = VECTOR ( 'NONE', #54094, 1000.000000000000000 ) ;
#74061 = CARTESIAN_POINT ( 'NONE',  ( 19.97611676871187569, -6.800378171449690257, -1.500000000000002220 ) ) ;
#74062 = CARTESIAN_POINT ( 'NONE',  ( -87.52287095715006160, -24.64898659630528854, 1.056161002820827921 ) ) ;
#74063 = EDGE_CURVE ( 'NONE', #43385, #99855, #74336, .T. ) ;
#74064 = CARTESIAN_POINT ( 'NONE',  ( 2.598243466966731585, -6.376774720514413630, 20.31174627870924709 ) ) ;
#74065 = CARTESIAN_POINT ( 'NONE',  ( -97.52287095715006160, -23.47596703998600631, 11.44779298504228215 ) ) ;
#74066 = AXIS2_PLACEMENT_3D ( 'NONE', #78515, #56216, #87145 ) ;
#74067 = CARTESIAN_POINT ( 'NONE',  ( 12.99736557111424595, 3.316774720514426900, -27.13536621820933448 ) ) ;
#74068 = CARTESIAN_POINT ( 'NONE',  ( -100.5562042904833788, -24.99132157543166599, 2.256160258750667058 ) ) ;
#74069 = CARTESIAN_POINT ( 'NONE',  ( 20.57361055066190758, -8.084994430987380909, -1.500000000000002220 ) ) ;
#74070 = CARTESIAN_POINT ( 'NONE',  ( -116.5158267652437729, -24.65952944569305316, 1.056160979905712338 ) ) ;
#74071 = ADVANCED_FACE ( 'NONE', ( #76310 ), #82932, .F. ) ;
#74072 = CARTESIAN_POINT ( 'NONE',  ( -2.606012662418322634, -6.376774720514410077, 19.21974929698718881 ) ) ;
#74073 = CARTESIAN_POINT ( 'NONE',  ( -40.89894032811586300, -25.31624730604892903, 5.492539635573550960 ) ) ;
#74074 = B_SPLINE_CURVE_WITH_KNOTS ( 'NONE', 3,
 ( #9448, #96197, #25168, #72864, #71863, #26176, #72363, #24662 ),
 .UNSPECIFIED., .F., .F.,
 ( 4, 2, 2, 4 ),
 ( -0.001224554619866345846, -0.0002241820295893650998, 0.0007761905606876156466, 0.002776935741241582344 ),
 .UNSPECIFIED. ) ;
#74075 = EDGE_CURVE ( 'NONE', #55313, #76664, #59125, .T. ) ;
#74076 = CARTESIAN_POINT ( 'NONE',  ( -62.54342312881265542, -24.35071581493542681, 9.817618358456032368 ) ) ;
#74077 = EDGE_CURVE ( 'NONE', #92630, #62167, #61117, .T. ) ;
#74078 = LINE ( 'NONE', #4571, #27085 ) ;
#74079 = CARTESIAN_POINT ( 'NONE',  ( 16.79701800048795590, -13.18750964578662455, 11.49999999999998934 ) ) ;
#74080 = DIRECTION ( 'NONE',  ( -0.7512896232465891000, -0.000000000000000000, -0.6599726524652351767 ) ) ;
#74081 = EDGE_CURVE ( 'NONE', #40482, #67931, #21032, .T. ) ;
#74082 = CARTESIAN_POINT ( 'NONE',  ( -48.86261576302199217, -25.03707831087709579, 7.590867751134624974 ) ) ;
#74083 = DIRECTION ( 'NONE',  ( 0.000000000000000000, -0.9999999999976377785, -2.173523156925979128E-06 ) ) ;
#74084 = DIRECTION ( 'NONE',  ( 1.000000000000000000, 3.773278334444167608E-23, 8.201307833595939069E-29 ) ) ;
#74085 = CARTESIAN_POINT ( 'NONE',  ( 14.05383982582471170, -17.77673030755399708, -1.500000000000002220 ) ) ;
#74086 = PLANE ( 'NONE',  #49095 ) ;
#74087 = ORIENTED_EDGE ( 'NONE', *, *, #93811, .T. ) ;
#74088 = CARTESIAN_POINT ( 'NONE',  ( -50.37830952628071657, -25.31401921878212136, 5.197788989978542773 ) ) ;
#74089 = CARTESIAN_POINT ( 'NONE',  ( -79.51272270944330955, -23.96119346886880308, -0.6495511937832122440 ) ) ;
#74090 = CARTESIAN_POINT ( 'NONE',  ( 7.891737972721761807, -18.10977644326358771, 11.49999999999999645 ) ) ;
#74091 = LINE ( 'NONE', #97902, #48841 ) ;
#74092 = CARTESIAN_POINT ( 'NONE',  ( -73.52287095715007581, -23.72773821059537269, 11.05748984161097503 ) ) ;
#74093 = ORIENTED_EDGE ( 'NONE', *, *, #37159, .T. ) ;
#74094 = DIRECTION ( 'NONE',  ( -3.773278334453079030E-23, 0.9999999999976377785, 2.173523156925979128E-06 ) ) ;
#74095 = DIRECTION ( 'NONE',  ( -0.000000000000000000, -1.000000000000000000, -0.000000000000000000 ) ) ;
#74096 = CARTESIAN_POINT ( 'NONE',  ( -101.0369185477202336, -25.17353314354872396, 6.965963161511662172 ) ) ;
#74097 = CARTESIAN_POINT ( 'NONE',  ( -9.004746288917990782, -19.65190454534591069, 11.49999999999998934 ) ) ;
#74098 = AXIS2_PLACEMENT_3D ( 'NONE', #70041, #527, #9644 ) ;
#74099 = CARTESIAN_POINT ( 'NONE',  ( -70.62287095715005592, -29.50249982740957577, 7.747779886224967605 ) ) ;
#74100 = CARTESIAN_POINT ( 'NONE',  ( -81.42380231474228935, -25.30401792888237011, 5.197789011716578145 ) ) ;
#74101 = CARTESIAN_POINT ( 'NONE',  ( -45.62287095715004881, -29.50250243563736774, 8.947779886222146928 ) ) ;
#74102 = CARTESIAN_POINT ( 'NONE',  ( 14.45944668481935658, 13.51102189132778442, -1.500000000000002220 ) ) ;
#74103 = VERTEX_POINT ( 'NONE', #5816 ) ;
#74104 = VECTOR ( 'NONE', #4325, 1000.000000000000114 ) ;
#74105 = CARTESIAN_POINT ( 'NONE',  ( 16.58868386459195676, 11.68684615565071283, 11.49999999999999645 ) ) ;
#74106 = FACE_OUTER_BOUND ( 'NONE', #20924, .T. ) ;
#74107 = CARTESIAN_POINT ( 'NONE',  ( -44.52287095715004739, -24.51283580621364777, 0.6167428607019598275 ) ) ;
#74108 = ORIENTED_EDGE ( 'NONE', *, *, #17399, .F. ) ;
#74109 = CARTESIAN_POINT ( 'NONE',  ( -20.27875734969026311, -6.376774720514428729, 24.00402280011862288 ) ) ;
#74110 = DIRECTION ( 'NONE',  ( 0.000000000000000000, -0.000000000000000000, -1.000000000000000000 ) ) ;
#74111 = DIRECTION ( 'NONE',  ( 3.773278334444167608E-23, -1.000000000000000000, 0.000000000000000000 ) ) ;
#74112 = CARTESIAN_POINT ( 'NONE',  ( -95.62287095715007013, -24.92579138211020151, 1.929029949965665569 ) ) ;
#74113 = CARTESIAN_POINT ( 'NONE',  ( -10.34999999999997833, 22.00000000000000000, 2.100000000000000089 ) ) ;
#74114 = CARTESIAN_POINT ( 'NONE',  ( 7.329891291799937925, -18.66831812819665970, -1.500000000000002220 ) ) ;
#74115 = CARTESIAN_POINT ( 'NONE',  ( -67.55620429048337883, -23.48783264082478084, -1.443836473390066377 ) ) ;
#74116 = ORIENTED_EDGE ( 'NONE', *, *, #46680, .F. ) ;
#74117 = AXIS2_PLACEMENT_3D ( 'NONE', #28393, #37512, #44134 ) ;
#74118 = CARTESIAN_POINT ( 'NONE',  ( 0.7734273019049007214, 3.892732205269316292, -1.700000000000009059 ) ) ;
#74119 = CARTESIAN_POINT ( 'NONE',  ( -127.5228709571500616, -24.64898659630368627, 1.056161002820834804 ) ) ;
#74120 = DIRECTION ( 'NONE',  ( -0.000000000000000000, 1.000000000000000000, -0.000000000000000000 ) ) ;
#74121 = LINE ( 'NONE', #65041, #22101 ) ;
#74122 = EDGE_CURVE ( 'NONE', #36349, #36077, #36775, .T. ) ;
#74123 = AXIS2_PLACEMENT_3D ( 'NONE', #97734, #29720, #5881 ) ;
#74124 = FACE_OUTER_BOUND ( 'NONE', #50182, .T. ) ;
#74125 = EDGE_CURVE ( 'NONE', #74478, #49573, #86147, .T. ) ;
#74126 = CARTESIAN_POINT ( 'NONE',  ( -100.9401440129433070, -25.03707831087709934, 7.590867751134624086 ) ) ;
#74127 = ORIENTED_EDGE ( 'NONE', *, *, #92946, .F. ) ;
#74128 = CIRCLE ( 'NONE', #67619, 28.96799999999999287 ) ;
#74129 = CARTESIAN_POINT ( 'NONE',  ( -18.18203184671642703, 9.085611141607108365, -1.500000000000002220 ) ) ;
#74130 = ORIENTED_EDGE ( 'NONE', *, *, #10133, .T. ) ;
#74131 = CARTESIAN_POINT ( 'NONE',  ( -20.38739128398232836, 10.50225141308550292, -1.500000000000002220 ) ) ;
#74132 = CARTESIAN_POINT ( 'NONE',  ( 29.61860529676591369, 5.187414344753652706, 28.58826086137218780 ) ) ;
#74133 = ORIENTED_EDGE ( 'NONE', *, *, #4195, .F. ) ;
#74134 = CARTESIAN_POINT ( 'NONE',  ( 29.80070917940689412, -5.965225279485572685, 27.39560796525321607 ) ) ;
#74135 = CARTESIAN_POINT ( 'NONE',  ( -76.52287095715007581, -23.47593901973090169, -1.443836447538996648 ) ) ;
#74136 = CARTESIAN_POINT ( 'NONE',  ( -117.6228709571500559, -23.48786465467241769, 11.44779295918253759 ) ) ;
#74137 = CARTESIAN_POINT ( 'NONE',  ( -4.771770383141621608, -20.67029057396967318, 11.49999999999999645 ) ) ;
#74138 = B_SPLINE_CURVE_WITH_KNOTS ( 'NONE', 3,
 ( #35712, #27603, #50436, #81879 ),
 .UNSPECIFIED., .F., .F.,
 ( 4, 4 ),
 ( 0.8711220469307209280, 0.8801284782028364617 ),
 .UNSPECIFIED. ) ;
#74139 = ORIENTED_EDGE ( 'NONE', *, *, #35818, .T. ) ;
#74140 = CARTESIAN_POINT ( 'NONE',  ( -12.04397493737346991, 18.63154960201688226, -1.500000000000002220 ) ) ;
#74142 = EDGE_CURVE ( 'NONE', #30481, #48655, #15915, .T. ) ;
#74141 = CARTESIAN_POINT ( 'NONE',  ( 20.46650637700042097, -2.330123182410055893, -1.500000000000002220 ) ) ;
#74143 = EDGE_LOOP ( 'NONE', ( #4021, #87113, #22215, #42467 ) ) ;
#74144 = ORIENTED_EDGE ( 'NONE', *, *, #96911, .F. ) ;
#74145 = CARTESIAN_POINT ( 'NONE',  ( 10.86264265030973952, 5.965225279485574461, -28.64597719988137570 ) ) ;
#74146 = CARTESIAN_POINT ( 'NONE',  ( -50.52287095715006160, -24.62285846331433703, 9.038163153548369522 ) ) ;
#74147 = ORIENTED_EDGE ( 'NONE', *, *, #59749, .F. ) ;
#74148 = ORIENTED_EDGE ( 'NONE', *, *, #7730, .T. ) ;
#74149 = ORIENTED_EDGE ( 'NONE', *, *, #8120, .T. ) ;
#74150 = FACE_OUTER_BOUND ( 'NONE', #74162, .T. ) ;
#74151 = CARTESIAN_POINT ( 'NONE',  ( -28.64431595215229720, -24.00349382954137667, 10.23563545308467049 ) ) ;
#74152 = FACE_OUTER_BOUND ( 'NONE', #26108, .T. ) ;
#74153 = CARTESIAN_POINT ( 'NONE',  ( -13.51810693421681719, -15.76408947421354156, -1.500000000000002220 ) ) ;
#74154 = CARTESIAN_POINT ( 'NONE',  ( 14.84582651547613352, 15.88809324551894520, 11.49999999999999645 ) ) ;
#74155 = ORIENTED_EDGE ( 'NONE', *, *, #88448, .T. ) ;
#74156 = CARTESIAN_POINT ( 'NONE',  ( -37.62287095715005592, -24.66019654487199020, 8.947790411086135265 ) ) ;
#74157 = AXIS2_PLACEMENT_3D ( 'NONE', #17000, #95134, #9390 ) ;
#74158 = CARTESIAN_POINT ( 'NONE',  ( 10.34999999999999254, 4.999999999999998224, 2.100000000000000089 ) ) ;
#74159 = CARTESIAN_POINT ( 'NONE',  ( -19.78178409256797465, 10.57734301857266246, -1.500000000000002220 ) ) ;
#74160 = CARTESIAN_POINT ( 'NONE',  ( 0.6000000000000007550, 2.681976490132703452E-15, -21.89999999999999858 ) ) ;
#74161 = CARTESIAN_POINT ( 'NONE',  ( -102.5228709571500758, -23.48786465467241769, 11.44779295918254114 ) ) ;
#74162 = EDGE_LOOP ( 'NONE', ( #89396, #83878, #93655, #51599 ) ) ;
#74163 = CARTESIAN_POINT ( 'NONE',  ( -48.52287095715006160, -29.50250243563736774, 8.947779886222146928 ) ) ;
#74164 = CARTESIAN_POINT ( 'NONE',  ( -116.4728709571500502, -25.21113200442380275, 5.000950865234348619 ) ) ;
#74165 = B_SPLINE_SURFACE_WITH_KNOTS ( 'NONE', 3, 3, ( 
 ( #100340, #79023, #39474, #63840 ),
 ( #9020, #24242, #17128, #17635 ),
 ( #78012, #911, #39970, #32866 ),
 ( #94252, #31865, #69422, #48097 ),
 ( #54710, #1921, #38966, #8017 ),
 ( #9521, #30856, #94753, #47598 ),
 ( #55216, #77517, #70934, #62834 ) ),
 .UNSPECIFIED., .F., .F., .F.,
 ( 4, 3, 4 ),
 ( 4, 4 ),
 ( 0.7945040050992251413, 0.8970133687736510097, 0.9995227324480769893 ),
 ( 0.8797175456623916867, 0.8811364062137666542 ),
 .UNSPECIFIED. ) ;
#74166 = ORIENTED_EDGE ( 'NONE', *, *, #20583, .F. ) ;
#74167 = VERTEX_POINT ( 'NONE', #78803 ) ;
#74168 = CARTESIAN_POINT ( 'NONE',  ( -46.49380392490311920, -24.35071581493542325, 9.817618358456032368 ) ) ;
#74169 = ORIENTED_EDGE ( 'NONE', *, *, #85648, .T. ) ;
#74170 = CARTESIAN_POINT ( 'NONE',  ( -19.37389216307569129, 8.798533688548827669, -1.500000000000002220 ) ) ;
#74171 = VERTEX_POINT ( 'NONE', #8314 ) ;
#74172 = CARTESIAN_POINT ( 'NONE',  ( -88.54557060015829961, -24.51314013834315375, 0.6176544820404129554 ) ) ;
#74173 = PRODUCT_DEFINITION_SHAPE ( 'NONE', 'NONE',  #100431 ) ;
#74174 = CARTESIAN_POINT ( 'NONE',  ( 16.27406392464308027, 14.57352745747340172, -1.500000000000002220 ) ) ;
#74175 = CARTESIAN_POINT ( 'NONE',  ( 1.175186991919855872, 6.376774720514426953, 28.89597625626659649 ) ) ;
#74176 = CARTESIAN_POINT ( 'NONE',  ( -12.60694655700363143, 18.86142483545513926, 11.49999999999998934 ) ) ;
#74177 = CARTESIAN_POINT ( 'NONE',  ( -40.45829750704998418, -25.18430871329344711, 3.293943118056679165 ) ) ;
#74178 = LINE ( 'NONE', #4674, #33595 ) ;
#74179 = CARTESIAN_POINT ( 'NONE',  ( 20.11839708684271244, 8.774209887332036217, -1.500000000000002220 ) ) ;
#74180 = LINE ( 'NONE', #73681, #90069 ) ;
#74181 = VERTEX_POINT ( 'NONE', #84933 ) ;
#74182 = B_SPLINE_CURVE_WITH_KNOTS ( 'NONE', 3,
 ( #15096, #22191, #30316, #46062, #85605, #373, #46554, #61292, #45064, #69388 ),
 .UNSPECIFIED., .F., .F.,
 ( 4, 2, 2, 2, 4 ),
 ( 8.673617379884035472E-19, 0.0002559089097569039288, 0.0005118178195138069903, 0.0007677267292707100517, 0.001023635639027613113 ),
 .UNSPECIFIED. ) ;
#74183 = CARTESIAN_POINT ( 'NONE',  ( -122.5201542580532248, -24.15620529776629510, 10.23563542870659582 ) ) ;
#74184 = CARTESIAN_POINT ( 'NONE',  ( -49.00533630786537032, -25.26337435419707589, 6.749865916534812271 ) ) ;
#74185 = ADVANCED_FACE ( 'NONE', ( #61624 ), #93534, .F. ) ;
#74186 = VECTOR ( 'NONE', #93402, 1000.000000000000114 ) ;
#74188 = ORIENTED_EDGE ( 'NONE', *, *, #9511, .T. ) ;
#74187 = EDGE_CURVE ( 'NONE', #34234, #83477, #57245, .T. ) ;
#74189 = DIRECTION ( 'NONE',  ( 0.000000000000000000, -0.000000000000000000, -1.000000000000000000 ) ) ;
#74190 = EDGE_CURVE ( 'NONE', #45914, #77609, #81211, .T. ) ;
#74191 = CARTESIAN_POINT ( 'NONE',  ( -97.52287095715006160, -29.50250243563736774, 8.947779886222138046 ) ) ;
#74192 = CARTESIAN_POINT ( 'NONE',  ( -30.60533150986764284, -24.66488071993808617, 1.095224832288503203 ) ) ;
#74193 = CARTESIAN_POINT ( 'NONE',  ( 10.81949470224598997, -18.29866561848832518, 11.49999999999998934 ) ) ;
#74194 = CARTESIAN_POINT ( 'NONE',  ( -112.5540321080100057, -24.15543982623908192, -0.2315651400026420004 ) ) ;
#74195 = EDGE_CURVE ( 'NONE', #44951, #80766, #78312, .T. ) ;
#74196 = PLANE ( 'NONE',  #99743 ) ;
#74197 = CARTESIAN_POINT ( 'NONE',  ( 15.92621150404962016, 6.475225279485573360, -27.29681269571043245 ) ) ;
#74198 = CIRCLE ( 'NONE', #53130, 19.00000000000000000 ) ;
#74199 = CARTESIAN_POINT ( 'NONE',  ( -68.58782206624864841, -24.34968618360933590, 0.1864209137778813363 ) ) ;
#74200 = CARTESIAN_POINT ( 'NONE',  ( -32.52287095715004739, -23.47593901973090169, -1.443836447538997092 ) ) ;
#74201 = ORIENTED_EDGE ( 'NONE', *, *, #38775, .T. ) ;
#74202 = CARTESIAN_POINT ( 'NONE',  ( 7.829539893445508270, 17.95258299782629408, 11.49999999999999645 ) ) ;
#74203 = CARTESIAN_POINT ( 'NONE',  ( -43.52287095715007581, -23.47593901973090169, -1.443836447538997092 ) ) ;
#74204 = AXIS2_PLACEMENT_3D ( 'NONE', #84501, #14984, #45462 ) ;
#74205 = CARTESIAN_POINT ( 'NONE',  ( -28.34266632056247204, -24.71873428796616068, 8.144582237604435448 ) ) ;
#74206 = ADVANCED_FACE ( 'NONE', ( #39755 ), #47385, .T. ) ;
#74207 = VERTEX_POINT ( 'NONE', #46376 ) ;
#74208 = DIRECTION ( 'NONE',  ( 1.000000000000000000, 0.000000000000000000, 0.000000000000000000 ) ) ;
#74209 = LINE ( 'NONE', #12789, #40124 ) ;
#74210 = CARTESIAN_POINT ( 'NONE',  ( -63.22287095715005734, -23.47596703998600631, 11.44779298504227683 ) ) ;
#74211 = CARTESIAN_POINT ( 'NONE',  ( -62.52287095715006160, -23.48783264082477018, -1.443836473390091912 ) ) ;
#74212 = CARTESIAN_POINT ( 'NONE',  ( -0.7274468246531539117, 19.66889477801398911, 11.49999999999998934 ) ) ;
#74213 = VERTEX_POINT ( 'NONE', #86438 ) ;
#74214 = CARTESIAN_POINT ( 'NONE',  ( 10.48383480065558615, 3.481296116130239149, -27.02502823977714286 ) ) ;
#74215 = CARTESIAN_POINT ( 'NONE',  ( -71.30457154551152144, -25.24554880456021522, 6.209207408033732278 ) ) ;
#74216 = MECHANICAL_CONTEXT ( 'NONE', #89372, 'mechanical' ) ;
#74217 = EDGE_LOOP ( 'NONE', ( #67370, #78173, #19869, #61850 ) ) ;
#74218 = CARTESIAN_POINT ( 'NONE',  ( -74.52287095715007581, -23.73907113216989728, -1.053371485793254569 ) ) ;
#74219 = CARTESIAN_POINT ( 'NONE',  ( 6.365284455128204399, -6.376774720514413630, 19.73076923076922640 ) ) ;
#74220 = CARTESIAN_POINT ( 'NONE',  ( -47.56045512770388228, -23.73766607897670866, -1.055555164236438692 ) ) ;
#74221 = CARTESIAN_POINT ( 'NONE',  ( 32.76434349455507089, -3.489637856041424957, -3.883594654058048157 ) ) ;
#74222 = FACE_OUTER_BOUND ( 'NONE', #77979, .T. ) ;
#74223 = DIRECTION ( 'NONE',  ( 0.000000000000000000, -1.000000000000000000, 0.000000000000000000 ) ) ;
#74224 = DIRECTION ( 'NONE',  ( -3.773278334453079618E-23, 0.9999999999976377785, 2.173523156925979975E-06 ) ) ;
#74225 = CARTESIAN_POINT ( 'NONE',  ( 13.74685606122050885, 14.44317598224977672, -1.500000000000002220 ) ) ;
#74226 = CARTESIAN_POINT ( 'NONE',  ( -71.62287095715005592, -23.47593901973091235, -1.443836447539006196 ) ) ;
#74227 = DIRECTION ( 'NONE',  ( 0.000000000000000000, 0.000000000000000000, -1.000000000000000000 ) ) ;
#74228 = ORIENTED_EDGE ( 'NONE', *, *, #37654, .F. ) ;
#74229 = PLANE ( 'NONE',  #78291 ) ;
#74230 = EDGE_CURVE ( 'NONE', #39979, #23609, #43920, .T. ) ;
#74231 = CARTESIAN_POINT ( 'NONE',  ( 9.146648804565860047, -6.376774720514257311, -28.07004961687618660 ) ) ;
#74232 = CARTESIAN_POINT ( 'NONE',  ( -124.5120777840107138, -25.30063217623697014, 5.394079605411008060 ) ) ;
#74233 = DIRECTION ( 'NONE',  ( 0.000000000000000000, 0.000000000000000000, 1.000000000000000000 ) ) ;
#74234 = EDGE_CURVE ( 'NONE', #75345, #17858, #30653, .T. ) ;
#74235 = CARTESIAN_POINT ( 'NONE',  ( 13.91401389203221406, -0.3587747205144265483, 158.0376437107427137 ) ) ;
#74236 = FACE_OUTER_BOUND ( 'NONE', #4974, .T. ) ;
#74237 = ORIENTED_EDGE ( 'NONE', *, *, #67369, .T. ) ;
#74238 = B_SPLINE_SURFACE_WITH_KNOTS ( 'NONE', 3, 1, ( 
 ( #42789, #73233 ),
 ( #73720, #64646 ),
 ( #2227, #72233 ),
 ( #2727, #33665 ),
 ( #26044, #57017 ),
 ( #87954, #18435 ),
 ( #49406, #72736 ),
 ( #34170, #65141 ),
 ( #96064, #20412 ),
 ( #6697, #13302 ),
 ( #6200, #21905 ),
 ( #44280, #68114 ),
 ( #53390, #83824 ),
 ( #97552, #75209 ),
 ( #60011, #14303 ),
 ( #5701, #99034 ),
 ( #89943, #51893 ),
 ( #76202, #28052 ),
 ( #35667, #67127 ) ),
 .UNSPECIFIED., .F., .F., .F.,
 ( 4, 1, 1, 1, 1, 1, 1, 1, 1, 1, 1, 1, 1, 1, 1, 1, 4 ),
 ( 2, 2 ),
 ( 0.000000000000000000, 0.06113791491562082375, 0.1199938438512146849, 0.1782253215076174679, 0.2362564202618976927, 0.2949293769549120037, 0.3547157488097547051, 0.4167296639241671041, 0.4806644084708293629, 0.5458317702108683722, 0.6097581054261661526, 0.6729712284742268569, 0.7360168691676639563, 0.7998393981920308704, 0.8647753566655731472, 0.9310876232725697754, 0.9999999999999998890 ),
 ( 0.000000000000000000, 1.000000000000000000 ),
 .UNSPECIFIED. ) ;
#74239 = CARTESIAN_POINT ( 'NONE',  ( 30.53060340732036693, -5.220834790565956673, 0.4094854120269050823 ) ) ;
#74240 = CARTESIAN_POINT ( 'NONE',  ( 6.420673076923079314, -5.876774720514426953, 21.83974358974358765 ) ) ;
#74241 = EDGE_LOOP ( 'NONE', ( #93596, #91020, #74149, #48604 ) ) ;
#74242 = CARTESIAN_POINT ( 'NONE',  ( 18.08294815051442583, 9.098846914115775064, 11.49999999999998934 ) ) ;
#74243 = CARTESIAN_POINT ( 'NONE',  ( -122.5913838597558509, -23.73766607897671221, -1.055555164236450461 ) ) ;
#74244 = CARTESIAN_POINT ( 'NONE',  ( -48.62287095715004881, -29.50247984919015209, -1.443849546365058689 ) ) ;
#74245 = AXIS2_PLACEMENT_3D ( 'NONE', #16926, #49401, #33660 ) ;
#74246 = B_SPLINE_CURVE_WITH_KNOTS ( 'NONE', 3,
 ( #45323, #86865, #64568, #48322 ),
 .UNSPECIFIED., .F., .F.,
 ( 4, 4 ),
 ( 0.9335157282560042624, 0.9630223066614528316 ),
 .UNSPECIFIED. ) ;
#74247 = PLANE ( 'NONE',  #2310 ) ;
#74248 = ORIENTED_EDGE ( 'NONE', *, *, #9583, .F. ) ;
#74249 = CARTESIAN_POINT ( 'NONE',  ( -46.62287095715005592, -24.50321055353805022, 9.387540953477531147 ) ) ;
#74250 = FACE_OUTER_BOUND ( 'NONE', #6908, .T. ) ;
#74251 = CARTESIAN_POINT ( 'NONE',  ( 19.28819943863484454, -5.468471092112969778, -1.500000000000002220 ) ) ;
#74252 = CARTESIAN_POINT ( 'NONE',  ( -10.24336464640716216, -18.35016636821181280, 11.49999999999999645 ) ) ;
#74253 = LINE ( 'NONE', #66172, #89112 ) ;
#74254 = DIRECTION ( 'NONE',  ( 0.000000000000000000, 0.000000000000000000, 1.000000000000000000 ) ) ;
#74255 = CARTESIAN_POINT ( 'NONE',  ( -21.55788180805707555, 4.768121097544787190, 11.49999999999998934 ) ) ;
#74256 = AXIS2_PLACEMENT_3D ( 'NONE', #68868, #39915, #46043 ) ;
#74257 = CC_DESIGN_PERSON_AND_ORGANIZATION_ASSIGNMENT ( #37398, #20655, ( #69913 ) ) ;
#74258 = CARTESIAN_POINT ( 'NONE',  ( -40.38104457131870362, -25.31589329699823665, 5.081426734244629095 ) ) ;
#74259 = FACE_OUTER_BOUND ( 'NONE', #65786, .T. ) ;
#74260 = CARTESIAN_POINT ( 'NONE',  ( 3.036358173076929123, -6.376774720514420736, 20.87990785256409865 ) ) ;
#74261 = VERTEX_POINT ( 'NONE', #38255 ) ;
#74262 = CARTESIAN_POINT ( 'NONE',  ( -99.20032484257374961, -25.23532765140830136, 3.605358624617810648 ) ) ;
#74263 = CARTESIAN_POINT ( 'NONE',  ( -31.59416852699393985, -24.15543982623907127, -0.2315651400026576545 ) ) ;
#74264 = ORIENTED_EDGE ( 'NONE', *, *, #5274, .T. ) ;
#74265 = CIRCLE ( 'NONE', #48349, 5.500000000000001776 ) ;
#74266 = VERTEX_POINT ( 'NONE', #76803 ) ;
#74267 = DIRECTION ( 'NONE',  ( 0.000000000000000000, 0.9999999999976377785, 2.173523156925979128E-06 ) ) ;
#74268 = CARTESIAN_POINT ( 'NONE',  ( -5.366453405989236813, 0.000000000000000000, 19.30000000000000071 ) ) ;
#74269 = CARTESIAN_POINT ( 'NONE',  ( -76.63418747624923810, -24.15543982623907482, -0.2315651400026599305 ) ) ;
#74270 = CARTESIAN_POINT ( 'NONE',  ( -4.704028875484805639, -20.06825252194306941, -1.500000000000002220 ) ) ;
#74271 = CARTESIAN_POINT ( 'NONE',  ( 19.30674495121141376, 9.566621930910674365, 11.49999999999999645 ) ) ;
#74272 = ORIENTED_EDGE ( 'NONE', *, *, #75307, .F. ) ;
#74273 = DIRECTION ( 'NONE',  ( 0.000000000000000000, -0.000000000000000000, -1.000000000000000000 ) ) ;
#74274 = EDGE_CURVE ( 'NONE', #71246, #42693, #1711, .T. ) ;
#74275 = CARTESIAN_POINT ( 'NONE',  ( -28.32169924589829080, -0.3587747205143964613, -8.244178532169451401 ) ) ;
#74276 = CARTESIAN_POINT ( 'NONE',  ( -97.55620429048337883, -23.48783264082478084, -1.443836473390061936 ) ) ;
#74277 = CARTESIAN_POINT ( 'NONE',  ( 19.44376294880228428, 11.01865886811674677, -1.500000000000002220 ) ) ;
#74278 = CARTESIAN_POINT ( 'NONE',  ( 32.33217928425143839, -1.682774720514426114, -12.20610769812824437 ) ) ;
#74279 = CARTESIAN_POINT ( 'NONE',  ( -29.49875734969026198, -5.965225279485572685, 2.362022800118626531 ) ) ;
#74280 = ORIENTED_EDGE ( 'NONE', *, *, #11400, .T. ) ;
#74281 = DIRECTION ( 'NONE',  ( 0.000000000000000000, 0.9999999999976377785, 2.173523156925979975E-06 ) ) ;
#74282 = CARTESIAN_POINT ( 'NONE',  ( 3.671066620544169101, -5.876774720514424288, 21.47597918715562670 ) ) ;
#74283 = VECTOR ( 'NONE', #68000, 1000.000000000000114 ) ;
#74284 = CARTESIAN_POINT ( 'NONE',  ( -10.06633388967972209, 18.29571535785830960, -1.500000000000002220 ) ) ;
#74285 = EDGE_LOOP ( 'NONE', ( #55613, #75853, #22934, #91904 ) ) ;
#74287 = ORIENTED_EDGE ( 'NONE', *, *, #26586, .F. ) ;
#74286 = CARTESIAN_POINT ( 'NONE',  ( -86.60313021933721700, -23.48783264082478084, -1.443836473390066155 ) ) ;
#74288 = ORIENTED_EDGE ( 'NONE', *, *, #43712, .T. ) ;
#74289 = B_SPLINE_CURVE_WITH_KNOTS ( 'NONE', 3,
 ( #77245, #53443, #14854, #6748, #7749, #68662 ),
 .UNSPECIFIED., .F., .F.,
 ( 4, 2, 4 ),
 ( 0.000000000000000000, 0.001380901958385383774, 0.002761803916770767548 ),
 .UNSPECIFIED. ) ;
#74290 = CARTESIAN_POINT ( 'NONE',  ( -100.5100443294204808, -24.52399227489127398, 9.353111116836526406 ) ) ;
#74291 = CARTESIAN_POINT ( 'NONE',  ( 14.35337761433406811, 15.45585641580067104, -1.500000000000002220 ) ) ;
#74292 = ORIENTED_EDGE ( 'NONE', *, *, #86762, .F. ) ;
#74293 = CARTESIAN_POINT ( 'NONE',  ( -28.52287095715005094, -23.31182002239687989, -1.443836447538998202 ) ) ;
#74294 = DIRECTION ( 'NONE',  ( -0.000000000000000000, 1.000000000000000000, -0.000000000000000000 ) ) ;
#74295 = CARTESIAN_POINT ( 'NONE',  ( -120.5565306492393916, -23.85049219812686871, 10.88485053497526778 ) ) ;
#74296 = CARTESIAN_POINT ( 'NONE',  ( -68.55620429048337883, -23.48786465467241058, 11.44779295918255002 ) ) ;
#74297 = CARTESIAN_POINT ( 'NONE',  ( 7.089543269230769162, -5.876774720514413630, 19.75741185897435415 ) ) ;
#74298 = CARTESIAN_POINT ( 'NONE',  ( -17.16505717403991227, -13.39166244882208012, -1.500000000000002220 ) ) ;
#74299 = CARTESIAN_POINT ( 'NONE',  ( -81.41053730768496166, -25.24759681816308898, 6.535219080203766850 ) ) ;
#74300 = EDGE_CURVE ( 'NONE', #477, #76857, #87406, .T. ) ;
#74302 = EDGE_LOOP ( 'NONE', ( #25237, #81547, #24319, #54110 ) ) ;
#74301 = CARTESIAN_POINT ( 'NONE',  ( 11.81759748825469281, -18.92407201980706333, 11.49999999999999645 ) ) ;
#74303 = LINE ( 'NONE', #6281, #72882 ) ;
#74304 = CARTESIAN_POINT ( 'NONE',  ( 7.139069293134643779, -6.376774720514422512, 20.58118917620081945 ) ) ;
#74305 = DIRECTION ( 'NONE',  ( 2.860369681942282691E-39, 2.173523156925979128E-06, -0.9999999999976378895 ) ) ;
#74306 = ORIENTED_EDGE ( 'NONE', *, *, #83143, .T. ) ;
#74307 = B_SPLINE_CURVE_WITH_KNOTS ( 'NONE', 3,
 ( #29014, #90918, #21386, #52363 ),
 .UNSPECIFIED., .F., .F.,
 ( 4, 4 ),
 ( 0.000000000000000000, 0.0001000000000000028644 ),
 .UNSPECIFIED. ) ;
#74309 = ORIENTED_EDGE ( 'NONE', *, *, #93972, .F. ) ;
#74308 = CARTESIAN_POINT ( 'NONE',  ( -40.62287095715007013, -23.85196035786900381, -0.8779234886474998056 ) ) ;
#74310 = EDGE_LOOP ( 'NONE', ( #18314, #8876, #72296, #28959 ) ) ;
#74311 = ADVANCED_FACE ( 'NONE', ( #85429 ), #100130, .T. ) ;
#74312 = CARTESIAN_POINT ( 'NONE',  ( -6.499999999999992895, 1.000000000000000000, -2.500000000000001332 ) ) ;
#74313 = CARTESIAN_POINT ( 'NONE',  ( -128.5228709571500758, -23.47593901973090524, -1.443836447538996204 ) ) ;
#74314 = EDGE_CURVE ( 'NONE', #49492, #50837, #202, .T. ) ;
#74315 = B_SPLINE_CURVE_WITH_KNOTS ( 'NONE', 3,
 ( #92482, #55444, #7754, #1152 ),
 .UNSPECIFIED., .F., .F.,
 ( 4, 4 ),
 ( 0.5508933794777274295, 0.5598998107498430743 ),
 .UNSPECIFIED. ) ;
#74316 = CARTESIAN_POINT ( 'NONE',  ( -67.55620429048340725, -23.48786465467240703, 11.44779295918254647 ) ) ;
#74317 = DIRECTION ( 'NONE',  ( -1.000000000000000000, 0.000000000000000000, 0.000000000000000000 ) ) ;
#74318 = CARTESIAN_POINT ( 'NONE',  ( -51.16325253692608754, -25.31574324955554189, 5.002592196407556813 ) ) ;
#74319 = ORIENTED_EDGE ( 'NONE', *, *, #70735, .T. ) ;
#74320 = CARTESIAN_POINT ( 'NONE',  ( 3.017506814366913481, 19.14668354085002733, 11.49999999999999645 ) ) ;
#74321 = DIRECTION ( 'NONE',  ( -8.334928612639484546E-17, -1.000000000000000000, -7.321843366904296032E-17 ) ) ;
#74322 = EDGE_CURVE ( 'NONE', #53302, #37074, #53766, .T. ) ;
#74323 = ORIENTED_EDGE ( 'NONE', *, *, #73817, .F. ) ;
#74324 = CARTESIAN_POINT ( 'NONE',  ( 3.672440828437461224, -5.876774720514402972, 18.52532110411518573 ) ) ;
#74325 = CARTESIAN_POINT ( 'NONE',  ( 2.628295812946869425, -6.376774720514411854, 19.40849182188139110 ) ) ;
#74326 = FACE_OUTER_BOUND ( 'NONE', #58696, .T. ) ;
#74327 = AXIS2_PLACEMENT_3D ( 'NONE', #29170, #4843, #51025 ) ;
#74328 = PLANE ( 'NONE',  #9911 ) ;
#74329 = CARTESIAN_POINT ( 'NONE',  ( -12.94911239430987315, -14.73082512860577609, 11.49999999999998934 ) ) ;
#74330 = CARTESIAN_POINT ( 'NONE',  ( -66.55620429048339304, -23.48786465467241058, 11.44779295918255002 ) ) ;
#74331 = ORIENTED_EDGE ( 'NONE', *, *, #42798, .T. ) ;
#74332 = CARTESIAN_POINT ( 'NONE',  ( -19.93307770644097232, -8.117153041090405807, 11.49999999999998934 ) ) ;
#74333 = CARTESIAN_POINT ( 'NONE',  ( -121.5562042904834215, -23.48783264082479505, -1.443836473390058828 ) ) ;
#74334 = CARTESIAN_POINT ( 'NONE',  ( -71.26594616156928907, -25.25639464561320935, 6.471657872805320011 ) ) ;
#74335 = FACE_OUTER_BOUND ( 'NONE', #77861, .T. ) ;
#74336 = LINE ( 'NONE', #4827, #39110 ) ;
#74337 = CARTESIAN_POINT ( 'NONE',  ( 14.87233727408824713, -17.56007624320114857, -1.500000000000002220 ) ) ;
#74338 = DATE_AND_TIME ( #29156, #50575 ) ;
#74339 = LINE ( 'NONE', #43894, #2935 ) ;
#74340 = CARTESIAN_POINT ( 'NONE',  ( -53.58736094297834285, -24.34968618360933590, 0.1864209137778786440 ) ) ;
#74341 = CARTESIAN_POINT ( 'NONE',  ( 19.08902475966321788, 6.433202353099247262, 11.49999999999999645 ) ) ;
#74342 = CARTESIAN_POINT ( 'NONE',  ( -45.62287095715004881, -23.47596703998600276, 11.44779298504227505 ) ) ;
#74343 = DIRECTION ( 'NONE',  ( -0.000000000000000000, -1.000000000000000000, -0.000000000000000000 ) ) ;
#74344 = AXIS2_PLACEMENT_3D ( 'NONE', #99913, #60404, #14191 ) ;
#74345 = CARTESIAN_POINT ( 'NONE',  ( -4.930333147521421822, -5.876774720514410966, 19.46306892155547530 ) ) ;
#74346 = DIRECTION ( 'NONE',  ( 0.000000000000000000, 0.000000000000000000, -1.000000000000000000 ) ) ;
#74347 = CARTESIAN_POINT ( 'NONE',  ( -126.5562042904833646, -23.48786465467241769, 11.44779295918253581 ) ) ;
#74348 = CARTESIAN_POINT ( 'NONE',  ( -19.77004505525285083, 2.005399880840008642, 11.49999999999998934 ) ) ;
#74349 = CARTESIAN_POINT ( 'NONE',  ( 32.40199294184732537, 6.475225279485573360, -12.82361242714782712 ) ) ;
#74350 = CARTESIAN_POINT ( 'NONE',  ( 16.89532177248590372, -10.13005384644002227, -1.500000000000002220 ) ) ;
#74351 = PLANE ( 'NONE',  #94527 ) ;
#74352 = CARTESIAN_POINT ( 'NONE',  ( 30.93860345374796594, 6.475225279485573360, 19.84760796525321780 ) ) ;
#74353 = CARTESIAN_POINT ( 'NONE',  ( -111.5228709571500616, -24.65952944569305316, 1.056160979905704123 ) ) ;
#74354 = CARTESIAN_POINT ( 'NONE',  ( -13.08992234710881064, 15.94516925376868244, 11.49999999999999645 ) ) ;
#74355 = CARTESIAN_POINT ( 'NONE',  ( -75.62287095715005592, -23.47596703998600631, 11.44779298504227860 ) ) ;
#74356 = CARTESIAN_POINT ( 'NONE',  ( 30.32108885906865936, 5.356774720514427379, 3.274824222184972822 ) ) ;
#74357 = AXIS2_PLACEMENT_3D ( 'NONE', #329, #62244, #1343 ) ;
#74359 = EDGE_CURVE ( 'NONE', #26538, #95555, #96053, .T. ) ;
#74358 = CARTESIAN_POINT ( 'NONE',  ( 3.867644355387967359, 22.30990608135428488, 11.49999999999999645 ) ) ;
#74360 = ORIENTED_EDGE ( 'NONE', *, *, #58901, .T. ) ;
#74361 = CARTESIAN_POINT ( 'NONE',  ( -25.53098197642538736, -24.92569209777881056, 4.942811685741776984 ) ) ;
#74362 = CARTESIAN_POINT ( 'NONE',  ( 8.676776695296462449, 18.57322330470351091, 0.000000000000000000 ) ) ;
#74363 = CARTESIAN_POINT ( 'NONE',  ( -63.58341162693596971, -24.51314013834316796, 0.6176544820404160641 ) ) ;
#74364 = DIRECTION ( 'NONE',  ( 0.000000000000000000, -2.173523156925979975E-06, 0.9999999999976378895 ) ) ;
#74365 = ORIENTED_EDGE ( 'NONE', *, *, #44669, .F. ) ;
#74366 = ORIENTED_EDGE ( 'NONE', *, *, #28287, .F. ) ;
#74367 = CARTESIAN_POINT ( 'NONE',  ( 4.621320343559255583, 11.49999999999999467, 2.100000000000000089 ) ) ;
#74368 = CARTESIAN_POINT ( 'NONE',  ( 22.56601425305882813, -3.627385684441148506, 11.49999999999998934 ) ) ;
#74369 = CARTESIAN_POINT ( 'NONE',  ( -29.56144451721570832, -23.65455177597154091, -1.055554856561816246 ) ) ;
#74370 = B_SPLINE_CURVE_WITH_KNOTS ( 'NONE', 3,
 ( #69158, #76748, #43477, #4908, #30594, #28238, #31090, #69668 ),
 .UNSPECIFIED., .F., .F.,
 ( 4, 2, 2, 4 ),
 ( -0.001240666984355830215, -0.0002401179793394881724, 0.0007604310256768538698, 0.002761529035709538171 ),
 .UNSPECIFIED. ) ;
#74371 = CARTESIAN_POINT ( 'NONE',  ( 5.819084965910729323, 20.79142713412266730, -1.500000000000002220 ) ) ;
#74372 = CARTESIAN_POINT ( 'NONE',  ( -113.6235176254694750, -24.66019654487200086, 8.947790411086106843 ) ) ;
#74373 = DIRECTION ( 'NONE',  ( 0.000000000000000000, -2.173523156925979552E-06, 0.9999999999976378895 ) ) ;
#74374 = CARTESIAN_POINT ( 'NONE',  ( 21.16815136333514502, -7.790938087775149512, 11.49999999999999645 ) ) ;
#74375 = ORIENTED_EDGE ( 'NONE', *, *, #83611, .F. ) ;
#74376 = CARTESIAN_POINT ( 'NONE',  ( -69.64187497903644442, -25.31612452842404437, 5.000677404731540321 ) ) ;
#74377 = CARTESIAN_POINT ( 'NONE',  ( 21.66556372666567754, 3.824538051775513647, -1.500000000000002220 ) ) ;
#74378 = EDGE_CURVE ( 'NONE', #81873, #95644, #16049, .T. ) ;
#74379 = CARTESIAN_POINT ( 'NONE',  ( -111.5570160696827173, -23.73766607897670511, -1.055555164236450461 ) ) ;
#74380 = LINE ( 'NONE', #35825, #54113 ) ;
#74381 = VERTEX_POINT ( 'NONE', #34659 ) ;
#74382 = DIRECTION ( 'NONE',  ( -0.000000000000000000, -1.000000000000000000, -0.000000000000000000 ) ) ;
#74383 = CARTESIAN_POINT ( 'NONE',  ( -107.5228709571500758, -24.64965694238575011, 8.947790433994192938 ) ) ;
#74384 = EDGE_LOOP ( 'NONE', ( #99028, #27448, #87033, #79491 ) ) ;
#74385 = CARTESIAN_POINT ( 'NONE',  ( -84.62287095715005592, -24.64898659630367561, 1.056161002820826145 ) ) ;
#74386 = VECTOR ( 'NONE', #1381, 1000.000000000000000 ) ;
#74387 = EDGE_CURVE ( 'NONE', #39577, #17025, #88941, .T. ) ;
#74388 = ORIENTED_EDGE ( 'NONE', *, *, #11412, .F. ) ;
#74389 = AXIS2_PLACEMENT_3D ( 'NONE', #7845, #36811, #14453 ) ;
#74390 = ORIENTED_EDGE ( 'NONE', *, *, #68768, .F. ) ;
#74391 = DIRECTION ( 'NONE',  ( -3.773278334453080206E-23, 0.9999999999976377785, 2.173523156925979975E-06 ) ) ;
#74392 = DIRECTION ( 'NONE',  ( -3.773278334453079030E-23, 0.9999999999976377785, 2.173523156925979128E-06 ) ) ;
#74393 = CARTESIAN_POINT ( 'NONE',  ( -115.6228709571500417, -25.00182538069145721, 7.747789668545097541 ) ) ;
#74394 = CARTESIAN_POINT ( 'NONE',  ( -19.95082702767638239, -4.354873812894156870, -1.500000000000002220 ) ) ;
#74395 = ORIENTED_EDGE ( 'NONE', *, *, #97337, .F. ) ;
#74396 = CARTESIAN_POINT ( 'NONE',  ( -71.03488587359156270, -25.06952888890338471, 7.387088048512346461 ) ) ;
#74397 = EDGE_CURVE ( 'NONE', #47456, #73995, #10001, .T. ) ;
#74398 = VECTOR ( 'NONE', #46081, 1000.000000000000000 ) ;
#74399 = LINE ( 'NONE', #22088, #80643 ) ;
#74400 = ADVANCED_FACE ( 'NONE', ( #57510 ), #49395, .T. ) ;
#74401 = CARTESIAN_POINT ( 'NONE',  ( -105.5906832248129490, -24.40034930558991277, 0.3402023900116059041 ) ) ;
#74402 = CARTESIAN_POINT ( 'NONE',  ( -70.52593452554701514, -25.03149848527395704, 7.557317387464395075 ) ) ;
#74403 = EDGE_LOOP ( 'NONE', ( #4417, #51681, #96400, #25064 ) ) ;
#74404 = CARTESIAN_POINT ( 'NONE',  ( -122.6228709571500417, -23.47593901973091235, -1.443836447538997536 ) ) ;
#74405 = CARTESIAN_POINT ( 'NONE',  ( -88.22287095715005023, -23.47593901973090169, -1.443836447538996870 ) ) ;
#74406 = ADVANCED_FACE ( 'NONE', ( #64130 ), #95049, .T. ) ;
#74407 = ORIENTED_EDGE ( 'NONE', *, *, #90390, .F. ) ;
#74408 = VECTOR ( 'NONE', #592, 1000.000000000000114 ) ;
#74409 = CARTESIAN_POINT ( 'NONE',  ( 19.72710162658169608, 6.580912942549038469, 11.49999999999998934 ) ) ;
#74410 = ORIENTED_EDGE ( 'NONE', *, *, #44663, .F. ) ;
#74412 = ORIENTED_EDGE ( 'NONE', *, *, #60112, .F. ) ;
#74411 = CARTESIAN_POINT ( 'NONE',  ( -39.56951972374358206, -25.30125091222718225, 4.659097539256057630 ) ) ;
#74413 = CARTESIAN_POINT ( 'NONE',  ( -51.52764846858840997, -25.12217663958179870, 6.187573060801323521 ) ) ;
#74414 = PLANE ( 'NONE',  #37317 ) ;
#74415 = ORIENTED_EDGE ( 'NONE', *, *, #29261, .T. ) ;
#74416 = ORIENTED_EDGE ( 'NONE', *, *, #40680, .F. ) ;
#74417 = CARTESIAN_POINT ( 'NONE',  ( -112.6228709571500701, -23.48783264082479150, -1.443836473390060160 ) ) ;
#74418 = VECTOR ( 'NONE', #74987, 1000.000000000000000 ) ;
#74419 = CARTESIAN_POINT ( 'NONE',  ( -118.3656746162385645, -25.21753786267797892, 3.540021004441392893 ) ) ;
#74420 = CARTESIAN_POINT ( 'NONE',  ( -4.977357939505175466, -5.876774720514410077, 19.14913681718893557 ) ) ;
#74421 = B_SPLINE_CURVE_WITH_KNOTS ( 'NONE', 3,
 ( #40916, #26696, #88102, #19070 ),
 .UNSPECIFIED., .F., .F.,
 ( 4, 4 ),
 ( 0.000000000000000000, 9.999999999997510880E-05 ),
 .UNSPECIFIED. ) ;
#74422 = CARTESIAN_POINT ( 'NONE',  ( -43.60020624437694181, -23.96169478059712432, 10.65365249895718769 ) ) ;
#74423 = ADVANCED_FACE ( 'NONE', ( #48889 ), #26033, .F. ) ;
#74425 = ORIENTED_EDGE ( 'NONE', *, *, #41191, .F. ) ;
#74424 = CARTESIAN_POINT ( 'NONE',  ( -21.77411086464670831, -3.637377321037103872, 11.49999999999999645 ) ) ;
#74426 = CARTESIAN_POINT ( 'NONE',  ( -72.62287095715005592, -23.48783264082478084, -1.443836473390067265 ) ) ;
#74427 = CARTESIAN_POINT ( 'NONE',  ( 22.24477432615492134, 4.004077059304647968, 11.49999999999998934 ) ) ;
#74429 = ORIENTED_EDGE ( 'NONE', *, *, #12202, .T. ) ;
#74428 = FACE_OUTER_BOUND ( 'NONE', #76552, .T. ) ;
#74430 = ORIENTED_EDGE ( 'NONE', *, *, #1362, .T. ) ;
#74431 = CARTESIAN_POINT ( 'NONE',  ( 30.93860345374796594, 6.475225279485573360, 28.07639619989136293 ) ) ;
#74432 = EDGE_CURVE ( 'NONE', #33918, #21622, #46248, .T. ) ;
#74433 = EDGE_CURVE ( 'NONE', #15452, #49598, #19421, .T. ) ;
#74434 = B_SPLINE_SURFACE_WITH_KNOTS ( 'NONE', 3, 1, ( 
 ( #62154, #63154 ),
 ( #8849, #45928 ),
 ( #76350, #23561 ),
 ( #53045, #92576 ),
 ( #53544, #39797 ),
 ( #99678, #70755 ),
 ( #83975, #68758 ),
 ( #736, #30181 ),
 ( #30686, #76839 ),
 ( #8348, #54044 ),
 ( #69252, #54531 ),
 ( #23054, #7847 ),
 ( #7341, #22553 ),
 ( #31689, #238 ),
 ( #55037, #100170 ),
 ( #84969, #77347 ),
 ( #38796, #15951 ),
 ( #70253, #93572 ),
 ( #41822, #18462 ) ),
 .UNSPECIFIED., .F., .F., .F.,
 ( 4, 1, 1, 1, 1, 1, 1, 1, 1, 1, 1, 1, 1, 1, 1, 1, 4 ),
 ( 2, 2 ),
 ( 0.000000000000000000, 0.07524330859112852987, 0.1472088117202518809, 0.2164470898547687372, 0.2840250416193483840, 0.3506554491966432097, 0.4150313178410243720, 0.4796298309645117830, 0.5446516341371376857, 0.6080442396977419062, 0.6678275650288183485, 0.7251142466493384342, 0.7809917079106386550, 0.8355270040618592020, 0.8894381545415823709, 0.9440720891799450065, 1.000000000000000000 ),
 ( 0.000000000000000000, 1.000000000000000000 ),
 .UNSPECIFIED. ) ;
#74435 = CARTESIAN_POINT ( 'NONE',  ( -57.55355702163512177, -23.96169478059713143, 10.65365249895718058 ) ) ;
#74436 = ORIENTED_EDGE ( 'NONE', *, *, #19534, .F. ) ;
#74437 = DIRECTION ( 'NONE',  ( 0.000000000000000000, 1.000000000000000000, 0.000000000000000000 ) ) ;
#74438 = CARTESIAN_POINT ( 'NONE',  ( 1.165341552704713513, 22.26021350444069213, -1.500000000000002220 ) ) ;
#74439 = DIRECTION ( 'NONE',  ( -1.000000000000000000, -3.773278334444167608E-23, -8.201307810031802745E-29 ) ) ;
#74440 = EDGE_CURVE ( 'NONE', #54707, #61052, #72724, .T. ) ;
#74441 = EDGE_LOOP ( 'NONE', ( #20247, #2764, #79301, #96058 ) ) ;
#74442 = LINE ( 'NONE', #14022, #95116 ) ;
#74443 = CARTESIAN_POINT ( 'NONE',  ( 22.81105451610979173, 500000.0000000000582, -18.46691820600746681 ) ) ;
#74444 = ADVANCED_FACE ( 'NONE', ( #48383 ), #3227, .F. ) ;
#74445 = CARTESIAN_POINT ( 'NONE',  ( -70.52287095715007581, -23.47593901973090524, -1.443836447538997092 ) ) ;
#74446 = DIRECTION ( 'NONE',  ( 0.000000000000000000, -0.000000000000000000, 1.000000000000000000 ) ) ;
#74447 = EDGE_CURVE ( 'NONE', #67104, #27095, #2217, .T. ) ;
#74448 = CARTESIAN_POINT ( 'NONE',  ( -18.91883139384513157, -4.797682538509264738, -1.500000000000002220 ) ) ;
#74449 = CARTESIAN_POINT ( 'NONE',  ( 20.36625868517733196, 6.724766957447481097, -1.500000000000002220 ) ) ;
#74450 = CARTESIAN_POINT ( 'NONE',  ( -1.304987980769231948, -6.376774720514415407, 19.76512419871795245 ) ) ;
#74451 = CARTESIAN_POINT ( 'NONE',  ( -41.52287095715006870, -29.50247984919015209, -1.443849546365060466 ) ) ;
#74452 = CARTESIAN_POINT ( 'NONE',  ( -48.52287095715006160, -23.47596703998600631, 11.44779298504229104 ) ) ;
#74453 = CARTESIAN_POINT ( 'NONE',  ( -12.44792101662413408, -19.12764231104124946, -1.500000000000002220 ) ) ;
#74454 = DIRECTION ( 'NONE',  ( 1.000000000000000000, 0.000000000000000000, 0.000000000000000000 ) ) ;
#74455 = CARTESIAN_POINT ( 'NONE',  ( -49.50841769935765768, -25.27292115247390569, 3.984447733149576898 ) ) ;
#74456 = CARTESIAN_POINT ( 'NONE',  ( -50.52287095715006160, -23.48786465467241058, 11.44779295918255002 ) ) ;
#74457 = CARTESIAN_POINT ( 'NONE',  ( 6.038693664686949347, 19.05185810397003721, 11.49999999999999645 ) ) ;
#74458 = CARTESIAN_POINT ( 'NONE',  ( -101.6228709571500559, -24.66019654487199730, 8.947790411086121054 ) ) ;
#74459 = CIRCLE ( 'NONE', #64791, 2.249999999999998668 ) ;
#74460 = CARTESIAN_POINT ( 'NONE',  ( -74.51666087527418370, -23.73791477778911840, 11.05961554403170588 ) ) ;
#74461 = PLANE ( 'NONE',  #29391 ) ;
#74462 = EDGE_LOOP ( 'NONE', ( #3425, #8420, #74410, #49770 ) ) ;
#74463 = CARTESIAN_POINT ( 'NONE',  ( -26.02075258637046673, -24.72833475862651653, 2.618636308606199226 ) ) ;
#74464 = CARTESIAN_POINT ( 'NONE',  ( -124.5228709571501611, -24.34917612406838572, 0.1852690917426621509 ) ) ;
#74465 = CARTESIAN_POINT ( 'NONE',  ( 19.97611268498323511, -8.487024919450899318, 11.49999999999998934 ) ) ;
#74466 = DIRECTION ( 'NONE',  ( -1.000000000000000000, 0.000000000000000000, 0.000000000000000000 ) ) ;
#74467 = AXIS2_PLACEMENT_3D ( 'NONE', #66079, #75151, #44219 ) ;
#74468 = CARTESIAN_POINT ( 'NONE',  ( -19.43040671759091609, -1.856541507571394467, -1.500000000000002220 ) ) ;
#74469 = CARTESIAN_POINT ( 'NONE',  ( -100.3031470170733712, -25.13382359911133435, 7.097745423514688845 ) ) ;
#74471 = ORIENTED_EDGE ( 'NONE', *, *, #68896, .F. ) ;
#74470 = CIRCLE ( 'NONE', #45283, 1.000000000000000000 ) ;
#74472 = AXIS2_PLACEMENT_3D ( 'NONE', #36437, #19702, #4992 ) ;
#74473 = CARTESIAN_POINT ( 'NONE',  ( 14.52511747680497933, -6.475225279485573360, -27.86035006098926559 ) ) ;
#74474 = CARTESIAN_POINT ( 'NONE',  ( 14.46511082492616573, -14.46070965572739730, 11.49999999999999645 ) ) ;
#74475 = CARTESIAN_POINT ( 'NONE',  ( 11.84174468958795323, -6.475225279485574248, -27.06880646454217043 ) ) ;
#74476 = CARTESIAN_POINT ( 'NONE',  ( -39.62287095715005592, -24.64965695001468404, 8.947790433994187609 ) ) ;
#74477 = VECTOR ( 'NONE', #89521, 1000.000000000000000 ) ;
#74478 = VERTEX_POINT ( 'NONE', #34161 ) ;
#74479 = DIRECTION ( 'NONE',  ( -0.000000000000000000, -0.000000000000000000, 1.000000000000000000 ) ) ;
#74480 = DIRECTION ( 'NONE',  ( -3.773278334453079618E-23, 0.9999999999976377785, 2.173523156925979975E-06 ) ) ;
#74481 = CARTESIAN_POINT ( 'NONE',  ( -78.62287095715005592, -23.47593901973091235, -1.443836447539004642 ) ) ;
#74482 = B_SPLINE_CURVE_WITH_KNOTS ( 'NONE', 3,
 ( #29507, #14277, #3825, #60487 ),
 .UNSPECIFIED., .F., .F.,
 ( 4, 4 ),
 ( 0.000000000000000000, 9.999999999998897304E-05 ),
 .UNSPECIFIED. ) ;
#74483 = CARTESIAN_POINT ( 'NONE',  ( -85.52287095715006160, -23.85196035786899316, -0.8779234886475173472 ) ) ;
#74484 = EDGE_LOOP ( 'NONE', ( #95606, #96363, #84580, #20183 ) ) ;
#74485 = CARTESIAN_POINT ( 'NONE',  ( -80.34687923781922336, -25.14083923594767356, 2.947789366383932297 ) ) ;
#74486 = CARTESIAN_POINT ( 'NONE',  ( 22.64363655503811046, -4.068770074275382953, 11.49999999999999645 ) ) ;
#74487 = CARTESIAN_POINT ( 'NONE',  ( -22.52399778787742335, 3.408274809117095572, -1.500000000000002220 ) ) ;
#74488 = CARTESIAN_POINT ( 'NONE',  ( -110.5527773381347458, -24.40133493613049609, 9.663955038902800609 ) ) ;
#74489 = CARTESIAN_POINT ( 'NONE',  ( -40.52287095715006160, -23.84047902841603417, -0.8780736468305391229 ) ) ;
#74490 = CARTESIAN_POINT ( 'NONE',  ( -98.89303308397303738, -25.25494757631710385, 6.110950176066591411 ) ) ;
#74491 = CARTESIAN_POINT ( 'NONE',  ( -70.52287095715007581, -25.00158670708909625, 2.256160236439166411 ) ) ;
#74492 = CARTESIAN_POINT ( 'NONE',  ( -110.5886823328070534, -24.63355581998384380, 0.9682620441943931011 ) ) ;
#74493 = CARTESIAN_POINT ( 'NONE',  ( 19.94191871449930531, -9.063712221575384476, -1.500000000000002220 ) ) ;
#74494 = CARTESIAN_POINT ( 'NONE',  ( -59.58953762381670316, -24.64965694238406968, 8.947790433994660120 ) ) ;
#74495 = EDGE_CURVE ( 'NONE', #26773, #36250, #64437, .T. ) ;
#74496 = CARTESIAN_POINT ( 'NONE',  ( -50.58953762381672448, -23.48786465467241058, 11.44779295918255180 ) ) ;
#74497 = CARTESIAN_POINT ( 'NONE',  ( -120.6228709571500985, -24.62226745350444190, 0.9660975649729637293 ) ) ;
#74498 = CARTESIAN_POINT ( 'NONE',  ( -96.52287095715006160, -24.50321055353804311, 9.387540953477515160 ) ) ;
#74499 = ORIENTED_EDGE ( 'NONE', *, *, #15401, .F. ) ;
#74500 = CARTESIAN_POINT ( 'NONE',  ( 13.86372479123709311, 15.02075200336711092, 11.49999999999998934 ) ) ;
#74501 = ORIENTED_EDGE ( 'NONE', *, *, #50757, .T. ) ;
#74502 = ORIENTED_EDGE ( 'NONE', *, *, #88517, .T. ) ;
#74503 = ORIENTED_EDGE ( 'NONE', *, *, #65861, .F. ) ;
#74504 = VERTEX_POINT ( 'NONE', #81327 ) ;
#74505 = CARTESIAN_POINT ( 'NONE',  ( 15.83906049732654608, 16.74391201645830662, -1.500000000000002220 ) ) ;
#74506 = CARTESIAN_POINT ( 'NONE',  ( -57.62287095715004881, -29.50250243563736774, 8.947779886222145151 ) ) ;
#74507 = CARTESIAN_POINT ( 'NONE',  ( 0.8729654516333695824, -20.24016528753796962, -1.500000000000002220 ) ) ;
#74508 = VERTEX_POINT ( 'NONE', #25031 ) ;
#74509 = EDGE_CURVE ( 'NONE', #82785, #30829, #56007, .T. ) ;
#74510 = CARTESIAN_POINT ( 'NONE',  ( -93.62287095715005592, -29.50250243563736774, 8.947779886222139822 ) ) ;
#74511 = ADVANCED_FACE ( 'NONE', ( #6688 ), #45263, .T. ) ;
#74512 = CARTESIAN_POINT ( 'NONE',  ( -48.52287095715006870, -24.51387760970724372, 9.387446482453402297 ) ) ;
#74513 = EDGE_CURVE ( 'NONE', #6511, #72410, #6351, .T. ) ;
#74514 = CARTESIAN_POINT ( 'NONE',  ( -51.62287095715007013, -24.33927499327855415, 9.819080762295820719 ) ) ;
#74515 = CARTESIAN_POINT ( 'NONE',  ( -41.62287095715006302, -23.47596703998600276, 11.44779298504227505 ) ) ;
#74517 = EDGE_LOOP ( 'NONE', ( #41458, #16381, #16507, #26740 ) ) ;
#74516 = CARTESIAN_POINT ( 'NONE',  ( 9.194277187580093269, -19.27880637823015419, 11.49999999999999645 ) ) ;
#74518 = CARTESIAN_POINT ( 'NONE',  ( -55.52287095715005449, -23.84047902841601996, -0.8780736468305719855 ) ) ;
#74519 = EDGE_CURVE ( 'NONE', #90247, #3242, #20400, .T. ) ;
#74520 = ORIENTED_EDGE ( 'NONE', *, *, #47746, .F. ) ;
#74521 = CARTESIAN_POINT ( 'NONE',  ( 15.88595335714125589, -15.59144682577495189, -1.500000000000002220 ) ) ;
#74522 = B_SPLINE_CURVE_WITH_KNOTS ( 'NONE', 3,
 ( #87475, #17967, #40305, #78842 ),
 .UNSPECIFIED., .F., .F.,
 ( 4, 4 ),
 ( 0.000000000000000000, 1.000000000000000000 ),
 .UNSPECIFIED. ) ;
#74523 = CARTESIAN_POINT ( 'NONE',  ( -4.528870947376731237, 20.18191347215651987, 11.49999999999998934 ) ) ;
#74524 = VECTOR ( 'NONE', #28069, 1000.000000000000000 ) ;
#74525 = VERTEX_POINT ( 'NONE', #13791 ) ;
#74526 = CARTESIAN_POINT ( 'NONE',  ( -28.57383953491463657, -24.50287364620303521, 1.056161677404372501 ) ) ;
#74527 = EDGE_LOOP ( 'NONE', ( #96488, #97771, #73702, #7990 ) ) ;
#74528 = PLANE ( 'NONE',  #5682 ) ;
#74529 = CIRCLE ( 'NONE', #24331, 2.249999999999998668 ) ;
#74530 = ORIENTED_EDGE ( 'NONE', *, *, #48646, .T. ) ;
#74531 = CARTESIAN_POINT ( 'NONE',  ( -17.10473743203234775, -12.04273770408705246, -1.500000000000002220 ) ) ;
#74532 = EDGE_CURVE ( 'NONE', #32327, #71712, #24500, .T. ) ;
#74533 = CARTESIAN_POINT ( 'NONE',  ( -0.1377007522546883911, -21.91379463844567965, 11.49999999999999645 ) ) ;
#74534 = CARTESIAN_POINT ( 'NONE',  ( -37.63489630462677127, -24.35071581493542325, 9.817618358456030592 ) ) ;
#74535 = CARTESIAN_POINT ( 'NONE',  ( 12.90280524143238594, -18.44629484376132922, -1.500000000000002220 ) ) ;
#74536 = CIRCLE ( 'NONE', #46945, 1.500000000000001332 ) ;
#74537 = CARTESIAN_POINT ( 'NONE',  ( 17.09260067683297635, -12.12037977771017871, -1.500000000000002220 ) ) ;
#74538 = DIRECTION ( 'NONE',  ( 0.000000000000000000, -0.9999999999976377785, -2.173523156925979975E-06 ) ) ;
#74539 = CARTESIAN_POINT ( 'NONE',  ( -81.62287095715004170, -23.48786465467241058, 11.44779295918254647 ) ) ;
#74540 = DIRECTION ( 'NONE',  ( 0.000000000000000000, -1.000000000000000000, 0.000000000000000000 ) ) ;
#74542 = EDGE_CURVE ( 'NONE', #40372, #36906, #21397, .T. ) ;
#74541 = ORIENTED_EDGE ( 'NONE', *, *, #79272, .T. ) ;
#74543 = AXIS2_PLACEMENT_3D ( 'NONE', #4529, #35478, #41595 ) ;
#74544 = ORIENTED_EDGE ( 'NONE', *, *, #6475, .T. ) ;
#74545 = AXIS2_PLACEMENT_3D ( 'NONE', #8353, #53178, #6493 ) ;
#74546 = EDGE_LOOP ( 'NONE', ( #53812, #98607, #49367, #1742, #55425, #75157, #57928 ) ) ;
#74547 = DIRECTION ( 'NONE',  ( 1.000000000000000000, -7.960204194457801640E-17, 0.000000000000000000 ) ) ;
#74548 = ADVANCED_FACE ( 'NONE', ( #91416 ), #59488, .T. ) ;
#74549 = CIRCLE ( 'NONE', #32403, 2.500000000000000444 ) ;
#74550 = CARTESIAN_POINT ( 'NONE',  ( 11.86944616785735818, -17.87650476368427732, -1.500000000000002220 ) ) ;
#74551 = CARTESIAN_POINT ( 'NONE',  ( 9.299999999999993605, 12.00000000000002309, 2.100000000000000089 ) ) ;
#74552 = ORIENTED_EDGE ( 'NONE', *, *, #85735, .F. ) ;
#74553 = CARTESIAN_POINT ( 'NONE',  ( -3.607955376466517095, 20.77440192976073519, 11.49999999999998934 ) ) ;
#74554 = CARTESIAN_POINT ( 'NONE',  ( -100.3262102087699787, -25.19537855052032782, 3.296406834188733370 ) ) ;
#74555 = CARTESIAN_POINT ( 'NONE',  ( -27.86046284349298219, -0.3587747205143967943, -8.091963836038763347 ) ) ;
#74556 = DIRECTION ( 'NONE',  ( -3.246014568247801031E-12, 0.000000000000000000, 1.000000000000000000 ) ) ;
#74557 = CARTESIAN_POINT ( 'NONE',  ( 11.80640562518893866, -6.475225279485576024, -27.06722565682295567 ) ) ;
#74558 = CARTESIAN_POINT ( 'NONE',  ( -0.5218785734906133955, -5.876774720514409189, 19.14848118821636547 ) ) ;
#74559 = CARTESIAN_POINT ( 'NONE',  ( -22.05048665130746954, -1.834114841651104832, -1.500000000000002220 ) ) ;
#74560 = CARTESIAN_POINT ( 'NONE',  ( -81.54104209881381848, -24.66019654487198665, 8.947790411086131712 ) ) ;
#74561 = CARTESIAN_POINT ( 'NONE',  ( -109.8650282762807393, -25.28040082146351608, 5.784628005357986602 ) ) ;
#74562 = CARTESIAN_POINT ( 'NONE',  ( 10.46399479596396453, -2.682774720514426559, -27.03001098546561920 ) ) ;
#74563 = EDGE_CURVE ( 'NONE', #47721, #23558, #58503, .T. ) ;
#74564 = CARTESIAN_POINT ( 'NONE',  ( -100.5937343098658943, -24.15503026093918137, -0.2815557561904373229 ) ) ;
#74565 = CARTESIAN_POINT ( 'NONE',  ( 4.555389213293416617, -20.86945110937667280, -1.500000000000002220 ) ) ;
#74566 = CARTESIAN_POINT ( 'NONE',  ( -26.16584078008908421, -24.94396127023346210, 5.878266566680999894 ) ) ;
#74567 = CARTESIAN_POINT ( 'NONE',  ( -51.95662050938321386, -25.03707831087709579, 7.590867751134624974 ) ) ;
#74568 = ADVANCED_FACE ( 'NONE', ( #37140 ), #68103, .T. ) ;
#74569 = DIRECTION ( 'NONE',  ( -1.000000000000000000, 0.000000000000000000, 0.000000000000000000 ) ) ;
#74570 = CARTESIAN_POINT ( 'NONE',  ( -70.34217583644009153, -25.29972316739413429, 4.286145325355288804 ) ) ;
#74571 = CARTESIAN_POINT ( 'NONE',  ( 20.84710439121840864, 8.857176948214046774, -1.500000000000002220 ) ) ;
#74572 = ORIENTED_EDGE ( 'NONE', *, *, #77606, .F. ) ;
#74573 = DIRECTION ( 'NONE',  ( -0.000000000000000000, 1.000000000000000000, -0.000000000000000000 ) ) ;
#74574 = CARTESIAN_POINT ( 'NONE',  ( -20.77875734969026311, 5.356774720514426491, 27.45402280011862217 ) ) ;
#74575 = CARTESIAN_POINT ( 'NONE',  ( 8.221391366598689743, 17.94232518691122635, 11.49999999999999645 ) ) ;
#74576 = DIRECTION ( 'NONE',  ( -0.000000000000000000, -0.000000000000000000, -1.000000000000000000 ) ) ;
#74577 = CARTESIAN_POINT ( 'NONE',  ( -119.5228709571500758, -24.65952944569305316, 1.056160979905705899 ) ) ;
#74578 = EDGE_LOOP ( 'NONE', ( #25466, #15735, #68909, #72908 ) ) ;
#74579 = CARTESIAN_POINT ( 'NONE',  ( 22.02124265030973760, 6.143225279485574397, 18.45402280011862217 ) ) ;
#74580 = CARTESIAN_POINT ( 'NONE',  ( -28.79528301136424417, -24.60093966666663690, 1.979581142082611489 ) ) ;
#74581 = CARTESIAN_POINT ( 'NONE',  ( -75.52287095715007581, -24.52323809116984776, 9.355190652339432589 ) ) ;
#74582 = CARTESIAN_POINT ( 'NONE',  ( -16.79864850723062020, -13.61054813162024679, 11.49999999999998934 ) ) ;
#74583 = CARTESIAN_POINT ( 'NONE',  ( -49.11088876609831289, -25.27518098729074225, 3.850711683794803886 ) ) ;
#74584 = CARTESIAN_POINT ( 'NONE',  ( 4.481524277812761525, 18.85844072219565604, -1.500000000000002220 ) ) ;
#74585 = LINE ( 'NONE', #11683, #78872 ) ;
#74586 = CARTESIAN_POINT ( 'NONE',  ( -80.85468212908030239, -25.05082048915169679, 7.526967310880902318 ) ) ;
#74587 = CARTESIAN_POINT ( 'NONE',  ( 18.24360591643979035, -7.691401616277519615, 11.49999999999998934 ) ) ;
#74588 = VERTEX_POINT ( 'NONE', #51882 ) ;
#74589 = CARTESIAN_POINT ( 'NONE',  ( -13.42616926349082895, -15.17935092467416069, 11.49999999999999645 ) ) ;
#74590 = CARTESIAN_POINT ( 'NONE',  ( 10.70203014590133783, 5.295085572968130094, -27.33604350180555187 ) ) ;
#74591 = CIRCLE ( 'NONE', #30847, 91.74549126261076992 ) ;
#74592 = B_SPLINE_CURVE_WITH_KNOTS ( 'NONE', 3,
 ( #56474, #70174, #54455, #16884, #31606, #23474, #55969, #71686 ),
 .UNSPECIFIED., .F., .F.,
 ( 4, 2, 2, 4 ),
 ( -0.001240355328176780516, -0.0002398155169398910602, 0.0007607242942969983952, 0.002761803916770777523 ),
 .UNSPECIFIED. ) ;
#74593 = CARTESIAN_POINT ( 'NONE',  ( 5.654014271574485662, -5.876774720514419847, 20.92503208403226722 ) ) ;
#74594 = ORIENTED_EDGE ( 'NONE', *, *, #71317, .T. ) ;
#74595 = CARTESIAN_POINT ( 'NONE',  ( -99.52764846858842418, -25.26416398485831749, 3.999772271414141489 ) ) ;
#74596 = CARTESIAN_POINT ( 'NONE',  ( 33.55334901790278224, 3.914284326356132659, -11.46592497341461758 ) ) ;
#74597 = CARTESIAN_POINT ( 'NONE',  ( -44.62287095715005592, -24.51283580621362646, 0.6167428607019806996 ) ) ;
#74598 = CARTESIAN_POINT ( 'NONE',  ( -95.62287095715005592, -23.48783264082479150, -1.443836473390061936 ) ) ;
#74599 = CARTESIAN_POINT ( 'NONE',  ( -31.52287095715006870, -23.72773821059535848, 11.05748984161097503 ) ) ;
#74600 = CARTESIAN_POINT ( 'NONE',  ( 3.179702300980958185, 19.78100630842630281, 11.49999999999998934 ) ) ;
#74601 = DIRECTION ( 'NONE',  ( -0.6599726524652352877, 0.000000000000000000, 0.7512896232465892110 ) ) ;
#74602 = EDGE_LOOP ( 'NONE', ( #65718, #60439, #97225, #8380 ) ) ;
#74603 = AXIS2_PLACEMENT_3D ( 'NONE', #55713, #39470, #46088 ) ;
#74604 = FACE_OUTER_BOUND ( 'NONE', #96250, .T. ) ;
#74605 = CARTESIAN_POINT ( 'NONE',  ( 2.100208336950355914, 0.000000000000000000, 1.249999999999996003 ) ) ;
#74606 = CARTESIAN_POINT ( 'NONE',  ( -51.52287095715006870, -24.64898659630367206, 1.056161002820821038 ) ) ;
#74607 = VECTOR ( 'NONE', #52156, 1000.000000000000114 ) ;
#74608 = DIRECTION ( 'NONE',  ( -1.226388327005079762E-16, 0.000000000000000000, 1.000000000000000000 ) ) ;
#74609 = CIRCLE ( 'NONE', #97296, 1.000000000000000000 ) ;
#74610 = LINE ( 'NONE', #6604, #96439 ) ;
#74611 = DIRECTION ( 'NONE',  ( 0.000000000000000000, 0.000000000000000000, 1.000000000000000000 ) ) ;
#74612 = ORIENTED_EDGE ( 'NONE', *, *, #75245, .F. ) ;
#74613 = EDGE_CURVE ( 'NONE', #14296, #81702, #83803, .T. ) ;
#74614 = CARTESIAN_POINT ( 'NONE',  ( 13.61570878652767291, 15.11107311891478666, 11.49999999999998934 ) ) ;
#74616 = EDGE_CURVE ( 'NONE', #44958, #54031, #5193, .T. ) ;
#74615 = ORIENTED_EDGE ( 'NONE', *, *, #87184, .T. ) ;
#74617 = CARTESIAN_POINT ( 'NONE',  ( 15.56936346670522120, 16.85858822313069894, 11.49999999999998934 ) ) ;
#74618 = DIRECTION ( 'NONE',  ( 0.000000000000000000, -0.9999999999976377785, -2.173523156925979128E-06 ) ) ;
#74619 = EDGE_CURVE ( 'NONE', #10895, #234, #75690, .T. ) ;
#74620 = ORIENTED_EDGE ( 'NONE', *, *, #37587, .T. ) ;
#74621 = CARTESIAN_POINT ( 'NONE',  ( -42.62287095715004881, -23.48786465467240347, 11.44779295918255180 ) ) ;
#74622 = EDGE_CURVE ( 'NONE', #10305, #70795, #99024, .T. ) ;
#74623 = CARTESIAN_POINT ( 'NONE',  ( -49.58282627629191808, -25.12215357654226011, 6.816471934855654169 ) ) ;
#74624 = CARTESIAN_POINT ( 'NONE',  ( -90.52287095715006160, -29.50249982740957577, 7.747779886224967605 ) ) ;
#74626 = ORIENTED_EDGE ( 'NONE', *, *, #32773, .T. ) ;
#74625 = CARTESIAN_POINT ( 'NONE',  ( -20.82729772986975547, -4.079710536234080642, 11.49999999999999645 ) ) ;
#74627 = ORIENTED_EDGE ( 'NONE', *, *, #14238, .F. ) ;
#74628 = CARTESIAN_POINT ( 'NONE',  ( -21.91774099701738621, 3.392077650570975766, -1.500000000000002220 ) ) ;
#74629 = CARTESIAN_POINT ( 'NONE',  ( 7.647619880454145758, 19.11525441646967849, -1.500000000000002220 ) ) ;
#74630 = ORIENTED_EDGE ( 'NONE', *, *, #29836, .F. ) ;
#74631 = ORIENTED_EDGE ( 'NONE', *, *, #2836, .T. ) ;
#74632 = LINE ( 'NONE', #97958, #31684 ) ;
#74633 = EDGE_CURVE ( 'NONE', #90630, #17609, #90928, .T. ) ;
#74634 = PLANE ( 'NONE',  #6 ) ;
#74635 = ORIENTED_EDGE ( 'NONE', *, *, #20672, .T. ) ;
#74636 = ORIENTED_EDGE ( 'NONE', *, *, #71447, .F. ) ;
#74637 = ORIENTED_EDGE ( 'NONE', *, *, #79580, .F. ) ;
#74638 = CARTESIAN_POINT ( 'NONE',  ( -83.62287095715002749, -24.51283580621364777, 0.6167428607019832532 ) ) ;
#74639 = CARTESIAN_POINT ( 'NONE',  ( 3.252401863874210264, 5.965225279485592225, -29.35688408629928858 ) ) ;
#74640 = CARTESIAN_POINT ( 'NONE',  ( 15.35137209921566992, -4.335618847589873148, -28.31916638425216348 ) ) ;
#74641 = CARTESIAN_POINT ( 'NONE',  ( 20.74337371777590278, 0.4424840333690017724, -1.500000000000002220 ) ) ;
#74642 = CARTESIAN_POINT ( 'NONE',  ( -21.72135255055207281, 0.4632500610043824851, 11.49999999999999645 ) ) ;
#74643 = ORIENTED_EDGE ( 'NONE', *, *, #99121, .F. ) ;
#74644 = CARTESIAN_POINT ( 'NONE',  ( -39.45263493068827643, -25.26937817949567133, 4.062928063294833692 ) ) ;
#74645 = CARTESIAN_POINT ( 'NONE',  ( -34.58953762381673869, -23.47596703998600276, 11.44779298504227505 ) ) ;
#74646 = CARTESIAN_POINT ( 'NONE',  ( -82.52287095715006160, -23.48786465467241058, 11.44779295918254469 ) ) ;
#74647 = CARTESIAN_POINT ( 'NONE',  ( -3.561414601982806349, 22.15502443119318343, -1.500000000000002220 ) ) ;
#74648 = CARTESIAN_POINT ( 'NONE',  ( -50.88361436997121245, -25.31296737229286009, 4.608108779064076899 ) ) ;
#74649 = CARTESIAN_POINT ( 'NONE',  ( -65.53968771207756561, -24.63355581998386867, 0.9682620441943842193 ) ) ;
#74650 = ORIENTED_EDGE ( 'NONE', *, *, #51601, .T. ) ;
#74651 = CARTESIAN_POINT ( 'NONE',  ( -98.52287095715006160, -24.50321055353803956, 9.387540953477515160 ) ) ;
#74652 = CARTESIAN_POINT ( 'NONE',  ( 11.96746718618548577, -4.832654890647344104, -27.30666805081000348 ) ) ;
#74653 = ORIENTED_EDGE ( 'NONE', *, *, #46115, .F. ) ;
#74654 = ORIENTED_EDGE ( 'NONE', *, *, #93858, .F. ) ;
#74655 = AXIS2_PLACEMENT_3D ( 'NONE', #79774, #9767, #41739 ) ;
#74656 = CARTESIAN_POINT ( 'NONE',  ( -46.56050914129246365, -23.73791477778911840, 11.05961554403171299 ) ) ;
#74657 = ORIENTED_EDGE ( 'NONE', *, *, #2261, .T. ) ;
#74658 = CARTESIAN_POINT ( 'NONE',  ( 11.00477826368897283, 18.22718707545001138, -1.500000000000002220 ) ) ;
#74659 = B_SPLINE_CURVE_WITH_KNOTS ( 'NONE', 3,
 ( #40390, #85048, #1832, #7927, #17040, #55118 ),
 .UNSPECIFIED., .F., .F.,
 ( 4, 2, 4 ),
 ( 6.384118678608765745E-06, 0.001386860460828371082, 0.002767336802978133652 ),
 .UNSPECIFIED. ) ;
#74660 = ORIENTED_EDGE ( 'NONE', *, *, #86185, .T. ) ;
#74661 = CARTESIAN_POINT ( 'NONE',  ( -5.912814555383966386, -5.876774720514418071, 20.28973052848695602 ) ) ;
#74662 = CARTESIAN_POINT ( 'NONE',  ( 21.44370820036873937, 4.193779532373530294, -1.500000000000002220 ) ) ;
#74663 = CARTESIAN_POINT ( 'NONE',  ( -32.62287095715004881, -29.50248528299804818, 1.056150453629029817 ) ) ;
#74664 = CARTESIAN_POINT ( 'NONE',  ( -7.973561950239375307, 21.24132968703115765, -1.500000000000002220 ) ) ;
#74665 = DIRECTION ( 'NONE',  ( -1.000000000000000000, 0.000000000000000000, 0.000000000000000000 ) ) ;
#74666 = DIRECTION ( 'NONE',  ( -1.334402673828313093E-16, 0.000000000000000000, -1.000000000000000000 ) ) ;
#74667 = CARTESIAN_POINT ( 'NONE',  ( -16.46405638241306946, -14.47283864684382237, -1.500000000000002220 ) ) ;
#74668 = CARTESIAN_POINT ( 'NONE',  ( -87.50770710757781501, -24.34968618360934656, 0.1864209137778970737 ) ) ;
#74669 = ORIENTED_EDGE ( 'NONE', *, *, #40250, .T. ) ;
#74670 = CARTESIAN_POINT ( 'NONE',  ( -40.13634460731591957, -25.29441190524739369, 5.523624973409209993 ) ) ;
#74671 = CARTESIAN_POINT ( 'NONE',  ( -28.98875734969026041, -6.376774720514426953, 0.7300228001186309656 ) ) ;
#74672 = ORIENTED_EDGE ( 'NONE', *, *, #59623, .T. ) ;
#74673 = EDGE_CURVE ( 'NONE', #11637, #56992, #29521, .T. ) ;
#74674 = CARTESIAN_POINT ( 'NONE',  ( -84.62911920018937906, -24.35071581493543391, 9.817618358456027039 ) ) ;
#74675 = AXIS2_PLACEMENT_3D ( 'NONE', #8298, #6792, #45869 ) ;
#74676 = CARTESIAN_POINT ( 'NONE',  ( -130.5728709571500303, -24.75179208683297816, 8.640809912072070276 ) ) ;
#74677 = AXIS2_PLACEMENT_3D ( 'NONE', #7993, #16597, #39948 ) ;
#74678 = CARTESIAN_POINT ( 'NONE',  ( -20.46794915382770341, -22.99521002796696934, -0.9709657327914291702 ) ) ;
#74679 = CARTESIAN_POINT ( 'NONE',  ( 9.380127297304197143, -19.07726845333505494, 11.49999999999998934 ) ) ;
#74680 = CARTESIAN_POINT ( 'NONE',  ( -55.62287095715007723, -24.52323809116985487, 9.355190652339427260 ) ) ;
#74681 = CARTESIAN_POINT ( 'NONE',  ( -26.55847933594999333, -24.97064538767926933, 2.904079897768723661 ) ) ;
#74682 = EDGE_CURVE ( 'NONE', #7353, #14136, #35657, .T. ) ;
#74683 = CARTESIAN_POINT ( 'NONE',  ( -85.54663212275447393, -24.52300882791530157, 0.6510814631126307095 ) ) ;
#74684 = LINE ( 'NONE', #82795, #28126 ) ;
#74685 = CARTESIAN_POINT ( 'NONE',  ( -117.5566936961534310, -23.73791477778912551, 11.05961554403169878 ) ) ;
#74686 = EDGE_LOOP ( 'NONE', ( #10849, #82142, #59174, #42409 ) ) ;
#74687 = CARTESIAN_POINT ( 'NONE',  ( -4.924063254364682507, -18.92933890202812464, 11.49999999999999645 ) ) ;
#74688 = CARTESIAN_POINT ( 'NONE',  ( -78.52287095715006160, -24.51387760970723662, 9.387446482453398744 ) ) ;
#74689 = CARTESIAN_POINT ( 'NONE',  ( -73.62287095715005592, -29.50247984919015209, -1.443849546365055359 ) ) ;
#74690 = ORIENTED_EDGE ( 'NONE', *, *, #94246, .T. ) ;
#74691 = PLANE ( 'NONE',  #83062 ) ;
#74692 = CARTESIAN_POINT ( 'NONE',  ( -44.52287095715006160, -24.65952944569303895, 1.056160979905691910 ) ) ;
#74693 = CARTESIAN_POINT ( 'NONE',  ( -26.49999761102944618, -24.66668825682660326, 7.831587328706810958 ) ) ;
#74694 = CARTESIAN_POINT ( 'NONE',  ( -106.5228709571500332, -24.51283580621365843, 0.6167428607019763698 ) ) ;
#74695 = CARTESIAN_POINT ( 'NONE',  ( 11.96684523812195700, 15.63349346248531546, -1.500000000000002220 ) ) ;
#74696 = ORIENTED_EDGE ( 'NONE', *, *, #13406, .F. ) ;
#74697 = DIRECTION ( 'NONE',  ( -3.773278334453079030E-23, 0.9999999999976377785, 2.173523156925979128E-06 ) ) ;
#74698 = DIRECTION ( 'NONE',  ( -1.000000000000000000, -0.000000000000000000, -0.000000000000000000 ) ) ;
#74699 = APPLICATION_PROTOCOL_DEFINITION ( 'international standard', 'config_control_design', 1994, #2559 ) ;
#74700 = ORIENTED_EDGE ( 'NONE', *, *, #3614, .T. ) ;
#74701 = CARTESIAN_POINT ( 'NONE',  ( 8.971512145086501633, -0.9869079657328782007, 3.741933919974615552 ) ) ;
#74702 = CARTESIAN_POINT ( 'NONE',  ( -20.27875734969026311, -6.143225279485574397, 26.25402280011862288 ) ) ;
#74703 = CARTESIAN_POINT ( 'NONE',  ( -47.49417500838666939, -24.34968618360933590, 0.1864209137778879144 ) ) ;
#74704 = CARTESIAN_POINT ( 'NONE',  ( -118.5578086755916871, -23.48783264082477018, -1.443836473390085695 ) ) ;
#74705 = CARTESIAN_POINT ( 'NONE',  ( 5.402409956206937203, -6.376774720514424288, 21.18719775722114917 ) ) ;
#74706 = CARTESIAN_POINT ( 'NONE',  ( 9.940598223437573822, -6.376774720514426953, 21.78128695274315874 ) ) ;
#74707 = CARTESIAN_POINT ( 'NONE',  ( -107.5534875950873186, -24.15543982623908192, -0.2315651400026443874 ) ) ;
#74708 = CARTESIAN_POINT ( 'NONE',  ( 0.05828707793547563409, -19.95834144014285272, -1.500000000000002220 ) ) ;
#74709 = CARTESIAN_POINT ( 'NONE',  ( -8.160000000000000142, -10.65233964170348635, 1.211157557776864291 ) ) ;
#74710 = CARTESIAN_POINT ( 'NONE',  ( -0.05362039087632652912, -22.35584190302588681, 9.068352157775928291 ) ) ;
#74711 = VERTEX_POINT ( 'NONE', #59000 ) ;
#74712 = DIRECTION ( 'NONE',  ( -0.000000000000000000, -0.000000000000000000, -1.000000000000000000 ) ) ;
#74713 = CARTESIAN_POINT ( 'NONE',  ( 13.02836919244612623, -3.777199458296179646, -28.16488413836729521 ) ) ;
#74714 = B_SPLINE_CURVE_WITH_KNOTS ( 'NONE', 3,
 ( #89360, #12219, #19828, #5617 ),
 .UNSPECIFIED., .F., .F.,
 ( 4, 4 ),
 ( 0.000000000000000000, 1.000000000000000000 ),
 .UNSPECIFIED. ) ;
#74715 = SHAPE_REPRESENTATION_RELATIONSHIP ( 'NONE' , 'NONE' ,  #60715, #13793 ) ;
#74716 = CARTESIAN_POINT ( 'NONE',  ( -80.63529280476316785, -24.40133493613050319, 9.663955038902802386 ) ) ;
#74717 = CARTESIAN_POINT ( 'NONE',  ( -125.2170126610060947, -25.23515688875662732, 6.311387300439234238 ) ) ;
#74718 = CARTESIAN_POINT ( 'NONE',  ( -81.59562872226922536, -23.96119346886881019, -0.6495511937831893734 ) ) ;
#74719 = VECTOR ( 'NONE', #53375, 1000.000000000000000 ) ;
#74720 = DIRECTION ( 'NONE',  ( -3.773278334453079030E-23, 0.9999999999976377785, 2.173523156925979128E-06 ) ) ;
#74721 = CARTESIAN_POINT ( 'NONE',  ( -1.568769572606061535, -5.876774720514415407, 19.76359802465961835 ) ) ;
#74722 = ORIENTED_EDGE ( 'NONE', *, *, #93866, .F. ) ;
#74723 = CARTESIAN_POINT ( 'NONE',  ( -37.62287095715003460, -24.33927499327853639, 9.819080762295815390 ) ) ;
#74724 = CARTESIAN_POINT ( 'NONE',  ( 6.132272708306365949, -6.376774720514424288, 21.80683391321003839 ) ) ;
#74725 = ORIENTED_EDGE ( 'NONE', *, *, #86242, .T. ) ;
#74726 = EDGE_CURVE ( 'NONE', #49130, #59761, #50916, .T. ) ;
#74727 = CARTESIAN_POINT ( 'NONE',  ( 15.52975653788041122, 12.98207780544785628, 11.49999999999998934 ) ) ;
#74728 = CARTESIAN_POINT ( 'NONE',  ( -69.00130780607547365, -25.29264792232144643, 5.753730642603843926 ) ) ;
#74729 = CARTESIAN_POINT ( 'NONE',  ( -129.6228709571499280, -23.94994826722565406, -0.6494450866342679207 ) ) ;
#74730 = EDGE_CURVE ( 'NONE', #733, #49698, #53439, .T. ) ;
#74731 = DIRECTION ( 'NONE',  ( -0.9762960071199348056, -0.2164396139380965756, -4.956352788505166226E-16 ) ) ;
#74732 = ADVANCED_FACE ( 'NONE', ( #46763 ), #41376, .T. ) ;
#74733 = EDGE_LOOP ( 'NONE', ( #54884, #61450 ) ) ;
#74734 = CARTESIAN_POINT ( 'NONE',  ( -79.00053288248066963, -25.30543024437582034, 5.507749646993243431 ) ) ;
#74735 = CARTESIAN_POINT ( 'NONE',  ( -6.499999999999993783, 3.000000000000000000, 4.499999999999999112 ) ) ;
#74736 = VECTOR ( 'NONE', #96183, 1000.000000000000000 ) ;
#74737 = CARTESIAN_POINT ( 'NONE',  ( -16.72505113720834657, 11.10480813184383742, -1.500000000000002220 ) ) ;
#74738 = B_SPLINE_CURVE_WITH_KNOTS ( 'NONE', 3,
 ( #85356, #98584, #37199, #14341 ),
 .UNSPECIFIED., .F., .F.,
 ( 4, 4 ),
 ( 0.7192904550652682305, 0.7202912021060337011 ),
 .UNSPECIFIED. ) ;
#74739 = ADVANCED_FACE ( 'NONE', ( #34045 ), #57899, .F. ) ;
#74740 = CARTESIAN_POINT ( 'NONE',  ( -18.19455084753484542, -10.52586660885228298, 11.49999999999999645 ) ) ;
#74741 = CARTESIAN_POINT ( 'NONE',  ( 2.899999999999999467, 33.29999999999999716, 2.100000000000000089 ) ) ;
#74742 = CARTESIAN_POINT ( 'NONE',  ( -70.50643210755447399, -24.15602025860895807, 10.28564288303535967 ) ) ;
#74743 = CARTESIAN_POINT ( 'NONE',  ( -17.89045161427552699, -12.92718102017995641, 11.49999999999998934 ) ) ;
#74744 = EDGE_CURVE ( 'NONE', #100315, #87641, #96925, .T. ) ;
#74745 = CARTESIAN_POINT ( 'NONE',  ( -39.44687923781921057, -25.31589135549187120, 4.188173601291640402 ) ) ;
#74746 = B_SPLINE_CURVE_WITH_KNOTS ( 'NONE', 3,
 ( #65668, #78844, #57547, #86969 ),
 .UNSPECIFIED., .F., .F.,
 ( 4, 4 ),
 ( 0.000000000000000000, 0.0001007156686975780100 ),
 .UNSPECIFIED. ) ;
#74747 = CARTESIAN_POINT ( 'NONE',  ( -47.62287095715004881, -24.50216790748205398, 0.6166512839542470648 ) ) ;
#74748 = DIRECTION ( 'NONE',  ( 0.000000000000000000, 0.000000000000000000, 1.000000000000000000 ) ) ;
#74749 = ORIENTED_EDGE ( 'NONE', *, *, #91528, .T. ) ;
#74750 = DIRECTION ( 'NONE',  ( 0.000000000000000000, 0.000000000000000000, 1.000000000000000000 ) ) ;
#74751 = CARTESIAN_POINT ( 'NONE',  ( -31.58039431984602885, -24.51314013834316086, 0.6176544820404139546 ) ) ;
#74752 = ORIENTED_EDGE ( 'NONE', *, *, #94246, .F. ) ;
#74753 = ORIENTED_EDGE ( 'NONE', *, *, #11760, .T. ) ;
#74754 = CARTESIAN_POINT ( 'NONE',  ( -83.62287095715007013, -24.65952944569304606, 1.056160979905700792 ) ) ;
#74755 = CARTESIAN_POINT ( 'NONE',  ( 282.9764569301858046, 6.475225279485573360, 20.79159422840526616 ) ) ;
#74757 = EDGE_CURVE ( 'NONE', #24982, #14570, #11030, .T. ) ;
#74756 = CARTESIAN_POINT ( 'NONE',  ( -76.55011161496653926, -24.15543982623907482, -0.2315651400026599582 ) ) ;
#74758 = CARTESIAN_POINT ( 'NONE',  ( -6.092534927433182368, -19.63929903328317295, -1.500000000000002220 ) ) ;
#74759 = CARTESIAN_POINT ( 'NONE',  ( 16.61460563260716583, 13.71664681387569118, 11.49999999999999645 ) ) ;
#74760 = ORIENTED_EDGE ( 'NONE', *, *, #90211, .T. ) ;
#74761 = CARTESIAN_POINT ( 'NONE',  ( -91.62578869787175506, -24.51314013834316086, 0.6176544820404156200 ) ) ;
#74762 = FACE_OUTER_BOUND ( 'NONE', #66937, .T. ) ;
#74763 = CARTESIAN_POINT ( 'NONE',  ( 20.54922051473491607, -8.805037660420627077, 11.49999999999998934 ) ) ;
#74764 = CARTESIAN_POINT ( 'NONE',  ( 6.420673076923079314, -5.876774720514427841, 21.83974358974358765 ) ) ;
#74765 = CARTESIAN_POINT ( 'NONE',  ( 33.96422015159436114, -0.3587747205144265483, -7.233236000911337449 ) ) ;
#74766 = ORIENTED_EDGE ( 'NONE', *, *, #77612, .F. ) ;
#74767 = CARTESIAN_POINT ( 'NONE',  ( -40.49165087243459737, -29.50249503729891742, 5.543933732384023649 ) ) ;
#74768 = CARTESIAN_POINT ( 'NONE',  ( 3.036358173076929123, -5.876774720514420736, 20.87990785256409865 ) ) ;
#74769 = CARTESIAN_POINT ( 'NONE',  ( -17.14161228048114438, 11.91956482804130601, -1.500000000000002220 ) ) ;
#74770 = ORIENTED_EDGE ( 'NONE', *, *, #170, .F. ) ;
#74772 = ORIENTED_EDGE ( 'NONE', *, *, #91833, .F. ) ;
#74771 = CARTESIAN_POINT ( 'NONE',  ( -39.57784196604458771, -25.15646891919385908, 3.099756419313730138 ) ) ;
#74773 = ORIENTED_EDGE ( 'NONE', *, *, #5704, .F. ) ;
#74774 = AXIS2_PLACEMENT_3D ( 'NONE', #76401, #69304, #8904 ) ;
#74775 = CARTESIAN_POINT ( 'NONE',  ( -100.6235771386987778, -25.00182538069146787, 7.747789668545043362 ) ) ;
#74776 = CARTESIAN_POINT ( 'NONE',  ( -8.144517828999388698, 19.50133175306300970, -1.500000000000002220 ) ) ;
#74777 = EDGE_LOOP ( 'NONE', ( #43568, #98231, #81397 ) ) ;
#74778 = CARTESIAN_POINT ( 'NONE',  ( -117.5877662462894904, -24.65952944569305316, 1.056160979905706343 ) ) ;
#74779 = CARTESIAN_POINT ( 'NONE',  ( -71.52287095715007581, -29.50247984919015209, -1.443849546365055359 ) ) ;
#74780 = CARTESIAN_POINT ( 'NONE',  ( -121.6228709571500417, -23.48783264082478794, -1.443836473390058384 ) ) ;
#74781 = CARTESIAN_POINT ( 'NONE',  ( -76.50052754764180918, -24.51419770103157347, 9.386484678747176957 ) ) ;
#74782 = CARTESIAN_POINT ( 'NONE',  ( -49.17699911376700328, -25.22559820935306618, 3.608295678972204268 ) ) ;
#74783 = CARTESIAN_POINT ( 'NONE',  ( -19.76859095128058996, -9.124614402804876789, -1.500000000000002220 ) ) ;
#74784 = CARTESIAN_POINT ( 'NONE',  ( -81.14265914342044539, -25.24759757244822467, 6.882252479551046243 ) ) ;
#74786 = ORIENTED_EDGE ( 'NONE', *, *, #27283, .T. ) ;
#74785 = CARTESIAN_POINT ( 'NONE',  ( -22.12323335113916301, -3.008119206214963981, 11.49999999999999645 ) ) ;
#74787 = LINE ( 'NONE', #13885, #61592 ) ;
#74788 = CARTESIAN_POINT ( 'NONE',  ( -92.52287095715006160, -23.47596703998600631, 11.44779298504228393 ) ) ;
#74789 = EDGE_CURVE ( 'NONE', #9388, #62667, #46072, .T. ) ;
#74790 = CARTESIAN_POINT ( 'NONE',  ( 18.72495633783376334, -0.5000000000000000000, 2.346898003627108320 ) ) ;
#74791 = VERTEX_POINT ( 'NONE', #40660 ) ;
#74792 = VERTEX_POINT ( 'NONE', #97918 ) ;
#74793 = EDGE_CURVE ( 'NONE', #96596, #19596, #52178, .T. ) ;
#74794 = ORIENTED_EDGE ( 'NONE', *, *, #85854, .F. ) ;
#74795 = DIRECTION ( 'NONE',  ( 0.000000000000000000, 0.000000000000000000, 1.000000000000000000 ) ) ;
#74796 = VECTOR ( 'NONE', #4837, 1000.000000000000000 ) ;
#74797 = CARTESIAN_POINT ( 'NONE',  ( -114.6228709571500559, -24.66019654487199730, 8.947790411086122830 ) ) ;
#74798 = CARTESIAN_POINT ( 'NONE',  ( -78.94303308397306296, -25.03137954913951901, 5.977537200458097999 ) ) ;
#74799 = CARTESIAN_POINT ( 'NONE',  ( -68.52287095715006160, -29.50250243563736774, 8.947779886222143375 ) ) ;
#74800 = B_SPLINE_CURVE_WITH_KNOTS ( 'NONE', 3,
 ( #48932, #80372, #71767, #34701, #64678, #42333 ),
 .UNSPECIFIED., .F., .F.,
 ( 4, 2, 4 ),
 ( 0.000000000000000000, 0.001380901958385387677, 0.002761803916770775354 ),
 .UNSPECIFIED. ) ;
#74801 = DIRECTION ( 'NONE',  ( 0.000000000000000000, -2.173523156925980399E-06, 0.9999999999976378895 ) ) ;
#74802 = EDGE_CURVE ( 'NONE', #37700, #23800, #1902, .T. ) ;
#74803 = CARTESIAN_POINT ( 'NONE',  ( -38.52287095715009002, -23.94994826722564696, -0.6494450866342726947 ) ) ;
#74804 = ORIENTED_EDGE ( 'NONE', *, *, #79972, .F. ) ;
#74805 = CARTESIAN_POINT ( 'NONE',  ( 19.37663158793545293, -0.8356294931911363300, 11.49999999999999645 ) ) ;
#74806 = CARTESIAN_POINT ( 'NONE',  ( -115.5228709571500190, -24.52323809116983355, 9.355190652339423707 ) ) ;
#74807 = EDGE_CURVE ( 'NONE', #81557, #21450, #57025, .T. ) ;
#74808 = EDGE_LOOP ( 'NONE', ( #13307, #91651, #33593, #95370 ) ) ;
#74809 = CARTESIAN_POINT ( 'NONE',  ( 3.160575456146155204, -6.376774720514408301, 18.86877352677795372 ) ) ;
#74810 = CARTESIAN_POINT ( 'NONE',  ( 10.73283225838973642, 5.356774720506346732, -27.03068772369604744 ) ) ;
#74811 = FACE_OUTER_BOUND ( 'NONE', #28114, .T. ) ;
#74812 = CARTESIAN_POINT ( 'NONE',  ( 8.160000000000000142, -10.15233964170348457, 0.003711184059992174607 ) ) ;
#74813 = B_SPLINE_CURVE_WITH_KNOTS ( 'NONE', 3,
 ( #73239, #19437, #42310, #48404, #64653, #94561 ),
 .UNSPECIFIED., .F., .F.,
 ( 4, 2, 4 ),
 ( 0.000000000000000000, 0.001380764517854763014, 0.002761529035709526028 ),
 .UNSPECIFIED. ) ;
#74814 = VECTOR ( 'NONE', #29413, 1000.000000000000000 ) ;
#74815 = CARTESIAN_POINT ( 'NONE',  ( 19.11985901488480621, -4.296470200863222288, -1.500000000000002220 ) ) ;
#74816 = CARTESIAN_POINT ( 'NONE',  ( -37.62287095715005592, -24.64898659630367206, 1.056161002820819261 ) ) ;
#74818 = ORIENTED_EDGE ( 'NONE', *, *, #54648, .F. ) ;
#74817 = APPROVAL_PERSON_ORGANIZATION ( #27782, #21550, #58735 ) ;
#74819 = CARTESIAN_POINT ( 'NONE',  ( -14.38888013576714719, -16.06800976983558726, -1.500000000000002220 ) ) ;
#74820 = CARTESIAN_POINT ( 'NONE',  ( 10.45000000000000462, 1.999999999999998668, 19.19609335255483984 ) ) ;
#74821 = CARTESIAN_POINT ( 'NONE',  ( -70.32380231474228083, -25.12219144746705268, 7.101635560771297762 ) ) ;
#74822 = CARTESIAN_POINT ( 'NONE',  ( -44.62287095715004881, -29.50248528299804818, 1.056150453629031594 ) ) ;
#74823 = CARTESIAN_POINT ( 'NONE',  ( -10.24059822343757808, -6.376774720514426953, 17.91871304725684766 ) ) ;
#74824 = CARTESIAN_POINT ( 'NONE',  ( -11.38079350637645959, -19.95400817559217899, -1.500000000000002220 ) ) ;
#74825 = CC_DESIGN_PERSON_AND_ORGANIZATION_ASSIGNMENT ( #80326, #48386, ( #55421 ) ) ;
#74826 = SECURITY_CLASSIFICATION_LEVEL ( 'unclassified' ) ;
#74827 = CARTESIAN_POINT ( 'NONE',  ( 7.160000000000000142, 8.793627758918228565, -2.994553991265763049 ) ) ;
#74828 = CARTESIAN_POINT ( 'NONE',  ( -24.97666371003640151, 5.965225279485592225, -15.72894043976419098 ) ) ;
#74829 = CARTESIAN_POINT ( 'NONE',  ( -19.56588111578679090, -4.897929960003377658, 11.49999999999999645 ) ) ;
#74830 = CARTESIAN_POINT ( 'NONE',  ( -70.92287095715006728, -23.47593901973090169, -1.443836447538997536 ) ) ;
#74831 = CARTESIAN_POINT ( 'NONE',  ( -91.52287095715010423, -24.34917612406837861, 0.1852690917426554895 ) ) ;
#74832 = DIRECTION ( 'NONE',  ( 1.000000000000000000, 3.773278334444167608E-23, 8.201307833595939069E-29 ) ) ;
#74833 = DIRECTION ( 'NONE',  ( -0.000000000000000000, -0.000000000000000000, -1.000000000000000000 ) ) ;
#74834 = CARTESIAN_POINT ( 'NONE',  ( -31.23108706089061570, -23.47596703998600276, 11.44779298504227683 ) ) ;
#74835 = CARTESIAN_POINT ( 'NONE',  ( 1.822157996128044299, -19.77364354024053839, 11.49999999999998934 ) ) ;
#74836 = DIRECTION ( 'NONE',  ( 0.000000000000000000, -1.000000000000000000, 0.000000000000000000 ) ) ;
#74837 = CARTESIAN_POINT ( 'NONE',  ( -19.57314199983870751, -2.777824058246878280, -1.500000000000002220 ) ) ;
#74838 = CARTESIAN_POINT ( 'NONE',  ( -126.5549963774327580, -24.51419770103158058, 9.386484678747164523 ) ) ;
#74839 = DIRECTION ( 'NONE',  ( -3.773278334453080206E-23, 0.9999999999976377785, 2.173523156925979975E-06 ) ) ;
#74840 = CARTESIAN_POINT ( 'NONE',  ( 3.085011456917871264, -6.376774720514408301, 19.00082519311127172 ) ) ;
#74841 = CARTESIAN_POINT ( 'NONE',  ( 3.345817365282868217, 20.41450801592841557, 11.49999999999999645 ) ) ;
#74842 = CARTESIAN_POINT ( 'NONE',  ( -99.62287095715005592, -29.50250786944525672, 11.44777988621623166 ) ) ;
#74843 = CARTESIAN_POINT ( 'NONE',  ( -111.3776484685884327, -29.50249240399202222, 4.332395270848422797 ) ) ;
#74844 = CARTESIAN_POINT ( 'NONE',  ( -75.52287095715006160, -25.00158670708909625, 2.256160236439166411 ) ) ;
#74845 = CARTESIAN_POINT ( 'NONE',  ( 8.023449251107201974, -21.19570997880782670, 11.49999999999999645 ) ) ;
#74846 = ORIENTED_EDGE ( 'NONE', *, *, #5396, .F. ) ;
#74847 = B_SPLINE_SURFACE_WITH_KNOTS ( 'NONE', 3, 3, ( 
 ( #53695, #36954, #91237, #54198 ),
 ( #8001, #7500, #92233, #98843 ),
 ( #91732, #68903, #38949, #53193 ),
 ( #38452, #14609, #76497, #7004 ),
 ( #37951, #30335, #67922, #22706 ),
 ( #69904, #84623, #69407, #30840 ),
 ( #59811, #61806, #15608, #92726 ),
 ( #85122, #46573, #389, #83116 ),
 ( #21218, #13606, #24226, #41462 ),
 ( #85625, #40464, #9002, #18120 ) ),
 .UNSPECIFIED., .F., .F., .F.,
 ( 4, 3, 3, 4 ),
 ( 4, 4 ),
 ( 0.0004766839783816472268, 0.1491231665100170578, 0.2234464077758347711, 0.2977696490416524844 ),
 ( 0.5995664120385277851, 0.6009364153319428636 ),
 .UNSPECIFIED. ) ;
#74848 = CARTESIAN_POINT ( 'NONE',  ( -0.4453066574538939171, -5.876774720514410077, 19.14913681718892491 ) ) ;
#74849 = DIRECTION ( 'NONE',  ( 0.9903949459893287566, 0.09776975748869010108, -0.09776975748868974025 ) ) ;
#74850 = ADVANCED_FACE ( 'NONE', ( #96938 ), #89822, .F. ) ;
#74851 = DIRECTION ( 'NONE',  ( 1.000000000000000000, -0.000000000000000000, 0.000000000000000000 ) ) ;
#74852 = DIRECTION ( 'NONE',  ( -0.000000000000000000, -1.000000000000000000, -0.000000000000000000 ) ) ;
#74853 = ORIENTED_EDGE ( 'NONE', *, *, #88458, .F. ) ;
#74854 = EDGE_LOOP ( 'NONE', ( #66568, #5720, #26432, #92372 ) ) ;
#74855 = CARTESIAN_POINT ( 'NONE',  ( -99.96719126485838558, -25.13541771911171807, 7.029542260679920496 ) ) ;
#74856 = CARTESIAN_POINT ( 'NONE',  ( 22.85402955525884394, -0.1436109537974766814, -1.500000000000002220 ) ) ;
#74857 = CARTESIAN_POINT ( 'NONE',  ( -29.58660889787569914, -24.27033885141579006, 0.1864212292069159782 ) ) ;
#74858 = CARTESIAN_POINT ( 'NONE',  ( -5.754811884962036217, -20.78327508566754389, -1.500000000000002220 ) ) ;
#74859 = DIRECTION ( 'NONE',  ( 1.000000000000000000, 3.773278334444166432E-23, 8.201307841325785021E-29 ) ) ;
#74860 = CARTESIAN_POINT ( 'NONE',  ( -32.58953762381672448, -23.48783264082477729, -1.443836473390074371 ) ) ;
#74861 = EDGE_CURVE ( 'NONE', #82569, #24683, #97437, .T. ) ;
#74862 = CARTESIAN_POINT ( 'NONE',  ( -3.649967738973055376, -22.27025559232234642, 11.49999999999999645 ) ) ;
#74863 = VERTEX_POINT ( 'NONE', #52265 ) ;
#74864 = CARTESIAN_POINT ( 'NONE',  ( -88.62287095715004170, -29.50250243563736774, 8.947779886222139822 ) ) ;
#74865 = AXIS2_PLACEMENT_3D ( 'NONE', #84318, #43778, #36162 ) ;
#74866 = CARTESIAN_POINT ( 'NONE',  ( -10.95654650054425794, 19.06054500580150446, 11.49999999999998934 ) ) ;
#74867 = EDGE_CURVE ( 'NONE', #26640, #37802, #4919, .T. ) ;
#74868 = CARTESIAN_POINT ( 'NONE',  ( -64.52287095715009002, -23.94994826722565406, -0.6494450866342742490 ) ) ;
#74869 = FACE_OUTER_BOUND ( 'NONE', #84695, .T. ) ;
#74870 = VERTEX_POINT ( 'NONE', #35548 ) ;
#74871 = DIRECTION ( 'NONE',  ( 0.000000000000000000, 0.000000000000000000, 1.000000000000000000 ) ) ;
#74872 = CARTESIAN_POINT ( 'NONE',  ( -90.63292611122409426, -24.40133493613050675, 9.663955038902805939 ) ) ;
#74873 = VERTEX_POINT ( 'NONE', #6080 ) ;
#74874 = CARTESIAN_POINT ( 'NONE',  ( -29.52287095715007581, -24.42901175215209619, 0.6166258780728530731 ) ) ;
#74875 = ORIENTED_EDGE ( 'NONE', *, *, #20547, .F. ) ;
#74876 = ORIENTED_EDGE ( 'NONE', *, *, #8305, .F. ) ;
#74877 = CARTESIAN_POINT ( 'NONE',  ( -111.5228709571500616, -23.47596703998600631, 11.44779298504228038 ) ) ;
#74878 = CARTESIAN_POINT ( 'NONE',  ( -27.25988310792305214, -0.3587747205144265483, 30.32664379231667695 ) ) ;
#74880 = EDGE_CURVE ( 'NONE', #74873, #72523, #89387, .T. ) ;
#74879 = CARTESIAN_POINT ( 'NONE',  ( -36.60105005485234386, -23.96119346886880663, -0.6495511937832127991 ) ) ;
#74881 = CARTESIAN_POINT ( 'NONE',  ( -19.81292649638395531, 4.959676026661640869, -1.500000000000002220 ) ) ;
#74882 = VERTEX_POINT ( 'NONE', #36033 ) ;
#74883 = DIRECTION ( 'NONE',  ( 1.000000000000000000, 3.491481338843133355E-15, 2.352173255807796056E-16 ) ) ;
#74884 = CARTESIAN_POINT ( 'NONE',  ( -92.52287095715009002, -24.66019654487200086, 8.947790411086115725 ) ) ;
#74886 = CARTESIAN_POINT ( 'NONE',  ( -105.5960322518042176, -23.85016227208580730, -0.8807180028928328630 ) ) ;
#74885 = AXIS2_PLACEMENT_3D ( 'NONE', #99988, #83285, #21374 ) ;
#74887 = CARTESIAN_POINT ( 'NONE',  ( -81.42380231474228935, -25.31401921878147832, 5.197788989978542773 ) ) ;
#74888 = ORIENTED_EDGE ( 'NONE', *, *, #13121, .T. ) ;
#74889 = B_SPLINE_CURVE_WITH_KNOTS ( 'NONE', 3,
 ( #55905, #87843, #74115, #66532 ),
 .UNSPECIFIED., .F., .F.,
 ( 4, 4 ),
 ( 0.000000000000000000, 0.0001000000000000028644 ),
 .UNSPECIFIED. ) ;
#74890 = CARTESIAN_POINT ( 'NONE',  ( 22.81105451610979173, 1.477225279485574028, -18.46691820600746681 ) ) ;
#74891 = CARTESIAN_POINT ( 'NONE',  ( -94.55620429048340725, -23.47593901973091235, -1.443836447539002865 ) ) ;
#74892 = CC_DESIGN_SECURITY_CLASSIFICATION ( #65234, ( #55421 ) ) ;
#74893 = CARTESIAN_POINT ( 'NONE',  ( 19.40640353424967302, -7.489167304209242815, -1.500000000000002220 ) ) ;
#74894 = ORIENTED_EDGE ( 'NONE', *, *, #36502, .F. ) ;
#74896 = ORIENTED_EDGE ( 'NONE', *, *, #61948, .F. ) ;
#74895 = DIRECTION ( 'NONE',  ( 0.000000000000000000, 0.000000000000000000, -1.000000000000000000 ) ) ;
#74897 = CARTESIAN_POINT ( 'NONE',  ( -68.52287095715004739, -24.50321055353805733, 9.387540953477525818 ) ) ;
#74898 = CARTESIAN_POINT ( 'NONE',  ( -8.160000000000000142, -9.652339641703484574, 1.560255187525485976 ) ) ;
#74899 = EDGE_LOOP ( 'NONE', ( #94847, #45922, #46332, #52295 ) ) ;
#74900 = EDGE_LOOP ( 'NONE', ( #10802, #34951 ) ) ;
#74901 = CARTESIAN_POINT ( 'NONE',  ( -29.49875734969026198, 0.3587747205144265483, 2.362022800118626531 ) ) ;
#74902 = CARTESIAN_POINT ( 'NONE',  ( -116.4728709570019873, -25.30556170156494744, 4.804051544042277300 ) ) ;
#74903 = CARTESIAN_POINT ( 'NONE',  ( -60.52287095715006160, -23.48786465467241058, 11.44779295918254824 ) ) ;
#74904 = CARTESIAN_POINT ( 'NONE',  ( -71.30457154551152144, -25.31201785239418456, 6.209207263561717483 ) ) ;
#74906 = EDGE_LOOP ( 'NONE', ( #31185, #99457, #37100, #64197 ) ) ;
#74905 = CARTESIAN_POINT ( 'NONE',  ( 20.51613352552997327, 8.347415244503286758, 11.49999999999999645 ) ) ;
#74907 = CARTESIAN_POINT ( 'NONE',  ( -88.88918693012689687, -25.26877915520014639, 5.947789088310639904 ) ) ;
#74908 = CARTESIAN_POINT ( 'NONE',  ( 22.24477432615492134, 4.004077059304647968, -1.500000000000002220 ) ) ;
#74910 = ORIENTED_EDGE ( 'NONE', *, *, #86747, .T. ) ;
#74909 = CARTESIAN_POINT ( 'NONE',  ( -115.5889401794561024, -24.63419186844613051, 9.035850630976923981 ) ) ;
#74911 = EDGE_CURVE ( 'NONE', #25435, #84515, #83614, .T. ) ;
#74912 = ORIENTED_EDGE ( 'NONE', *, *, #52871, .T. ) ;
#74913 = CARTESIAN_POINT ( 'NONE',  ( 14.76093561896378326, 3.316774720514426456, -26.55548769130088260 ) ) ;
#74914 = EDGE_CURVE ( 'NONE', #44615, #30450, #4096, .T. ) ;
#74915 = AXIS2_PLACEMENT_3D ( 'NONE', #61838, #93261, #77532 ) ;
#74916 = CARTESIAN_POINT ( 'NONE',  ( -78.62287095715005592, -24.64965695001468404, 8.947790433994182280 ) ) ;
#74917 = VERTEX_POINT ( 'NONE', #67494 ) ;
#74918 = DIRECTION ( 'NONE',  ( -1.000000000000000000, -0.000000000000000000, -0.000000000000000000 ) ) ;
#74919 = CARTESIAN_POINT ( 'NONE',  ( 2.321567282091853812, -22.14299765706108403, -1.500000000000002220 ) ) ;
#74920 = DIRECTION ( 'NONE',  ( -1.000000000000000000, -0.000000000000000000, -0.000000000000000000 ) ) ;
#74921 = ORIENTED_EDGE ( 'NONE', *, *, #95204, .F. ) ;
#74922 = CARTESIAN_POINT ( 'NONE',  ( -5.000686017310577824, -6.376774720514411854, 19.46274624311237034 ) ) ;
#74923 = CARTESIAN_POINT ( 'NONE',  ( -81.32299058106391954, -25.08345032616901094, 7.319022766874549113 ) ) ;
#74924 = CARTESIAN_POINT ( 'NONE',  ( -25.63723411449804246, -24.85022734580098458, 3.654579668448656005 ) ) ;
#74925 = CARTESIAN_POINT ( 'NONE',  ( -103.5228709571500758, -23.72773821059536203, 11.05748984161097326 ) ) ;
#74926 = LINE ( 'NONE', #99269, #95814 ) ;
#74927 = CARTESIAN_POINT ( 'NONE',  ( -1.849579639615634097, -19.42000222497389927, -1.500000000000002220 ) ) ;
#74928 = AXIS2_PLACEMENT_3D ( 'NONE', #73846, #29162, #52511 ) ;
#74929 = CARTESIAN_POINT ( 'NONE',  ( -11.48222599368078889, -18.13851731312990267, -1.500000000000002220 ) ) ;
#74930 = CARTESIAN_POINT ( 'NONE',  ( -2.772696838893043747, -5.876774720514411854, 19.95463486386180207 ) ) ;
#74931 = PLANE ( 'NONE',  #36743 ) ;
#74932 = CARTESIAN_POINT ( 'NONE',  ( -65.52287095715006160, -25.00182538069144655, 7.747789668545101982 ) ) ;
#74933 = CARTESIAN_POINT ( 'NONE',  ( 22.80427751693360960, 0.003464389817739472934, -1.500000000000002220 ) ) ;
#74934 = ADVANCED_FACE ( 'NONE', ( #12689 ), #66518, .F. ) ;
#74935 = EDGE_CURVE ( 'NONE', #38058, #70059, #68316, .T. ) ;
#74936 = PERSON_AND_ORGANIZATION_ROLE ( 'creator' ) ;
#74937 = DIRECTION ( 'NONE',  ( 0.000000000000000000, -1.000000000000000000, 0.000000000000000000 ) ) ;
#74938 = CARTESIAN_POINT ( 'NONE',  ( -125.5228709571500616, -23.48783264083375144, -1.443836473376139740 ) ) ;
#74939 = CARTESIAN_POINT ( 'NONE',  ( -19.26508835251014773, 5.270845654819066084, 11.49999999999999645 ) ) ;
#74940 = CARTESIAN_POINT ( 'NONE',  ( -50.52287095715007581, -24.15431212366388891, -0.2830839119429292561 ) ) ;
#74941 = CARTESIAN_POINT ( 'NONE',  ( -74.62362437411805161, -24.66019654487199730, 8.947790411086108620 ) ) ;
#74942 = CARTESIAN_POINT ( 'NONE',  ( -108.6228709571500559, -23.47593901973091235, -1.443836447538999312 ) ) ;
#74943 = ORIENTED_EDGE ( 'NONE', *, *, #60389, .F. ) ;
#74944 = CARTESIAN_POINT ( 'NONE',  ( -69.62287095715005592, -29.50250243563736774, 8.947779886222143375 ) ) ;
#74945 = CARTESIAN_POINT ( 'NONE',  ( -92.62287095715005592, -24.65952944569304606, 1.056160979905700348 ) ) ;
#74946 = CARTESIAN_POINT ( 'NONE',  ( -17.03913561245058261, -13.47071831616118942, 11.49999999999998934 ) ) ;
#74947 = EDGE_CURVE ( 'NONE', #55598, #59310, #69975, .T. ) ;
#74948 = CARTESIAN_POINT ( 'NONE',  ( -37.55620429048340014, -23.47593901973091235, -1.443836447539011525 ) ) ;
#74949 = CARTESIAN_POINT ( 'NONE',  ( 19.50827032651345405, -1.201405007418623994, -1.500000000000002220 ) ) ;
#74950 = EDGE_CURVE ( 'NONE', #55465, #39871, #44649, .T. ) ;
#74951 = LINE ( 'NONE', #90692, #21504 ) ;
#74952 = VECTOR ( 'NONE', #50759, 1000.000000000000000 ) ;
#74953 = ORIENTED_EDGE ( 'NONE', *, *, #96604, .T. ) ;
#74955 = EDGE_CURVE ( 'NONE', #19969, #3731, #47321, .T. ) ;
#74954 = DATE_TIME_ROLE ( 'classification_date' ) ;
#74956 = CC_DESIGN_APPROVAL ( #54338, ( #16578 ) ) ;
#74957 = CARTESIAN_POINT ( 'NONE',  ( -108.8968792378191921, -25.14264220134206695, 6.986250900936221697 ) ) ;
#74958 = CARTESIAN_POINT ( 'NONE',  ( -40.62287095715005592, -23.47593901973091235, -1.443836447539011525 ) ) ;
#74959 = CARTESIAN_POINT ( 'NONE',  ( -20.49763986188970932, -1.003951800832726615, 11.49999999999999645 ) ) ;
#74960 = CARTESIAN_POINT ( 'NONE',  ( -47.52287095715006160, -23.48786465467240347, 11.44779295918255002 ) ) ;
#74961 = CARTESIAN_POINT ( 'NONE',  ( -42.62287095715004881, -24.66019654487199020, 8.947790411086135265 ) ) ;
#74962 = AXIS2_PLACEMENT_3D ( 'NONE', #31920, #61877, #1978 ) ;
#74963 = EDGE_LOOP ( 'NONE', ( #30222, #55944, #10111, #79365 ) ) ;
#74964 = CARTESIAN_POINT ( 'NONE',  ( -62.52287095715009002, -23.72773821059535848, 11.05748984161097503 ) ) ;
#74965 = CARTESIAN_POINT ( 'NONE',  ( -3.826923076923074429, -6.376774720514427841, 21.75000000000000355 ) ) ;
#74966 = DIRECTION ( 'NONE',  ( -0.9921023176230513441, 0.000000000000000000, 0.1254312216594016538 ) ) ;
#74967 = VECTOR ( 'NONE', #31597, 1000.000000000000000 ) ;
#74968 = ADVANCED_FACE ( 'NONE', ( #74106 ), #22781, .F. ) ;
#74969 = CARTESIAN_POINT ( 'NONE',  ( -61.62287095715002749, -23.94994826722515668, -0.6494450866351731966 ) ) ;
#74970 = EDGE_LOOP ( 'NONE', ( #12002, #24372, #23167, #29846 ) ) ;
#74971 = CARTESIAN_POINT ( 'NONE',  ( 6.273728352332436309, -6.376774720514415407, 20.10092598260902008 ) ) ;
#74972 = CARTESIAN_POINT ( 'NONE',  ( 20.35648204094723468, -10.72454223111430593, 11.49999999999999645 ) ) ;
#74973 = CARTESIAN_POINT ( 'NONE',  ( -4.239441843796335263, -22.36999388947090139, -1.500000000000002220 ) ) ;
#74974 = CARTESIAN_POINT ( 'NONE',  ( 3.557932825399831689, -6.376774720514429617, 21.44518044978141091 ) ) ;
#74975 = B_SPLINE_SURFACE_WITH_KNOTS ( 'NONE', 3, 1, ( 
 ( #39265, #84940 ),
 ( #70225, #15425 ),
 ( #705, #31652 ),
 ( #41277, #74593 ),
 ( #94552, #25039 ),
 ( #58884, #66520 ),
 ( #1718, #40275 ),
 ( #72232, #4603 ),
 ( #35550, #32654 ),
 ( #96940, #67008 ),
 ( #63632, #89825 ),
 ( #20295, #56014 ),
 ( #51267, #16930 ),
 ( #66023, #82208 ),
 ( #9821, #17938 ),
 ( #50776, #5083 ),
 ( #95061, #48899 ),
 ( #43166, #86943 ),
 ( #79825, #27434 ) ),
 .UNSPECIFIED., .F., .F., .F.,
 ( 4, 1, 1, 1, 1, 1, 1, 1, 1, 1, 1, 1, 1, 1, 1, 1, 4 ),
 ( 2, 2 ),
 ( 0.000000000000000000, 0.06185264594669137583, 0.1212838306153700696, 0.1807779320756104369, 0.2392732340142800229, 0.2986414352139401540, 0.3581858222417109161, 0.4207600867589704752, 0.4852046730216416082, 0.5503622689482856600, 0.6136499245309111616, 0.6766234955168239917, 0.7391080134690120040, 0.8021647022429441165, 0.8667165971324768403, 0.9320376285055436139, 1.000000000000000000 ),
 ( 0.000000000000000000, 1.000000000000000000 ),
 .UNSPECIFIED. ) ;
#74976 = DIRECTION ( 'NONE',  ( 3.496357139254347770E-15, -0.9940716917543757081, -0.1087265912856345967 ) ) ;
#74977 = CARTESIAN_POINT ( 'NONE',  ( 10.54059822343757702, -5.876774720514426953, 17.17691942396159988 ) ) ;
#74978 = CARTESIAN_POINT ( 'NONE',  ( -40.52287095715006870, -23.48786465467241058, 11.44779295918255180 ) ) ;
#74979 = CARTESIAN_POINT ( 'NONE',  ( -99.19454649804008284, -25.30157761398589500, 5.270710036488496009 ) ) ;
#74980 = CARTESIAN_POINT ( 'NONE',  ( 15.10893391618534665, -15.86458014800626692, -1.500000000000002220 ) ) ;
#74981 = ADVANCED_FACE ( 'NONE', ( #76575 ), #99903, .T. ) ;
#74982 = CARTESIAN_POINT ( 'NONE',  ( -10.54059822343757880, -5.876774720514426953, 23.12308057603841149 ) ) ;
#74983 = AXIS2_PLACEMENT_3D ( 'NONE', #34525, #19776, #76424 ) ;
#74984 = CARTESIAN_POINT ( 'NONE',  ( -34.58953762381673158, -24.66019654487199375, 8.947790411086135265 ) ) ;
#74985 = EDGE_CURVE ( 'NONE', #53498, #21106, #463, .T. ) ;
#74986 = LINE ( 'NONE', #21200, #59013 ) ;
#74987 = DIRECTION ( 'NONE',  ( -1.000000000000000000, -0.000000000000000000, -0.000000000000000000 ) ) ;
#74988 = LINE ( 'NONE', #97831, #84170 ) ;
#74989 = ORIENTED_EDGE ( 'NONE', *, *, #62720, .T. ) ;
#74990 = CARTESIAN_POINT ( 'NONE',  ( 1.945971545120378288, -20.36639758168144709, -1.500000000000002220 ) ) ;
#74991 = ORIENTED_EDGE ( 'NONE', *, *, #89518, .T. ) ;
#74992 = ORIENTED_EDGE ( 'NONE', *, *, #33291, .T. ) ;
#74993 = ORIENTED_EDGE ( 'NONE', *, *, #67611, .F. ) ;
#74994 = VERTEX_POINT ( 'NONE', #14685 ) ;
#74995 = CARTESIAN_POINT ( 'NONE',  ( 11.60186680256600233, 19.91347440808847935, 11.49999999999998934 ) ) ;
#74997 = EDGE_CURVE ( 'NONE', #17101, #14971, #85199, .T. ) ;
#74996 = CARTESIAN_POINT ( 'NONE',  ( -61.61074830552635717, -23.48783264082476663, -1.443836473390096575 ) ) ;
#74998 = CARTESIAN_POINT ( 'NONE',  ( -14.42758394406654610, -14.16023863206117994, -1.500000000000002220 ) ) ;
#74999 = VECTOR ( 'NONE', #34611, 1000.000000000000114 ) ;
#75000 = ORIENTED_EDGE ( 'NONE', *, *, #58385, .F. ) ;
#75001 = CARTESIAN_POINT ( 'NONE',  ( 29.57907552799942863, -6.376774720514426953, 29.21818156447040948 ) ) ;
#75002 = LINE ( 'NONE', #6506, #44943 ) ;
#75003 = EDGE_CURVE ( 'NONE', #92987, #69513, #37535, .T. ) ;
#75004 = CARTESIAN_POINT ( 'NONE',  ( -51.52287095715009002, -23.48783264082477018, -1.443836473390092578 ) ) ;
#75005 = CARTESIAN_POINT ( 'NONE',  ( -99.62530823664367574, -24.51419770103158413, 9.386484678747175181 ) ) ;
#75007 = ORIENTED_EDGE ( 'NONE', *, *, #60128, .T. ) ;
#75006 = CARTESIAN_POINT ( 'NONE',  ( -20.52298544035203776, 6.160189734329080125, 11.49999999999999645 ) ) ;
#75008 = FACE_OUTER_BOUND ( 'NONE', #32075, .T. ) ;
#75009 = VECTOR ( 'NONE', #28531, 1000.000000000000000 ) ;
#75010 = EDGE_LOOP ( 'NONE', ( #64747, #62692, #43248, #79270 ) ) ;
#75011 = CARTESIAN_POINT ( 'NONE',  ( -0.2510023010970363067, -20.70922355669356563, -1.500000000000002220 ) ) ;
#75012 = EDGE_LOOP ( 'NONE', ( #86507, #10489, #15378, #25355 ) ) ;
#75013 = LINE ( 'NONE', #13116, #30792 ) ;
#75014 = VERTEX_POINT ( 'NONE', #62894 ) ;
#75015 = CARTESIAN_POINT ( 'NONE',  ( 3.176458874063926352, -5.965225279485592225, -28.85257003503889095 ) ) ;
#75016 = ORIENTED_EDGE ( 'NONE', *, *, #44039, .T. ) ;
#75017 = CARTESIAN_POINT ( 'NONE',  ( 20.71091302404612833, 3.140364381853995912, -1.500000000000002220 ) ) ;
#75018 = CARTESIAN_POINT ( 'NONE',  ( 21.77894307773758698, -2.757304969434911879, 11.49999999999999645 ) ) ;
#75019 = CARTESIAN_POINT ( 'NONE',  ( -91.55620429048339304, -24.65952944569304606, 1.056160979905700792 ) ) ;
#75020 = CARTESIAN_POINT ( 'NONE',  ( -3.310667818835141940, 22.29536907041311977, -1.500000000000002220 ) ) ;
#75021 = CARTESIAN_POINT ( 'NONE',  ( -19.40599490818632233, 7.965113791304038848, 11.49999999999998934 ) ) ;
#75022 = CARTESIAN_POINT ( 'NONE',  ( 5.930937628982182908, -6.376774720514417183, 20.24478033514397524 ) ) ;
#75023 = CARTESIAN_POINT ( 'NONE',  ( -119.5902191003218036, -24.15620529776629510, 10.23563542870659582 ) ) ;
#75024 = AXIS2_PLACEMENT_3D ( 'NONE', #36402, #75445, #68852 ) ;
#75026 = ADVANCED_FACE ( 'NONE', ( #7080 ), #23184, .T. ) ;
#75025 = DIRECTION ( 'NONE',  ( -0.9496245541219264785, 6.845827386180410961E-16, -0.3133898629642195011 ) ) ;
#75027 = ORIENTED_EDGE ( 'NONE', *, *, #10647, .F. ) ;
#75028 = LOCAL_TIME ( 0, 54, 15.00000000000000000, #60759 ) ;
#75029 = ORIENTED_EDGE ( 'NONE', *, *, #62731, .T. ) ;
#75030 = ORIENTED_EDGE ( 'NONE', *, *, #29467, .F. ) ;
#75031 = CARTESIAN_POINT ( 'NONE',  ( -66.60922468828853482, -23.48783264082476308, -1.443836473390097463 ) ) ;
#75032 = CARTESIAN_POINT ( 'NONE',  ( 3.930203739357332360, 21.12693704021120666, -1.500000000000002220 ) ) ;
#75033 = VECTOR ( 'NONE', #77446, 1000.000000000000000 ) ;
#75034 = EDGE_CURVE ( 'NONE', #53330, #1588, #18196, .T. ) ;
#75035 = B_SPLINE_CURVE_WITH_KNOTS ( 'NONE', 3,
 ( #23785, #956, #31908, #77061 ),
 .UNSPECIFIED., .F., .F.,
 ( 4, 4 ),
 ( 0.8493875703647875142, 0.8503883174055528738 ),
 .UNSPECIFIED. ) ;
#75036 = CARTESIAN_POINT ( 'NONE',  ( -91.52287095715010423, -24.66019654487199730, 8.947790411086115725 ) ) ;
#75037 = ORIENTED_EDGE ( 'NONE', *, *, #71872, .T. ) ;
#75038 = CARTESIAN_POINT ( 'NONE',  ( 16.98782256641479904, -12.52229676876588371, 11.49999999999998934 ) ) ;
#75039 = DIRECTION ( 'NONE',  ( -0.06283980576413537855, -0.000000000000000000, -0.9980236263794188822 ) ) ;
#75040 = CARTESIAN_POINT ( 'NONE',  ( -64.58350591778255989, -24.51314013834315730, 0.6176544820404094027 ) ) ;
#75041 = DIRECTION ( 'NONE',  ( -0.000000000000000000, 1.000000000000000000, -0.000000000000000000 ) ) ;
#75042 = LINE ( 'NONE', #44611, #32911 ) ;
#75043 = CARTESIAN_POINT ( 'NONE',  ( -1.292025413547811308, -5.876774720514412742, 19.72913074730690752 ) ) ;
#75044 = CARTESIAN_POINT ( 'NONE',  ( 7.254013858510784729, 20.86747967231135803, -1.500000000000002220 ) ) ;
#75045 = CIRCLE ( 'NONE', #68534, 1.699999999999998401 ) ;
#75046 = CARTESIAN_POINT ( 'NONE',  ( -20.77875734969026311, -5.356774720514426491, 27.45402280011862217 ) ) ;
#75047 = CARTESIAN_POINT ( 'NONE',  ( -51.93075163254042792, -25.24860253703637269, 6.142475047348883166 ) ) ;
#75048 = CARTESIAN_POINT ( 'NONE',  ( 11.92750898180832131, 4.915819049120522699, -27.17522536519172860 ) ) ;
#75049 = CARTESIAN_POINT ( 'NONE',  ( -43.62287095715007723, -24.34917612406837861, 0.1852690917426608463 ) ) ;
#75050 = CARTESIAN_POINT ( 'NONE',  ( 29.64064043116815128, 5.965225279485572685, 28.71191112024341408 ) ) ;
#75051 = CARTESIAN_POINT ( 'NONE',  ( -1.307668758097810358, 19.38731951181482671, 11.49999999999998934 ) ) ;
#75052 = CARTESIAN_POINT ( 'NONE',  ( 18.88549913130557556, 9.949676122998861061, -1.500000000000002220 ) ) ;
#75053 = CARTESIAN_POINT ( 'NONE',  ( -80.64675904551151575, -29.50249039766296022, 3.409318347773680369 ) ) ;
#75054 = LINE ( 'NONE', #42645, #75419 ) ;
#75055 = CARTESIAN_POINT ( 'NONE',  ( -64.52209052475978979, -23.48786465467241058, 11.44779295918254824 ) ) ;
#75056 = CARTESIAN_POINT ( 'NONE',  ( -129.5228709571500758, -29.50250243563736774, 8.947779886222132717 ) ) ;
#75057 = CARTESIAN_POINT ( 'NONE',  ( 14.74224262856723833, 17.19160420931263999, -1.500000000000002220 ) ) ;
#75058 = EDGE_CURVE ( 'NONE', #78774, #27297, #47300, .T. ) ;
#75059 = B_SPLINE_SURFACE_WITH_KNOTS ( 'NONE', 3, 3, ( 
 ( #9723, #53901, #71126, #46279 ),
 ( #1112, #93949, #32053, #77207 ),
 ( #71629, #48292, #24436, #7712 ),
 ( #79222, #85330, #84835, #78704 ),
 ( #40175, #23417, #46783, #62514 ),
 ( #63025, #9210, #32554, #63527 ),
 ( #15316, #38660, #69626, #62011 ) ),
 .UNSPECIFIED., .F., .F., .F.,
 ( 4, 3, 4 ),
 ( 4, 4 ),
 ( 0.0004766839783817475697, 0.1029713700210893867, 0.2054660560637970312 ),
 ( 0.4696134588889684935, 0.4708428622320510182 ),
 .UNSPECIFIED. ) ;
#75060 = VERTEX_POINT ( 'NONE', #48157 ) ;
#75061 = CARTESIAN_POINT ( 'NONE',  ( -110.2228709571500787, -23.47593901973090169, -1.443836447538996648 ) ) ;
#75062 = LINE ( 'NONE', #34528, #76755 ) ;
#75063 = CARTESIAN_POINT ( 'NONE',  ( -19.53060160647804722, 3.385818350044136338, 11.49999999999999645 ) ) ;
#75064 = CARTESIAN_POINT ( 'NONE',  ( -50.52287095715006160, -25.00158670708909270, 2.256160236439166411 ) ) ;
#75065 = DIRECTION ( 'NONE',  ( -3.773278334453079030E-23, 0.9999999999976377785, 2.173523156925979128E-06 ) ) ;
#75066 = VERTEX_POINT ( 'NONE', #10082 ) ;
#75067 = DIRECTION ( 'NONE',  ( -0.000000000000000000, -0.000000000000000000, -1.000000000000000000 ) ) ;
#75068 = CARTESIAN_POINT ( 'NONE',  ( -28.54389657640137656, -25.26026329057766517, 1.825711730509220976 ) ) ;
#75069 = AXIS2_PLACEMENT_3D ( 'NONE', #92257, #84646, #83140 ) ;
#75071 = EDGE_CURVE ( 'NONE', #68524, #83417, #34423, .T. ) ;
#75070 = CARTESIAN_POINT ( 'NONE',  ( 31.04236049493789906, -5.965225279485572685, 19.84760796525321780 ) ) ;
#75072 = CARTESIAN_POINT ( 'NONE',  ( 19.98343133220876666, -8.209121646405339590, 11.49999999999998934 ) ) ;
#75073 = ADVANCED_FACE ( 'NONE', ( #86207 ), #25300, .F. ) ;
#75074 = CARTESIAN_POINT ( 'NONE',  ( -99.62287095715005592, -23.96127896941631619, -0.6493128931037778218 ) ) ;
#75075 = CARTESIAN_POINT ( 'NONE',  ( -101.6228709571500559, -23.48786465467242479, 11.44779295918254114 ) ) ;
#75076 = EDGE_CURVE ( 'NONE', #93093, #13115, #21954, .T. ) ;
#75077 = DIRECTION ( 'NONE',  ( 0.7512896232465892110, -0.000000000000000000, 0.6599726524652350657 ) ) ;
#75078 = LINE ( 'NONE', #98411, #18267 ) ;
#75079 = CARTESIAN_POINT ( 'NONE',  ( -19.37706247964952411, -4.161318200553020041, -1.500000000000002220 ) ) ;
#75080 = B_SPLINE_CURVE_WITH_KNOTS ( 'NONE', 3,
 ( #20383, #82297, #14266, #27525, #74680, #21377, #45242, #37618 ),
 .UNSPECIFIED., .F., .F.,
 ( 4, 2, 2, 4 ),
 ( -0.001224554619866346930, -0.0002241820295893657503, 0.0007761905606876154298, 0.002776935741241573670 ),
 .UNSPECIFIED. ) ;
#75081 = ORIENTED_EDGE ( 'NONE', *, *, #99278, .F. ) ;
#75082 = VECTOR ( 'NONE', #23669, 1000.000000000000114 ) ;
#75083 = EDGE_CURVE ( 'NONE', #29468, #66746, #57043, .T. ) ;
#75084 = CARTESIAN_POINT ( 'NONE',  ( -11.07518157712430096, -17.02944518001645946, 11.49999999999999645 ) ) ;
#75085 = CARTESIAN_POINT ( 'NONE',  ( -8.160000000000000142, -10.15233964170348457, 0.003711184059992174607 ) ) ;
#75086 = B_SPLINE_CURVE_WITH_KNOTS ( 'NONE', 3,
 ( #89432, #20395, #59482, #98521 ),
 .UNSPECIFIED., .F., .F.,
 ( 4, 4 ),
 ( 0.09882728979063827579, 0.09982803683140384354 ),
 .UNSPECIFIED. ) ;
#75087 = PLANE ( 'NONE',  #68432 ) ;
#75088 = ORIENTED_EDGE ( 'NONE', *, *, #52482, .F. ) ;
#75089 = CARTESIAN_POINT ( 'NONE',  ( -107.5228709571500758, -23.48786465467241769, 11.44779295918253936 ) ) ;
#75090 = CARTESIAN_POINT ( 'NONE',  ( 32.25183987940364005, -5.965225279485572685, 2.026414261721653176 ) ) ;
#75091 = DIRECTION ( 'NONE',  ( 0.000000000000000000, 0.000000000000000000, 1.000000000000000000 ) ) ;
#75092 = LINE ( 'NONE', #60401, #42453 ) ;
#75093 = CARTESIAN_POINT ( 'NONE',  ( -51.48668340319347436, -25.21911759177204715, 6.451348099842415529 ) ) ;
#75094 = CARTESIAN_POINT ( 'NONE',  ( 2.879247915899910470, -19.84986158617241614, -1.500000000000002220 ) ) ;
#75095 = EDGE_CURVE ( 'NONE', #25724, #28213, #66763, .T. ) ;
#75096 = EDGE_CURVE ( 'NONE', #43147, #10045, #32924, .T. ) ;
#75097 = PLANE ( 'NONE',  #25669 ) ;
#75098 = ORIENTED_EDGE ( 'NONE', *, *, #46604, .F. ) ;
#75099 = VECTOR ( 'NONE', #56981, 1000.000000000000000 ) ;
#75100 = EDGE_CURVE ( 'NONE', #24828, #2526, #9582, .T. ) ;
#75101 = CARTESIAN_POINT ( 'NONE',  ( -0.9063223138645676302, -22.79912562917415997, 11.49999999999999645 ) ) ;
#75102 = DIRECTION ( 'NONE',  ( 0.000000000000000000, 0.000000000000000000, -1.000000000000000000 ) ) ;
#75103 = DIRECTION ( 'NONE',  ( -0.000000000000000000, -1.000000000000000000, -0.000000000000000000 ) ) ;
#75104 = LINE ( 'NONE', #5601, #46788 ) ;
#75105 = CARTESIAN_POINT ( 'NONE',  ( 6.326958800731953048, -5.876774720514425177, 21.47849181751607972 ) ) ;
#75106 = ADVANCED_FACE ( 'NONE', ( #56778 ), #33411, .F. ) ;
#75107 = DIRECTION ( 'NONE',  ( -0.000000000000000000, 1.000000000000000000, -0.000000000000000000 ) ) ;
#75108 = VECTOR ( 'NONE', #80076, 1000.000000000000000 ) ;
#75109 = CARTESIAN_POINT ( 'NONE',  ( -9.774569144048079750, -20.17623354167628946, 11.49999999999999645 ) ) ;
#75110 = CARTESIAN_POINT ( 'NONE',  ( -19.69812919673063689, 0.3587747205143964613, -22.00173861453436430 ) ) ;
#75111 = VERTEX_POINT ( 'NONE', #72995 ) ;
#75112 = CARTESIAN_POINT ( 'NONE',  ( 6.737473828552405841, -19.20966278261563076, -1.500000000000002220 ) ) ;
#75113 = AXIS2_PLACEMENT_3D ( 'NONE', #71957, #94773, #18152 ) ;
#75114 = ORIENTED_EDGE ( 'NONE', *, *, #18061, .F. ) ;
#75115 = CARTESIAN_POINT ( 'NONE',  ( -11.38079350637645959, -19.95400817559217899, -1.500000000000002220 ) ) ;
#75116 = ADVANCED_FACE ( 'NONE', ( #57285 ), #95320, .F. ) ;
#75117 = PLANE ( 'NONE',  #95470 ) ;
#75118 = VERTEX_POINT ( 'NONE', #1483 ) ;
#75119 = B_SPLINE_CURVE_WITH_KNOTS ( 'NONE', 3,
 ( #53658, #86087, #54652, #55661 ),
 .UNSPECIFIED., .F., .F.,
 ( 4, 4 ),
 ( 0.000000000000000000, 9.999999999998897304E-05 ),
 .UNSPECIFIED. ) ;
#75120 = CARTESIAN_POINT ( 'NONE',  ( -89.55620429048337883, -23.48783264082478794, -1.443836473390065045 ) ) ;
#75121 = ADVANCED_FACE ( 'NONE', ( #70992 ), #10577, .T. ) ;
#75122 = CARTESIAN_POINT ( 'NONE',  ( -77.51233885098207566, -23.96169478059713498, 10.65365249895717703 ) ) ;
#75123 = ADVANCED_FACE ( 'NONE', ( #72493 ), #41542, .T. ) ;
#75124 = CYLINDRICAL_SURFACE ( 'NONE', #13998, 4.450000000000000178 ) ;
#75126 = ORIENTED_EDGE ( 'NONE', *, *, #73135, .F. ) ;
#75125 = CARTESIAN_POINT ( 'NONE',  ( -20.86817740539179056, 4.147639786170328691, 11.49999999999999645 ) ) ;
#75127 = B_SPLINE_CURVE_WITH_KNOTS ( 'NONE', 3,
 ( #18802, #64016, #70592, #80712 ),
 .UNSPECIFIED., .F., .F.,
 ( 4, 4 ),
 ( 0.06976270681042859301, 1.000000000000000000 ),
 .UNSPECIFIED. ) ;
#75128 = ORIENTED_EDGE ( 'NONE', *, *, #61885, .T. ) ;
#75129 = CARTESIAN_POINT ( 'NONE',  ( -10.57539506955483333, 19.50334513348995813, 11.49999999999998934 ) ) ;
#75130 = CARTESIAN_POINT ( 'NONE',  ( -18.80638259998596951, 8.471300643254643603, 11.49999999999998934 ) ) ;
#75131 = ORIENTED_EDGE ( 'NONE', *, *, #44913, .F. ) ;
#75132 = ORIENTED_EDGE ( 'NONE', *, *, #69069, .F. ) ;
#75133 = DIRECTION ( 'NONE',  ( -0.000000000000000000, 1.000000000000000000, -0.000000000000000000 ) ) ;
#75134 = CARTESIAN_POINT ( 'NONE',  ( -55.52287095715006870, -23.47596703998600631, 11.44779298504228926 ) ) ;
#75135 = ORIENTED_EDGE ( 'NONE', *, *, #3220, .F. ) ;
#75136 =( BOUNDED_SURFACE ( )  B_SPLINE_SURFACE ( 3, 2, ( 
 ( #72360, #97185, #73847 ),
 ( #88581, #2855, #19054 ),
 ( #18556, #50512, #28175 ),
 ( #33788, #72860, #81957 ) ),
 .UNSPECIFIED., .F., .F., .T. ) 
 B_SPLINE_SURFACE_WITH_KNOTS ( ( 4, 4 ),
 ( 3, 3 ),
 ( 0.01105101719324316605, 0.01425305434006712661 ),
 ( 0.000000000000000000, 1.000000000000000000 ),
 .UNSPECIFIED. ) 
 GEOMETRIC_REPRESENTATION_ITEM ( )  RATIONAL_B_SPLINE_SURFACE ( (
 ( 1.000000000000000000, 0.7071067811865476838, 1.000000000000000000),
 ( 1.000000000000000000, 0.7071067811865476838, 1.000000000000000000),
 ( 1.000000000000000000, 0.7071067811865469066, 1.000000000000000000),
 ( 1.000000000000000000, 0.7071067811865469066, 1.000000000000000000) ) ) 
 REPRESENTATION_ITEM ( '' )  SURFACE ( )  );
#75137 = VERTEX_POINT ( 'NONE', #63902 ) ;
#75138 = CARTESIAN_POINT ( 'NONE',  ( -124.4728709571500360, -25.30558663486635851, 5.000950659935021747 ) ) ;
#75139 = CARTESIAN_POINT ( 'NONE',  ( -46.52287095715006870, -24.50216790748203621, 0.6166512839542526159 ) ) ;
#75140 = CARTESIAN_POINT ( 'NONE',  ( 15.48350366603649064, -4.450064631498825918, -28.28653584630414386 ) ) ;
#75141 = CARTESIAN_POINT ( 'NONE',  ( 6.562613027033147084, 19.67253995144353240, -1.500000000000002220 ) ) ;
#75142 = CARTESIAN_POINT ( 'NONE',  ( -21.62197530259306788, 2.132803791230205359, 11.49999999999999645 ) ) ;
#75143 = VERTEX_POINT ( 'NONE', #79082 ) ;
#75144 = CIRCLE ( 'NONE', #67131, 21.89999999999999858 ) ;
#75145 = CARTESIAN_POINT ( 'NONE',  ( -40.62552394256396582, -25.31583768111513066, 5.067902445723437843 ) ) ;
#75146 = DIRECTION ( 'NONE',  ( 0.000000000000000000, 0.000000000000000000, -1.000000000000000000 ) ) ;
#75147 = CARTESIAN_POINT ( 'NONE',  ( -115.5935074813547629, -23.85016227208580730, -0.8807180028928280890 ) ) ;
#75148 = CARTESIAN_POINT ( 'NONE',  ( 9.841385673706204429, 20.17164819615926064, 11.49999999999998934 ) ) ;
#75149 = CARTESIAN_POINT ( 'NONE',  ( -50.95636528269795207, -25.31296727064691510, 4.561343259994464105 ) ) ;
#75150 = EDGE_LOOP ( 'NONE', ( #87041, #86136, #19386, #15284 ) ) ;
#75151 = DIRECTION ( 'NONE',  ( -0.000000000000000000, -1.000000000000000000, -0.000000000000000000 ) ) ;
#75152 = DIRECTION ( 'NONE',  ( -1.000000000000000000, 0.000000000000000000, -0.000000000000000000 ) ) ;
#75153 = VECTOR ( 'NONE', #96782, 1000.000000000000114 ) ;
#75154 = ORIENTED_EDGE ( 'NONE', *, *, #55981, .F. ) ;
#75155 = VERTEX_POINT ( 'NONE', #56280 ) ;
#75156 = CARTESIAN_POINT ( 'NONE',  ( -46.61533402018017114, -23.48786465467240703, 11.44779295918255180 ) ) ;
#75157 = ORIENTED_EDGE ( 'NONE', *, *, #42949, .F. ) ;
#75158 = CARTESIAN_POINT ( 'NONE',  ( -9.338289970059909351, 19.12570833482435617, -1.500000000000002220 ) ) ;
#75159 = ORIENTED_EDGE ( 'NONE', *, *, #55390, .T. ) ;
#75160 = CARTESIAN_POINT ( 'NONE',  ( -5.891303133519534718, -5.876774720514420736, 20.71116975788854475 ) ) ;
#75161 = B_SPLINE_CURVE_WITH_KNOTS ( 'NONE', 3,
 ( #65443, #40191, #86363, #81136, #82134, #48311, #9228, #20222, #16847, #1637, #88760, #51193, #47806, #11615, #96362, #11123, #73529, #65939, #66440 ),
 .UNSPECIFIED., .F., .F.,
 ( 4, 1, 1, 1, 1, 1, 1, 1, 1, 1, 1, 1, 1, 1, 1, 1, 4 ),
 ( 0.000000000000000000, 0.06184170298390879311, 0.1212623730944467210, 0.1807459488653150592, 0.2392309018221055461, 0.2983075587884643221, 0.3581827976158475924, 0.4203592307800689265, 0.4847924155141841718, 0.5499384837666866366, 0.6137182775404276258, 0.6766807072496321407, 0.7391541704483172159, 0.8021997032403536121, 0.8667401776163008442, 0.9320496524002468419, 1.000000000000000000 ),
 .UNSPECIFIED. ) ;
#75162 = CARTESIAN_POINT ( 'NONE',  ( -20.81348254183067681, -2.960215062046979373, -1.500000000000002220 ) ) ;
#75163 = PLANE ( 'NONE',  #66043 ) ;
#75164 = CARTESIAN_POINT ( 'NONE',  ( 9.008567143757492346, 20.83016157428379955, 11.49999999999998934 ) ) ;
#75165 = DIRECTION ( 'NONE',  ( 0.000000000000000000, -1.000000000000000000, 0.000000000000000000 ) ) ;
#75166 = DIRECTION ( 'NONE',  ( 0.000000000000000000, 0.000000000000000000, 1.000000000000000000 ) ) ;
#75167 = CARTESIAN_POINT ( 'NONE',  ( 13.84421170697429737, -16.98027460053469895, -1.500000000000002220 ) ) ;
#75168 = CARTESIAN_POINT ( 'NONE',  ( -13.57581083383197296, -5.876774720514426953, 19.78786796564403616 ) ) ;
#75169 = ORIENTED_EDGE ( 'NONE', *, *, #6082, .F. ) ;
#75170 = CARTESIAN_POINT ( 'NONE',  ( 29.75874681941402855, -6.376774720514429617, 26.36094095093186596 ) ) ;
#75171 = VERTEX_POINT ( 'NONE', #2987 ) ;
#75172 = CARTESIAN_POINT ( 'NONE',  ( -84.63259752206350583, -24.15620529776628445, 10.23563542870660292 ) ) ;
#75173 = DIRECTION ( 'NONE',  ( -0.000000000000000000, 0.000000000000000000, 1.000000000000000000 ) ) ;
#75174 = CARTESIAN_POINT ( 'NONE',  ( -20.41827678953962888, -23.96516754450130549, 1.363349870542264863 ) ) ;
#75175 = CARTESIAN_POINT ( 'NONE',  ( -18.72683625574626376, -10.08736549105613278, -1.500000000000002220 ) ) ;
#75176 = CARTESIAN_POINT ( 'NONE',  ( -112.5175298555210190, -24.15543982623908192, -0.2315651400026420004 ) ) ;
#75177 = CARTESIAN_POINT ( 'NONE',  ( -26.71643515402310953, -24.97064495862396427, 2.706679050326408653 ) ) ;
#75178 = CARTESIAN_POINT ( 'NONE',  ( -85.64374433404715603, -23.85016227208579664, -0.8807180028928370819 ) ) ;
#75179 = CARTESIAN_POINT ( 'NONE',  ( -33.54542880383117875, -24.15543982623906771, -0.2315651400026580431 ) ) ;
#75180 = CARTESIAN_POINT ( 'NONE',  ( -39.62287095715004881, -24.51387760970725793, 9.387446482453437824 ) ) ;
#75181 = ORIENTED_EDGE ( 'NONE', *, *, #17729, .T. ) ;
#75182 = EDGE_CURVE ( 'NONE', #79519, #65212, #64904, .T. ) ;
#75183 = CARTESIAN_POINT ( 'NONE',  ( -6.723608784814384620, 18.44229941887336821, 11.49999999999999645 ) ) ;
#75184 = CARTESIAN_POINT ( 'NONE',  ( -7.662324775236974972, 31.59999999999999787, 0.000000000000000000 ) ) ;
#75185 = ADVANCED_FACE ( 'NONE', ( #88216 ), #96320, .T. ) ;
#75186 = CARTESIAN_POINT ( 'NONE',  ( -90.25937923781921768, -25.26877915520014994, 5.947789088310639904 ) ) ;
#75187 = ORIENTED_EDGE ( 'NONE', *, *, #71318, .F. ) ;
#75188 = EDGE_CURVE ( 'NONE', #38852, #86526, #44023, .T. ) ;
#75189 = CARTESIAN_POINT ( 'NONE',  ( -68.97793375987197351, -25.27731752798380072, 5.835604325072999643 ) ) ;
#75190 = CARTESIAN_POINT ( 'NONE',  ( 30.09341516180546350, 2.682774720514426559, -11.39311774897855756 ) ) ;
#75191 = EDGE_CURVE ( 'NONE', #1282, #91104, #79737, .T. ) ;
#75192 = CARTESIAN_POINT ( 'NONE',  ( -27.51938903004329617, -24.63785229949931121, 8.245938776320086205 ) ) ;
#75193 = EDGE_CURVE ( 'NONE', #31628, #41503, #71599, .T. ) ;
#75194 = CARTESIAN_POINT ( 'NONE',  ( -31.62287095715005236, -24.64898659630367206, 1.056161002820817485 ) ) ;
#75195 = CARTESIAN_POINT ( 'NONE',  ( -18.76583335001664565, 6.068782795689376286, -1.500000000000002220 ) ) ;
#75196 = B_SPLINE_CURVE_WITH_KNOTS ( 'NONE', 3,
 ( #92399, #30504, #44747, #37122, #59472, #98510, #68082, #22872 ),
 .UNSPECIFIED., .F., .F.,
 ( 4, 2, 2, 4 ),
 ( -0.001240666984356060066, -0.0002401179793396629458, 0.0007604310256767341739, 0.002761529035709528630 ),
 .UNSPECIFIED. ) ;
#75197 = ORIENTED_EDGE ( 'NONE', *, *, #54005, .T. ) ;
#75198 = B_SPLINE_CURVE_WITH_KNOTS ( 'NONE', 3,
 ( #57277, #42042, #88705, #89202, #71488, #48152 ),
 .UNSPECIFIED., .F., .F.,
 ( 4, 2, 4 ),
 ( 6.391158118966175555E-06, 0.001387004593080783544, 0.002767618028042600695 ),
 .UNSPECIFIED. ) ;
#75199 = DIRECTION ( 'NONE',  ( 0.000000000000000000, 1.000000000000000000, 0.000000000000000000 ) ) ;
#75200 = CARTESIAN_POINT ( 'NONE',  ( 22.81105451610979173, -6.475225279485573360, -18.46691820600746681 ) ) ;
#75201 = AXIS2_PLACEMENT_3D ( 'NONE', #9196, #56903, #87324 ) ;
#75202 = DATE_AND_TIME ( #44271, #40931 ) ;
#75203 = ORIENTED_EDGE ( 'NONE', *, *, #78088, .T. ) ;
#75204 = CARTESIAN_POINT ( 'NONE',  ( -19.80875734969026425, 0.3587747205144265483, 31.02402280011862246 ) ) ;
#75205 = CARTESIAN_POINT ( 'NONE',  ( -36.62287095715005592, -23.48786465467240347, 11.44779295918255180 ) ) ;
#75206 = CARTESIAN_POINT ( 'NONE',  ( -55.65727489617320600, -23.85016227208578954, -0.8807180028928371929 ) ) ;
#75207 = FACE_OUTER_BOUND ( 'NONE', #96083, .T. ) ;
#75208 = CARTESIAN_POINT ( 'NONE',  ( -7.324001883147635894, -6.376774720514413630, 20.17732409774492197 ) ) ;
#75209 = CARTESIAN_POINT ( 'NONE',  ( -69.96836528472165639, -25.24515055822771004, 5.376154610849502191 ) ) ;
#75210 = CARTESIAN_POINT ( 'NONE',  ( -85.58953762381672448, -25.00158670708909625, 2.256160236439166411 ) ) ;
#75211 = CARTESIAN_POINT ( 'NONE',  ( 6.038693664686949347, 19.05185810397003721, 11.49999999999998934 ) ) ;
#75212 = EDGE_CURVE ( 'NONE', #13162, #5889, #51143, .T. ) ;
#75213 = AXIS2_PLACEMENT_3D ( 'NONE', #73143, #51295, #97465 ) ;
#75214 = CARTESIAN_POINT ( 'NONE',  ( -100.3793702452611285, -25.27532861982699330, 2.834177754712485342 ) ) ;
#75215 = CARTESIAN_POINT ( 'NONE',  ( -0.1426030150137709562, -21.20389190742572083, 11.50200000000000422 ) ) ;
#75216 = ORIENTED_EDGE ( 'NONE', *, *, #46690, .T. ) ;
#75217 = CARTESIAN_POINT ( 'NONE',  ( -29.52287095715005449, -24.25394151242297980, 0.1849423911881836469 ) ) ;
#75218 = CARTESIAN_POINT ( 'NONE',  ( 13.59451591917074431, -3.316774720514426456, -28.23515841827053308 ) ) ;
#75219 = EDGE_CURVE ( 'NONE', #51956, #44056, #55787, .T. ) ;
#75220 = CARTESIAN_POINT ( 'NONE',  ( -119.5565861874301135, -23.73766607897670866, -1.055555164236450016 ) ) ;
#75221 = CARTESIAN_POINT ( 'NONE',  ( -80.56574517205659447, -23.48786465467241058, 11.44779295918254824 ) ) ;
#75222 = DIRECTION ( 'NONE',  ( -0.000000000000000000, -0.000000000000000000, -1.000000000000000000 ) ) ;
#75223 = CARTESIAN_POINT ( 'NONE',  ( -107.6228709571500701, -24.66019654487199730, 8.947790411086124607 ) ) ;
#75224 = CARTESIAN_POINT ( 'NONE',  ( -119.6228709571500559, -23.72747288104469732, -1.053458166803224350 ) ) ;
#75225 = CARTESIAN_POINT ( 'NONE',  ( -2.148731487934370410, -6.376774720514411854, 19.46295461892501422 ) ) ;
#75226 = ORIENTED_EDGE ( 'NONE', *, *, #80705, .T. ) ;
#75227 = CARTESIAN_POINT ( 'NONE',  ( -64.62287095715005592, -23.48783264082478084, -1.443836473390069042 ) ) ;
#75228 = CARTESIAN_POINT ( 'NONE',  ( 15.14080536460164517, -5.152774720514427642, -26.62908960815038384 ) ) ;
#75229 = ORIENTED_EDGE ( 'NONE', *, *, #62024, .F. ) ;
#75230 = CARTESIAN_POINT ( 'NONE',  ( -20.27173212042777806, -0.06527795377243154895, 11.49999999999998934 ) ) ;
#75231 = B_SPLINE_CURVE_WITH_KNOTS ( 'NONE', 3,
 ( #80255, #18848, #49828, #11243 ),
 .UNSPECIFIED., .F., .F.,
 ( 4, 4 ),
 ( 0.000000000000000000, 9.999999999998897304E-05 ),
 .UNSPECIFIED. ) ;
#75232 = DIRECTION ( 'NONE',  ( -0.000000000000000000, 1.000000000000000000, -0.000000000000000000 ) ) ;
#75233 = CARTESIAN_POINT ( 'NONE',  ( -106.5228709571500332, -23.48783264082477018, -1.443836473390085695 ) ) ;
#75234 = CARTESIAN_POINT ( 'NONE',  ( -20.27875734969026311, 7.743225279485574042, 26.25402280011862288 ) ) ;
#75236 = ORIENTED_EDGE ( 'NONE', *, *, #31659, .F. ) ;
#75235 = ADVANCED_FACE ( 'NONE', ( #82588 ), #52143, .T. ) ;
#75237 = DIRECTION ( 'NONE',  ( 0.000000000000000000, -0.9999999999976377785, -2.173523156925979975E-06 ) ) ;
#75238 = DIRECTION ( 'NONE',  ( 0.000000000000000000, -0.9999999999976377785, -2.173523156925979975E-06 ) ) ;
#75239 = CARTESIAN_POINT ( 'NONE',  ( 10.48293302797296356, 17.13603372422173976, -1.500000000000002220 ) ) ;
#75240 = CARTESIAN_POINT ( 'NONE',  ( 12.56776941831905070, -16.83212535568997126, 11.49999999999999645 ) ) ;
#75241 = AXIS2_PLACEMENT_3D ( 'NONE', #24785, #70474, #55262 ) ;
#75242 = CARTESIAN_POINT ( 'NONE',  ( -28.98875734969026041, 5.965225279485572685, 25.61802280011862720 ) ) ;
#75243 = CARTESIAN_POINT ( 'NONE',  ( -70.62988891066373753, -24.73531770709095312, 8.716586749053508498 ) ) ;
#75244 = CARTESIAN_POINT ( 'NONE',  ( 7.254013858510784729, 20.86747967231135803, -1.500000000000002220 ) ) ;
#75245 = EDGE_CURVE ( 'NONE', #19866, #24503, #35301, .T. ) ;
#75246 = CARTESIAN_POINT ( 'NONE',  ( 17.35315496411208613, -10.91789592880838811, -1.500000000000002220 ) ) ;
#75247 = CARTESIAN_POINT ( 'NONE',  ( -96.52287095715007581, -23.47593901973090524, -1.443836447538996648 ) ) ;
#75248 = CARTESIAN_POINT ( 'NONE',  ( -58.62287095715004881, -29.50250243563736774, 8.947779886222145151 ) ) ;
#75249 = CARTESIAN_POINT ( 'NONE',  ( -10.75273025779354796, -5.876774720514426953, 23.03521261039436752 ) ) ;
#75250 = VERTEX_POINT ( 'NONE', #34922 ) ;
#75251 = CARTESIAN_POINT ( 'NONE',  ( -82.62287095715004170, -23.47596703998600631, 11.44779298504227860 ) ) ;
#75252 = B_SPLINE_SURFACE_WITH_KNOTS ( 'NONE', 3, 3, ( 
 ( #90698, #82585, #98291, #32293 ),
 ( #46522, #844, #39903, #7951 ),
 ( #61761, #76953, #31799, #23160 ),
 ( #9456, #47029, #69358, #92680 ),
 ( #40413, #69861, #78452, #78955 ),
 ( #99777, #1358, #54152, #93183 ),
 ( #77945, #22661, #84573, #53649 ) ),
 .UNSPECIFIED., .F., .F., .F.,
 ( 4, 3, 4 ),
 ( 4, 4 ),
 ( 0.7945040050992239200, 0.8970133687736498995, 0.9995227324480758790 ),
 ( 0.3895929982246983947, 0.3907855847607153987 ),
 .UNSPECIFIED. ) ;
#75253 = CARTESIAN_POINT ( 'NONE',  ( -6.914873625533459744, -0.3587747205144265483, 29.95171384920748281 ) ) ;
#75254 = ORIENTED_EDGE ( 'NONE', *, *, #48399, .F. ) ;
#75255 = ORIENTED_EDGE ( 'NONE', *, *, #46940, .T. ) ;
#75256 = CYLINDRICAL_SURFACE ( 'NONE', #87494, 1.306876713926001354 ) ;
#75257 = CARTESIAN_POINT ( 'NONE',  ( -89.62287095715004170, -23.48786465467241413, 11.44779295918254114 ) ) ;
#75258 = CARTESIAN_POINT ( 'NONE',  ( -76.54259362716096859, -24.51314013834316441, 0.6176544820404193947 ) ) ;
#75259 = CARTESIAN_POINT ( 'NONE',  ( -20.17529555308526668, -4.016306826964139098, -1.500000000000002220 ) ) ;
#75260 = CARTESIAN_POINT ( 'NONE',  ( -21.50746323947805649, 1.722430922125298247, 11.49999999999999645 ) ) ;
#75261 = ORIENTED_EDGE ( 'NONE', *, *, #48652, .T. ) ;
#75262 = DIRECTION ( 'NONE',  ( 0.8219392559241306406, 0.08114015731558892053, -0.5637660281018073150 ) ) ;
#75263 = DIRECTION ( 'NONE',  ( -1.000000000000000000, -3.773278334444167608E-23, -8.201307833595939069E-29 ) ) ;
#75264 = CARTESIAN_POINT ( 'NONE',  ( 8.681249458320607459, -20.60847208623538762, -1.500000000000002220 ) ) ;
#75265 = CARTESIAN_POINT ( 'NONE',  ( -79.53472330195882023, -25.12205703624572095, 6.603901019741583056 ) ) ;
#75266 = CARTESIAN_POINT ( 'NONE',  ( 8.160000000000000142, -9.652339641703484574, -1.621096496867199033 ) ) ;
#75267 = ORIENTED_EDGE ( 'NONE', *, *, #74613, .T. ) ;
#75268 = CARTESIAN_POINT ( 'NONE',  ( -105.6228709571500417, -24.99156045073393173, 7.747789690856161648 ) ) ;
#75269 = CARTESIAN_POINT ( 'NONE',  ( -49.56034792530066824, -23.73791477778911840, 11.05961554403170943 ) ) ;
#75270 = CARTESIAN_POINT ( 'NONE',  ( -20.64841573231975147, 3.066018724555340746, -1.500000000000002220 ) ) ;
#75271 = ORIENTED_EDGE ( 'NONE', *, *, #71038, .T. ) ;
#75272 = VECTOR ( 'NONE', #93945, 1000.000000000000114 ) ;
#75274 = ORIENTED_EDGE ( 'NONE', *, *, #69941, .F. ) ;
#75273 = CARTESIAN_POINT ( 'NONE',  ( -67.63120879115606954, -24.35071581493543746, 9.817618358456023486 ) ) ;
#75275 = ORIENTED_EDGE ( 'NONE', *, *, #76930, .F. ) ;
#75276 = CARTESIAN_POINT ( 'NONE',  ( 15.92621150404962371, 5.965225279485572685, -27.29681269571043245 ) ) ;
#75277 = CARTESIAN_POINT ( 'NONE',  ( 20.99878002148846790, -2.064974809011826729, -1.500000000000002220 ) ) ;
#75278 = ORIENTED_EDGE ( 'NONE', *, *, #84962, .F. ) ;
#75279 = CARTESIAN_POINT ( 'NONE',  ( 3.675000000000004707, 0.000000000000000000, 0.000000000000000000 ) ) ;
#75280 = CARTESIAN_POINT ( 'NONE',  ( -48.87844976791110696, -25.26434452170244072, 6.005111483681883300 ) ) ;
#75281 = CARTESIAN_POINT ( 'NONE',  ( -86.62287095715004170, -29.50250786944525672, 11.44777988621623344 ) ) ;
#75282 = FACE_OUTER_BOUND ( 'NONE', #94072, .T. ) ;
#75283 = CARTESIAN_POINT ( 'NONE',  ( -79.39903364703884847, -25.24308088847154963, 6.330656792118257492 ) ) ;
#75284 = CARTESIAN_POINT ( 'NONE',  ( -13.65724274058436194, -16.95215541261048742, -1.500000000000002220 ) ) ;
#75285 = CARTESIAN_POINT ( 'NONE',  ( -71.49027787591442973, -25.24674164662046394, 5.369049284096080399 ) ) ;
#75287 = ORIENTED_EDGE ( 'NONE', *, *, #99360, .T. ) ;
#75286 = CARTESIAN_POINT ( 'NONE',  ( 19.83320176327591255, -10.20924650237717835, 11.49999999999999645 ) ) ;
#75288 = CARTESIAN_POINT ( 'NONE',  ( -45.62287095715004881, -23.48783264082478084, -1.443836473390070374 ) ) ;
#75289 = DIRECTION ( 'NONE',  ( 0.9975640502598241977, -0.06975647374412546897, -0.000000000000000000 ) ) ;
#75290 = CARTESIAN_POINT ( 'NONE',  ( -36.55620429048339304, -23.48786465467240347, 11.44779295918255180 ) ) ;
#75291 = ORIENTED_EDGE ( 'NONE', *, *, #983, .F. ) ;
#75292 = VECTOR ( 'NONE', #18485, 1000.000000000000114 ) ;
#75293 = VERTEX_POINT ( 'NONE', #5956 ) ;
#75294 = ORIENTED_EDGE ( 'NONE', *, *, #11965, .F. ) ;
#75295 = CARTESIAN_POINT ( 'NONE',  ( -28.52287095715005094, -23.31182002239687989, -1.443836447538998202 ) ) ;
#75296 = DIRECTION ( 'NONE',  ( 0.000000000000000000, 0.000000000000000000, -1.000000000000000000 ) ) ;
#75297 = CARTESIAN_POINT ( 'NONE',  ( 30.60441873609196151, -4.296715115238376015, 26.89749680779764773 ) ) ;
#75298 = CARTESIAN_POINT ( 'NONE',  ( 0.000000000000000000, -7.835183881457442823, -1.399999999999999911 ) ) ;
#75299 = CARTESIAN_POINT ( 'NONE',  ( -12.28997142660015740, 14.97987746540053422, 11.49999999999998934 ) ) ;
#75300 = CARTESIAN_POINT ( 'NONE',  ( -31.52287095715006160, -23.73934037231756022, 11.05740245334329686 ) ) ;
#75301 = ORIENTED_EDGE ( 'NONE', *, *, #46228, .F. ) ;
#75302 = EDGE_CURVE ( 'NONE', #62563, #35826, #58756, .T. ) ;
#75303 = CARTESIAN_POINT ( 'NONE',  ( 4.312616920666290987, -18.91975033782923887, 11.49999999999999645 ) ) ;
#75304 = CARTESIAN_POINT ( 'NONE',  ( -129.6228709571500417, -29.50247984919015209, -1.443849546365044922 ) ) ;
#75305 = ORIENTED_EDGE ( 'NONE', *, *, #60336, .T. ) ;
#75306 = CARTESIAN_POINT ( 'NONE',  ( 15.97264540888995299, 3.316774720514426456, -27.93485543958162154 ) ) ;
#75307 = EDGE_CURVE ( 'NONE', #85611, #7766, #96815, .T. ) ;
#75308 = CARTESIAN_POINT ( 'NONE',  ( 3.552794897967157528, -5.876774720514402084, 18.18650940196788568 ) ) ;
#75309 = DIRECTION ( 'NONE',  ( -0.7297249646783463550, 1.486126453139760626E-06, -0.6837407958597889746 ) ) ;
#75310 = EDGE_CURVE ( 'NONE', #65583, #11023, #98170, .T. ) ;
#75311 = CARTESIAN_POINT ( 'NONE',  ( -87.62287095715005592, -23.72773821059535848, 11.05748984161097681 ) ) ;
#75312 = CARTESIAN_POINT ( 'NONE',  ( -17.52035102510334141, -8.822347199899118309, 11.49999999999998934 ) ) ;
#75313 = EDGE_CURVE ( 'NONE', #84333, #58299, #30799, .T. ) ;
#75314 = DIRECTION ( 'NONE',  ( -3.773278334453079618E-23, 0.9999999999976377785, 2.173523156925979975E-06 ) ) ;
#75315 = ORIENTED_EDGE ( 'NONE', *, *, #53740, .T. ) ;
#75316 = VECTOR ( 'NONE', #99164, 1000.000000000000000 ) ;
#75317 = CARTESIAN_POINT ( 'NONE',  ( 19.98928912078053699, -8.061568661392884749, -1.500000000000002220 ) ) ;
#75318 = CARTESIAN_POINT ( 'NONE',  ( -33.60985848733059811, -23.73791477778911130, 11.05961554403171299 ) ) ;
#75319 = ADVANCED_FACE ( 'NONE', ( #52640 ), #69361, .T. ) ;
#75320 = CARTESIAN_POINT ( 'NONE',  ( -123.5895376238167245, -23.48786465467241769, 11.44779295918253759 ) ) ;
#75321 = CARTESIAN_POINT ( 'NONE',  ( -50.52287095715006160, -23.47593901973090169, -1.443836447538997092 ) ) ;
#75322 = CARTESIAN_POINT ( 'NONE',  ( -100.2462005486704442, -25.27473224266274343, 3.306208248721503651 ) ) ;
#75323 = CARTESIAN_POINT ( 'NONE',  ( 3.160899137004691717, 22.77513019406404382, -1.500000000000002220 ) ) ;
#75324 = APPROVAL_ROLE ( '' ) ;
#75325 = DIRECTION ( 'NONE',  ( -3.773278334444167608E-23, 1.000000000000000000, 0.000000000000000000 ) ) ;
#75326 = DIRECTION ( 'NONE',  ( -3.773278334453079030E-23, 0.9999999999976377785, 2.173523156925979128E-06 ) ) ;
#75327 = CARTESIAN_POINT ( 'NONE',  ( -7.184633862932894743, 18.80532529184710100, 11.49999999999999645 ) ) ;
#75328 = CARTESIAN_POINT ( 'NONE',  ( -45.62287095715006302, -24.82576562982390911, 8.398263435472966165 ) ) ;
#75329 = DIRECTION ( 'NONE',  ( 0.000000000000000000, -2.173523156925980399E-06, 0.9999999999976378895 ) ) ;
#75330 = CARTESIAN_POINT ( 'NONE',  ( -94.58953762381673869, -23.48786465467241769, 11.44779295918254114 ) ) ;
#75331 = LINE ( 'NONE', #75828, #82907 ) ;
#75332 = CARTESIAN_POINT ( 'NONE',  ( -111.3157468039189695, -25.29779307598838400, 3.994351246507165332 ) ) ;
#75333 = CARTESIAN_POINT ( 'NONE',  ( -1.214729172165279092, -19.82145330704504360, 11.49999999999998934 ) ) ;
#75334 = CARTESIAN_POINT ( 'NONE',  ( -51.52287095715006870, -29.50250786944525672, 11.44777988621624054 ) ) ;
#75335 = CARTESIAN_POINT ( 'NONE',  ( 5.507670110241905448, 19.00313184189250038, -1.500000000000002220 ) ) ;
#75336 = EDGE_CURVE ( 'NONE', #18831, #92224, #30288, .T. ) ;
#75337 = DIRECTION ( 'NONE',  ( 0.000000000000000000, 0.000000000000000000, -1.000000000000000000 ) ) ;
#75338 = PLANE ( 'NONE',  #50008 ) ;
#75339 = CARTESIAN_POINT ( 'NONE',  ( -1.836964591723098117, -6.376774720514410077, 19.23384392940399223 ) ) ;
#75340 = CARTESIAN_POINT ( 'NONE',  ( 18.97174343470660318, 8.267356841975738391, 11.49999999999999645 ) ) ;
#75341 = CARTESIAN_POINT ( 'NONE',  ( -98.62287095715005592, -29.50250786944525672, 11.44777988621623166 ) ) ;
#75342 = PLANE ( 'NONE',  #91802 ) ;
#75343 = CARTESIAN_POINT ( 'NONE',  ( -78.62287095715005592, -29.50248528299804818, 1.056150453629038477 ) ) ;
#75344 = CARTESIAN_POINT ( 'NONE',  ( -17.66434017299383896, 14.31182286555179139, 11.49999999999999645 ) ) ;
#75345 = VERTEX_POINT ( 'NONE', #92188 ) ;
#75346 = CARTESIAN_POINT ( 'NONE',  ( 32.88562546571908740, 0.3587747205144265483, -5.083907541707153754 ) ) ;
#75347 = CARTESIAN_POINT ( 'NONE',  ( -42.52287095715005449, -23.47596703998600631, 11.44779298504229281 ) ) ;
#75348 = B_SPLINE_CURVE_WITH_KNOTS ( 'NONE', 3,
 ( #11568, #42547, #3481, #3978, #51141, #28797, #83065, #75453 ),
 .UNSPECIFIED., .F., .F.,
 ( 4, 2, 2, 4 ),
 ( -0.001224554619866348448, -0.0002241820295893694366, 0.0007761905606876095751, 0.002776935741241576272 ),
 .UNSPECIFIED. ) ;
#75349 = CARTESIAN_POINT ( 'NONE',  ( 8.197725756732245017, -0.4963810196290975307, -3.727086380289611256 ) ) ;
#75350 = AXIS2_PLACEMENT_3D ( 'NONE', #90257, #97856, #59313 ) ;
#75351 = CARTESIAN_POINT ( 'NONE',  ( 0.000000000000000000, -16.94322527948557422, 0.000000000000000000 ) ) ;
#75352 = ORIENTED_EDGE ( 'NONE', *, *, #90583, .T. ) ;
#75353 = AXIS2_PLACEMENT_3D ( 'NONE', #52053, #91598, #59170 ) ;
#75354 = ORIENTED_EDGE ( 'NONE', *, *, #36022, .F. ) ;
#75355 = CARTESIAN_POINT ( 'NONE',  ( -0.4362980769230789257, -6.376774720514411854, 19.46153846153846345 ) ) ;
#75356 = CARTESIAN_POINT ( 'NONE',  ( -17.76840699843883442, -14.40508365592194195, -1.500000000000002220 ) ) ;
#75357 = CARTESIAN_POINT ( 'NONE',  ( -29.58014010773451119, -24.43378003436859558, 0.6176547996449982536 ) ) ;
#75358 = CARTESIAN_POINT ( 'NONE',  ( -16.60028029328060128, 13.79055755010687356, -1.500000000000002220 ) ) ;
#75359 = CARTESIAN_POINT ( 'NONE',  ( -104.5228709571500758, -29.50247984919015209, -1.443849546365050029 ) ) ;
#75360 = CARTESIAN_POINT ( 'NONE',  ( -103.5228709571501042, -23.47593901973090524, -1.443836447538996204 ) ) ;
#75361 = CARTESIAN_POINT ( 'NONE',  ( 13.09772080625096891, 18.35129493929886380, 11.49999999999999645 ) ) ;
#75362 = ORIENTED_EDGE ( 'NONE', *, *, #57358, .F. ) ;
#75363 = LINE ( 'NONE', #20581, #48136 ) ;
#75364 = CARTESIAN_POINT ( 'NONE',  ( 21.96865551644221881, -1.217672407684077918, 11.49999999999998934 ) ) ;
#75365 = B_SPLINE_CURVE_WITH_KNOTS ( 'NONE', 3,
 ( #34127, #18392, #56974, #20372, #3680, #28006 ),
 .UNSPECIFIED., .F., .F.,
 ( 4, 2, 4 ),
 ( 6.391158118973929294E-06, 0.001387004593080789615, 0.002767618028042605031 ),
 .UNSPECIFIED. ) ;
#75366 = EDGE_CURVE ( 'NONE', #79593, #45825, #92060, .T. ) ;
#75367 = CARTESIAN_POINT ( 'NONE',  ( -64.52287095715010423, -24.33832256527049154, 0.1851278514138605669 ) ) ;
#75368 = CARTESIAN_POINT ( 'NONE',  ( -29.00356289826891754, -25.21724786265444607, 6.647730440730820867 ) ) ;
#75369 = ORIENTED_EDGE ( 'NONE', *, *, #8188, .F. ) ;
#75370 = CARTESIAN_POINT ( 'NONE',  ( 14.61581670307174008, -2.682774720514426559, -27.35847990810646024 ) ) ;
#75371 = ADVANCED_FACE ( 'NONE', ( #84077 ), #29296, .F. ) ;
#75372 = CARTESIAN_POINT ( 'NONE',  ( -90.64148822836325792, -23.85049219812686161, 10.88485053497527488 ) ) ;
#75373 = VERTEX_POINT ( 'NONE', #15564 ) ;
#75374 = CARTESIAN_POINT ( 'NONE',  ( 11.05000000000000604, -14.50000000000000178, 24.00000000000000000 ) ) ;
#75375 = EDGE_LOOP ( 'NONE', ( #55415, #30274, #71824, #27080 ) ) ;
#75376 = ORIENTED_EDGE ( 'NONE', *, *, #80746, .T. ) ;
#75377 = CARTESIAN_POINT ( 'NONE',  ( 32.45853543194704116, 0.3587747205144265483, 9.169203677920338080 ) ) ;
#75378 = CARTESIAN_POINT ( 'NONE',  ( -104.5228709571500758, -23.73907113216990084, -1.053371485793246354 ) ) ;
#75379 = FACE_OUTER_BOUND ( 'NONE', #62330, .T. ) ;
#75380 = CARTESIAN_POINT ( 'NONE',  ( -19.05221060042639536, -7.346018566486852031, -1.500000000000002220 ) ) ;
#75381 = EDGE_CURVE ( 'NONE', #94475, #1915, #20712, .T. ) ;
#75382 = ORIENTED_EDGE ( 'NONE', *, *, #63892, .F. ) ;
#75383 = DIRECTION ( 'NONE',  ( 0.000000000000000000, 0.000000000000000000, -1.000000000000000000 ) ) ;
#75384 = CARTESIAN_POINT ( 'NONE',  ( -99.52287095715007581, -23.96177878511310055, 10.65340807706329507 ) ) ;
#75385 = CARTESIAN_POINT ( 'NONE',  ( -53.01255352321339842, -2.682774720514426559, 35.59556822165056644 ) ) ;
#75386 = CARTESIAN_POINT ( 'NONE',  ( -47.52287095715006160, -23.48786465467240347, 11.44779295918255002 ) ) ;
#75387 = ORIENTED_EDGE ( 'NONE', *, *, #9048, .T. ) ;
#75388 = DIRECTION ( 'NONE',  ( -1.000000000000000000, -3.773278334444167608E-23, -8.201307833595939069E-29 ) ) ;
#75389 = CARTESIAN_POINT ( 'NONE',  ( 8.971512145086503409, -1.028487854913504362, -3.750000000000000000 ) ) ;
#75390 = AXIS2_PLACEMENT_3D ( 'NONE', #28672, #59135, #6329 ) ;
#75391 = CARTESIAN_POINT ( 'NONE',  ( 11.01739540223112357, 17.63107602209319680, -1.500000000000002220 ) ) ;
#75392 = EDGE_LOOP ( 'NONE', ( #74272, #43093, #76708, #9412 ) ) ;
#75393 = APPROVAL ( #55384, 'UNKNOWN' ) ;
#75395 = ORIENTED_EDGE ( 'NONE', *, *, #19968, .F. ) ;
#75394 = DIRECTION ( 'NONE',  ( -1.000000000000000000, -0.000000000000000000, -0.000000000000000000 ) ) ;
#75396 = CARTESIAN_POINT ( 'NONE',  ( -68.52287095715010423, -23.95044443724990657, 10.65354141964648704 ) ) ;
#75397 = ORIENTED_EDGE ( 'NONE', *, *, #35592, .F. ) ;
#75398 = VERTEX_POINT ( 'NONE', #98803 ) ;
#75399 = LINE ( 'NONE', #15002, #78603 ) ;
#75400 = DIRECTION ( 'NONE',  ( 0.000000000000000000, 0.000000000000000000, -1.000000000000000000 ) ) ;
#75401 = DIRECTION ( 'NONE',  ( -0.000000000000000000, 1.000000000000000000, -0.000000000000000000 ) ) ;
#75402 = DIRECTION ( 'NONE',  ( 0.000000000000000000, 0.9513357669802769978, -0.3081562241202474572 ) ) ;
#75404 = ORIENTED_EDGE ( 'NONE', *, *, #69016, .F. ) ;
#75403 = CARTESIAN_POINT ( 'NONE',  ( 5.777647480883832287, 21.37485705712154171, 11.49999999999999645 ) ) ;
#75405 = DIRECTION ( 'NONE',  ( -0.000000000000000000, 2.173523156925979552E-06, -0.9999999999976378895 ) ) ;
#75406 = CARTESIAN_POINT ( 'NONE',  ( -6.441999407266626676, 21.70310835763521595, -1.500000000000002220 ) ) ;
#75408 = ORIENTED_EDGE ( 'NONE', *, *, #13599, .T. ) ;
#75407 = CARTESIAN_POINT ( 'NONE',  ( -99.16166289166535819, -25.30166215957521914, 5.311370747606397380 ) ) ;
#75409 = B_SPLINE_CURVE_WITH_KNOTS ( 'NONE', 3,
 ( #53610, #39862, #30750, #802, #70822, #31753, #93638, #1312 ),
 .UNSPECIFIED., .F., .F.,
 ( 4, 2, 2, 4 ),
 ( -0.001224873891641427596, -0.0002244903592271119651, 0.0007758931731872036660, 0.002776660238015834711 ),
 .UNSPECIFIED. ) ;
#75410 = ORIENTED_EDGE ( 'NONE', *, *, #48432, .T. ) ;
#75411 = LINE ( 'NONE', #36370, #66146 ) ;
#75412 = CIRCLE ( 'NONE', #15439, 28.96799999999999642 ) ;
#75413 = AXIS2_PLACEMENT_3D ( 'NONE', #9983, #40445, #23698 ) ;
#75414 = CARTESIAN_POINT ( 'NONE',  ( -3.374260732160392795, -19.82512954709321562, 11.49999999999998934 ) ) ;
#75415 = CARTESIAN_POINT ( 'NONE',  ( -105.6228709571500417, -29.50248789122583659, 2.256150453626215580 ) ) ;
#75416 = VERTEX_POINT ( 'NONE', #31292 ) ;
#75417 = DIRECTION ( 'NONE',  ( 0.8788171126619707119, -0.4771587602595986910, 6.123031769111886291E-17 ) ) ;
#75418 = CARTESIAN_POINT ( 'NONE',  ( -5.617636847906702258, 21.56867655435222630, -1.500000000000002220 ) ) ;
#75419 = VECTOR ( 'NONE', #5057, 1000.000000000000114 ) ;
#75420 = AXIS2_PLACEMENT_3D ( 'NONE', #57092, #80906, #51462 ) ;
#75421 = ORIENTED_EDGE ( 'NONE', *, *, #44913, .T. ) ;
#75422 = CARTESIAN_POINT ( 'NONE',  ( -95.52287095715004739, -23.47593901973090169, -1.443836447538996648 ) ) ;
#75423 = LINE ( 'NONE', #82548, #67029 ) ;
#75424 = LINE ( 'NONE', #41637, #13310 ) ;
#75425 = CIRCLE ( 'NONE', #86812, 1.836000000000002075 ) ;
#75426 = CARTESIAN_POINT ( 'NONE',  ( -43.62287095715003460, -23.47596703998600276, 11.44779298504227505 ) ) ;
#75427 = CARTESIAN_POINT ( 'NONE',  ( -1.081029368968937421, 19.50181592447522050, -1.500000000000002220 ) ) ;
#75428 = EDGE_CURVE ( 'NONE', #57047, #49573, #46525, .T. ) ;
#75429 = CARTESIAN_POINT ( 'NONE',  ( -14.42888051209446409, 15.91495273949476363, -1.500000000000002220 ) ) ;
#75430 = CARTESIAN_POINT ( 'NONE',  ( -2.786875287040666560, -5.876774720514415407, 20.09505574050193388 ) ) ;
#75431 = EDGE_CURVE ( 'NONE', #2274, #38855, #34032, .T. ) ;
#75432 = CARTESIAN_POINT ( 'NONE',  ( -29.49875734969025842, -5.965225279485572685, 25.61802280011862720 ) ) ;
#75433 = CARTESIAN_POINT ( 'NONE',  ( -115.6228709571500559, -24.99132157543166954, 2.256160258750667502 ) ) ;
#75434 = CARTESIAN_POINT ( 'NONE',  ( -16.39533425382319720, 15.89506036719111037, -1.500000000000002220 ) ) ;
#75435 = PERSON_AND_ORGANIZATION ( #70597, #27821 ) ;
#75436 = CARTESIAN_POINT ( 'NONE',  ( -96.62548630188759091, -24.51419770103159834, 9.386484678747169852 ) ) ;
#75437 = DIRECTION ( 'NONE',  ( 0.000000000000000000, 0.000000000000000000, -1.000000000000000000 ) ) ;
#75438 = CARTESIAN_POINT ( 'NONE',  ( -11.50144725928494438, 16.33591932373696665, 11.49999999999999645 ) ) ;
#75439 = PLANE ( 'NONE',  #14442 ) ;
#75440 = CARTESIAN_POINT ( 'NONE',  ( -35.62287095715005592, -23.48786465467240347, 11.44779295918255180 ) ) ;
#75441 = DIRECTION ( 'NONE',  ( 0.2164396139380966033, -0.9762960071199348056, 4.401934094135205585E-16 ) ) ;
#75442 = ORIENTED_EDGE ( 'NONE', *, *, #48309, .T. ) ;
#75443 = EDGE_CURVE ( 'NONE', #9124, #27797, #47032, .T. ) ;
#75444 = FACE_OUTER_BOUND ( 'NONE', #9157, .T. ) ;
#75445 = DIRECTION ( 'NONE',  ( -0.9952638024365006997, 0.000000000000000000, -0.09721092304694052555 ) ) ;
#75446 = CARTESIAN_POINT ( 'NONE',  ( -21.25272785503416273, -4.502612752106283978, 11.49999999999998934 ) ) ;
#75447 = DIRECTION ( 'NONE',  ( 0.000000000000000000, -1.000000000000000000, 0.000000000000000000 ) ) ;
#75448 = CARTESIAN_POINT ( 'NONE',  ( -5.392953615240748455, 18.82278424538476713, -1.500000000000002220 ) ) ;
#75449 = CARTESIAN_POINT ( 'NONE',  ( -34.52287095715006870, -23.73907113217657283, -1.053371485781498196 ) ) ;
#75450 = VERTEX_POINT ( 'NONE', #8461 ) ;
#75451 = PERSON_AND_ORGANIZATION_ROLE ( 'classification_officer' ) ;
#75452 = AXIS2_PLACEMENT_3D ( 'NONE', #75714, #91441, #14317 ) ;
#75453 = CARTESIAN_POINT ( 'NONE',  ( -60.62287095715005592, -23.48786465467241058, 11.44779295918254824 ) ) ;
#75454 = CARTESIAN_POINT ( 'NONE',  ( -47.52287095715006160, -24.64965694238406613, 8.947790433994203596 ) ) ;
#75455 = CARTESIAN_POINT ( 'NONE',  ( -20.18818894172909140, 3.697778396234267184, 11.49999999999999645 ) ) ;
#75456 = CARTESIAN_POINT ( 'NONE',  ( -47.52287095715004739, -24.66019654487199375, 8.947790411086122830 ) ) ;
#75457 = B_SPLINE_CURVE_WITH_KNOTS ( 'NONE', 3,
 ( #5792, #20507, #42878, #73809, #59100, #97151, #36747, #67715, #66227, #50988 ),
 .UNSPECIFIED., .F., .F.,
 ( 4, 2, 2, 2, 4 ),
 ( 0.000000000000000000, 0.0002022805416562973376, 0.0004045610833125946751, 0.0006068416249688920669, 0.0008091221666251893502 ),
 .UNSPECIFIED. ) ;
#75458 = DIRECTION ( 'NONE',  ( -0.000000000000000000, -1.000000000000000000, -0.000000000000000000 ) ) ;
#75459 = B_SPLINE_CURVE_WITH_KNOTS ( 'NONE', 3,
 ( #48207, #25354, #72543, #87252, #1529, #48718, #56331, #72049 ),
 .UNSPECIFIED., .F., .F.,
 ( 4, 2, 2, 4 ),
 ( -0.001240666984356058765, -0.0002401179793396618616, 0.0007604310256767346076, 0.002761529035709530365 ),
 .UNSPECIFIED. ) ;
#75460 = ORIENTED_EDGE ( 'NONE', *, *, #81524, .F. ) ;
#75461 = LINE ( 'NONE', #90706, #58894 ) ;
#75462 = CARTESIAN_POINT ( 'NONE',  ( -40.45829750704998418, -25.18430871329344356, 3.293943118056679165 ) ) ;
#75463 = FACE_OUTER_BOUND ( 'NONE', #52578, .T. ) ;
#75464 = CARTESIAN_POINT ( 'NONE',  ( 24.71017632900191074, 5.356774720514427379, 1.647607965253217399 ) ) ;
#75465 = ORIENTED_EDGE ( 'NONE', *, *, #91511, .T. ) ;
#75466 = CARTESIAN_POINT ( 'NONE',  ( -119.6228709571500701, -24.51283580621365132, 0.6167428607019876940 ) ) ;
#75467 = EDGE_CURVE ( 'NONE', #83063, #52175, #67874, .T. ) ;
#75468 = CARTESIAN_POINT ( 'NONE',  ( 12.94906671069258763, 19.00495796004926419, 11.49999999999999645 ) ) ;
#75469 = CARTESIAN_POINT ( 'NONE',  ( -9.230423729802735622, -20.81519635545753033, 11.49999999999998934 ) ) ;
#75470 = CARTESIAN_POINT ( 'NONE',  ( -106.6228709571500559, -29.50250243563736774, 8.947779886222136270 ) ) ;
#75471 = DIRECTION ( 'NONE',  ( -0.000000000000000000, -1.000000000000000000, -0.000000000000000000 ) ) ;
#75472 = DIRECTION ( 'NONE',  ( 7.994117400814786717E-16, 0.000000000000000000, -1.000000000000000000 ) ) ;
#75473 = LINE ( 'NONE', #67898, #12268 ) ;
#75474 = CARTESIAN_POINT ( 'NONE',  ( -103.6228709571500417, -23.47596703998600631, 11.44779298504227860 ) ) ;
#75475 = CARTESIAN_POINT ( 'NONE',  ( 12.66425630052701479, 17.85959152241435177, -1.500000000000002220 ) ) ;
#75476 = EDGE_CURVE ( 'NONE', #49712, #49492, #75958, .T. ) ;
#75477 = CARTESIAN_POINT ( 'NONE',  ( 7.475222833218381879, -5.876774720514418959, 20.91460388675487891 ) ) ;
#75478 = CIRCLE ( 'NONE', #65826, 1.500000000000001332 ) ;
#75479 = DIRECTION ( 'NONE',  ( 0.000000000000000000, 1.000000000000000000, -0.000000000000000000 ) ) ;
#75480 = DIRECTION ( 'NONE',  ( -0.000000000000000000, -0.000000000000000000, -1.000000000000000000 ) ) ;
#75481 = CARTESIAN_POINT ( 'NONE',  ( 21.57151214508649772, 3.625915217019311583E-15, -1.700000000000000178 ) ) ;
#75482 = CARTESIAN_POINT ( 'NONE',  ( -94.62287095715005592, -23.73934037231758154, 11.05740245334328442 ) ) ;
#75483 = DIRECTION ( 'NONE',  ( -1.000000000000000000, -3.773278334444166432E-23, -8.201307841325785021E-29 ) ) ;
#75484 = VERTEX_POINT ( 'NONE', #68367 ) ;
#75485 = AXIS2_PLACEMENT_3D ( 'NONE', #39101, #31492, #7658 ) ;
#75486 = CARTESIAN_POINT ( 'NONE',  ( 0.3735783541106268979, -20.45636175344465713, 11.49999999999998934 ) ) ;
#75487 = ORIENTED_EDGE ( 'NONE', *, *, #65735, .T. ) ;
#75488 = CIRCLE ( 'NONE', #69054, 2.249999999999998668 ) ;
#75489 = ORIENTED_EDGE ( 'NONE', *, *, #17601, .T. ) ;
#75490 = VERTEX_POINT ( 'NONE', #99303 ) ;
#75491 = ORIENTED_EDGE ( 'NONE', *, *, #51601, .F. ) ;
#75492 = CARTESIAN_POINT ( 'NONE',  ( 22.88022663504679599, 2.825535151426334934, -1.500000000000002220 ) ) ;
#75493 = DIRECTION ( 'NONE',  ( 0.000000000000000000, -2.173523156925980399E-06, 0.9999999999976378895 ) ) ;
#75494 = CARTESIAN_POINT ( 'NONE',  ( -11.13811422090317294, 16.88724661786912762, -1.500000000000002220 ) ) ;
#75495 = CIRCLE ( 'NONE', #52776, 28.45799999999999486 ) ;
#75496 = VERTEX_POINT ( 'NONE', #29797 ) ;
#75497 = DIRECTION ( 'NONE',  ( -1.000000000000000000, -0.000000000000000000, -0.000000000000000000 ) ) ;
#75498 = CARTESIAN_POINT ( 'NONE',  ( -42.52287095715005449, -24.64965694238575011, 8.947790433994205372 ) ) ;
#75499 = VECTOR ( 'NONE', #55790, 1000.000000000000114 ) ;
#75500 = B_SPLINE_CURVE_WITH_KNOTS ( 'NONE', 3,
 ( #73278, #3772, #67668, #42835 ),
 .UNSPECIFIED., .F., .F.,
 ( 4, 4 ),
 ( 1.583065275649749065E-09, 0.0004001880791969523793 ),
 .UNSPECIFIED. ) ;
#75501 = CARTESIAN_POINT ( 'NONE',  ( 7.749999999999998224, 23.99999999999999289, 2.100000000000000089 ) ) ;
#75502 = CARTESIAN_POINT ( 'NONE',  ( -67.52287095715006160, -24.65952944569304961, 1.056160979905697239 ) ) ;
#75504 = VERTEX_POINT ( 'NONE', #53152 ) ;
#75503 = CARTESIAN_POINT ( 'NONE',  ( -7.526967427842778946, 20.06989004931119425, 11.49999999999999645 ) ) ;
#75505 = FACE_OUTER_BOUND ( 'NONE', #59196, .T. ) ;
#75506 = CARTESIAN_POINT ( 'NONE',  ( -41.57628542697372609, -24.65952944569304606, 1.056160979905696351 ) ) ;
#75507 = EDGE_LOOP ( 'NONE', ( #21898, #61073, #28437, #90915 ) ) ;
#75508 = CARTESIAN_POINT ( 'NONE',  ( -9.423985339279758122, -18.44656043379632848, -1.500000000000002220 ) ) ;
#75509 = ADVANCED_FACE ( 'NONE', ( #91685 ), #79968, .F. ) ;
#75510 = PRODUCT_RELATED_PRODUCT_CATEGORY ( 'detail', '', ( #63584 ) ) ;
#75511 = ORIENTED_EDGE ( 'NONE', *, *, #9192, .T. ) ;
#75512 = CARTESIAN_POINT ( 'NONE',  ( 0.000000000000000000, 1.826774720514426464, 4.300000000000000711 ) ) ;
#75513 = EDGE_LOOP ( 'NONE', ( #777, #18111, #10619, #62087 ) ) ;
#75514 = CARTESIAN_POINT ( 'NONE',  ( 4.692776824272364422, -6.376774720514406525, 18.67160386110882442 ) ) ;
#75515 = EDGE_LOOP ( 'NONE', ( #42499, #69414, #59651 ) ) ;
#75516 = CARTESIAN_POINT ( 'NONE',  ( -12.59924929152775874, 16.77720732749412846, -1.500000000000002220 ) ) ;
#75517 = CARTESIAN_POINT ( 'NONE',  ( 17.58553779993395594, 13.13030503331179411, 11.49999999999999645 ) ) ;
#75518 = CARTESIAN_POINT ( 'NONE',  ( -73.55905819736636886, -23.73791477778911840, 11.05961554403170766 ) ) ;
#75519 = CARTESIAN_POINT ( 'NONE',  ( -11.58057713800463162, -19.31455136971746001, -1.500000000000002220 ) ) ;
#75520 = ADVANCED_FACE ( 'NONE', ( #86580 ), #9459, .T. ) ;
#75521 = CIRCLE ( 'NONE', #70922, 2.499999999999998668 ) ;
#75522 = CARTESIAN_POINT ( 'NONE',  ( -17.07941033872765146, 12.18221932706078370, -1.500000000000002220 ) ) ;
#75523 = CARTESIAN_POINT ( 'NONE',  ( 5.872047395031165351, -6.376774720514415407, 20.29192741308114734 ) ) ;
#75524 = FACE_OUTER_BOUND ( 'NONE', #74602, .T. ) ;
#75525 = CARTESIAN_POINT ( 'NONE',  ( -30.64643973578111158, -23.50395946778992240, -1.461890965025843814 ) ) ;
#75526 = VERTEX_POINT ( 'NONE', #25683 ) ;
#75527 = ORIENTED_EDGE ( 'NONE', *, *, #32113, .T. ) ;
#75528 = VERTEX_POINT ( 'NONE', #62770 ) ;
#75529 = CARTESIAN_POINT ( 'NONE',  ( -128.6228709571500417, -23.48786465467242479, 11.44779295918253403 ) ) ;
#75530 = CARTESIAN_POINT ( 'NONE',  ( 19.32660459246815421, -9.429101867163046435, -1.500000000000002220 ) ) ;
#75531 = LINE ( 'NONE', #89781, #37555 ) ;
#75532 = ORIENTED_EDGE ( 'NONE', *, *, #38073, .T. ) ;
#75533 = CARTESIAN_POINT ( 'NONE',  ( -8.144517828999388698, 19.50133175306300970, -1.500000000000002220 ) ) ;
#75534 = CARTESIAN_POINT ( 'NONE',  ( -52.62287095715007723, -23.95044443724992078, 10.65354141964650125 ) ) ;
#75535 = CARTESIAN_POINT ( 'NONE',  ( -81.88534077628074215, -25.24685308744633616, 6.293942982122114671 ) ) ;
#75536 = CARTESIAN_POINT ( 'NONE',  ( -83.50334353477138905, -24.51419770103157347, 9.386484678747180510 ) ) ;
#75537 = CARTESIAN_POINT ( 'NONE',  ( -33.52287095715006160, -24.66019654487198665, 8.947790411086131712 ) ) ;
#75538 = CARTESIAN_POINT ( 'NONE',  ( -99.13348957873378708, -25.24983560723895692, 3.836871924205407680 ) ) ;
#75539 = CARTESIAN_POINT ( 'NONE',  ( -10.67647856527443473, 19.39090429279614369, -1.500000000000002220 ) ) ;
#75540 = CARTESIAN_POINT ( 'NONE',  ( -81.62637662810675465, -24.51419770103159834, 9.386484678747182286 ) ) ;
#75541 = ADVANCED_FACE ( 'NONE', ( #41417 ), #1979, .T. ) ;
#75542 = ORIENTED_EDGE ( 'NONE', *, *, #77185, .T. ) ;
#75543 = CARTESIAN_POINT ( 'NONE',  ( -2.806649551956928335, -6.376774720514411854, 19.35116211686183618 ) ) ;
#75544 = DIRECTION ( 'NONE',  ( 0.000000000000000000, 0.9999999999976377785, 2.173523156925979975E-06 ) ) ;
#75545 = DIRECTION ( 'NONE',  ( -0.9980236263794188822, 0.000000000000000000, 0.06283980576413539243 ) ) ;
#75546 = CARTESIAN_POINT ( 'NONE',  ( -100.5497506620879165, -24.52300882791530512, 0.6510814631126384810 ) ) ;
#75547 = CARTESIAN_POINT ( 'NONE',  ( -19.39930850525863804, 0.8904154686948315689, 11.49999999999998934 ) ) ;
#75548 = CARTESIAN_POINT ( 'NONE',  ( -2.881439591185620319, 21.19155266312798958, -1.500000000000002220 ) ) ;
#75549 = CARTESIAN_POINT ( 'NONE',  ( -73.62287095715005592, -24.64965695001468404, 8.947790433994184056 ) ) ;
#75550 = FACE_OUTER_BOUND ( 'NONE', #48994, .T. ) ;
#75551 = ADVANCED_FACE ( 'NONE', ( #1361 ), #31802, .F. ) ;
#75552 = DIRECTION ( 'NONE',  ( 0.000000000000000000, 0.000000000000000000, -1.000000000000000000 ) ) ;
#75554 = B_SPLINE_CURVE_WITH_KNOTS ( 'NONE', 3,
 ( #64583, #26989, #11260, #94992 ),
 .UNSPECIFIED., .F., .F.,
 ( 4, 4 ),
 ( 0.000000000000000000, 9.999999999999592548E-05 ),
 .UNSPECIFIED. ) ;
#75553 = DIRECTION ( 'NONE',  ( -1.000000000000000000, -0.000000000000000000, -0.000000000000000000 ) ) ;
#75555 = CARTESIAN_POINT ( 'NONE',  ( -22.51868310087907687, -2.221351303042197411, -1.500000000000002220 ) ) ;
#75556 = AXIS2_PLACEMENT_3D ( 'NONE', #1255, #8350, #47422 ) ;
#75557 = VERTEX_POINT ( 'NONE', #71871 ) ;
#75558 = CIRCLE ( 'NONE', #70722, 1.050000000000000488 ) ;
#75559 = DIRECTION ( 'NONE',  ( -0.000000000000000000, 1.000000000000000000, -0.000000000000000000 ) ) ;
#75560 = CARTESIAN_POINT ( 'NONE',  ( -41.52287095715006870, -23.47596703998600631, 11.44779298504229281 ) ) ;
#75561 = CARTESIAN_POINT ( 'NONE',  ( 18.46520180437041603, 7.126043738416648843, 11.49999999999999645 ) ) ;
#75562 = CARTESIAN_POINT ( 'NONE',  ( -74.52287095715007581, -23.48783264082476308, -1.443836473390090802 ) ) ;
#75563 = AXIS2_PLACEMENT_3D ( 'NONE', #138, #84373, #23452 ) ;
#75564 = DIRECTION ( 'NONE',  ( 0.000000000000000000, 0.000000000000000000, -1.000000000000000000 ) ) ;
#75565 = ORIENTED_EDGE ( 'NONE', *, *, #1310, .T. ) ;
#75566 = EDGE_CURVE ( 'NONE', #91875, #95021, #64783, .T. ) ;
#75567 = CARTESIAN_POINT ( 'NONE',  ( 15.10569527345119845, -2.682774720514426114, -27.29188918592609525 ) ) ;
#75568 = CARTESIAN_POINT ( 'NONE',  ( -87.55620429048339304, -23.47596703998600631, 11.44779298504227683 ) ) ;
#75569 = CARTESIAN_POINT ( 'NONE',  ( 13.31326451270642330, 17.06472021985377552, 11.49999999999998934 ) ) ;
#75570 = CARTESIAN_POINT ( 'NONE',  ( -19.77875734969026311, 6.143225279485574397, 27.31649921512899937 ) ) ;
#75572 = VECTOR ( 'NONE', #87714, 1000.000000000000000 ) ;
#75571 = CARTESIAN_POINT ( 'NONE',  ( 7.147005326088517130, -18.03964237587283037, -1.500000000000002220 ) ) ;
#75573 = CARTESIAN_POINT ( 'NONE',  ( -61.62287095715004881, -24.51283580621364777, 0.6167428607019832532 ) ) ;
#75574 = DIRECTION ( 'NONE',  ( -0.000000000000000000, 1.000000000000000000, -0.000000000000000000 ) ) ;
#75575 = CARTESIAN_POINT ( 'NONE',  ( 16.85830656838225039, -10.38424343889589707, -1.500000000000002220 ) ) ;
#75576 = ORIENTED_EDGE ( 'NONE', *, *, #50356, .T. ) ;
#75577 = CARTESIAN_POINT ( 'NONE',  ( 20.12614038868121824, 2.982395457389826809, 11.49999999999999645 ) ) ;
#75578 = CARTESIAN_POINT ( 'NONE',  ( -101.6228709571500559, -29.50250243563736774, 8.947779886222138046 ) ) ;
#75579 = DIRECTION ( 'NONE',  ( 1.000000000000000000, -3.639962309748244178E-15, 0.000000000000000000 ) ) ;
#75580 = VERTEX_POINT ( 'NONE', #94185 ) ;
#75581 = CARTESIAN_POINT ( 'NONE',  ( -30.64427850938830389, -23.56000036390796382, -1.497999999999532150 ) ) ;
#75582 = CARTESIAN_POINT ( 'NONE',  ( -111.5122638532038337, -25.29712067403331233, 4.332404411321261861 ) ) ;
#75583 = CARTESIAN_POINT ( 'NONE',  ( -99.58953762381672448, -23.48786465467241769, 11.44779295918254114 ) ) ;
#75584 = CARTESIAN_POINT ( 'NONE',  ( -82.52287095715006160, -23.48786465467241058, 11.44779295918254469 ) ) ;
#75585 = CARTESIAN_POINT ( 'NONE',  ( 30.77564450787170003, -1.477225279485574028, -9.689394075852828081 ) ) ;
#75586 = CARTESIAN_POINT ( 'NONE',  ( -1.723993941171178879, -19.98520929721398431, 11.49999999999998934 ) ) ;
#75587 = CARTESIAN_POINT ( 'NONE',  ( -95.55620429048340725, -24.99132157543166954, 2.256160258750667946 ) ) ;
#75588 = ORIENTED_EDGE ( 'NONE', *, *, #74880, .T. ) ;
#75589 = CARTESIAN_POINT ( 'NONE',  ( -117.6228709571500701, -24.50321055353806088, 9.387540953477516936 ) ) ;
#75590 = VECTOR ( 'NONE', #73169, 1000.000000000000114 ) ;
#75591 = CARTESIAN_POINT ( 'NONE',  ( 4.181975289622855918, -22.47981636197143374, 11.49999999999999645 ) ) ;
#75592 = CARTESIAN_POINT ( 'NONE',  ( -30.47287095715008931, -25.29726141536321293, 4.434337432396732837 ) ) ;
#75593 = CARTESIAN_POINT ( 'NONE',  ( -4.141025641025641413, -6.376774720514420736, 20.67377804487180271 ) ) ;
#75594 = LINE ( 'NONE', #6097, #50066 ) ;
#75595 = CARTESIAN_POINT ( 'NONE',  ( 30.54789914928607431, -0.2637885907592280588, 23.75907673500033113 ) ) ;
#75596 = DIRECTION ( 'NONE',  ( -1.000000000000000000, -3.773278334444167608E-23, -8.201307833595939069E-29 ) ) ;
#75597 = ADVANCED_FACE ( 'NONE', ( #10454 ), #25177, .F. ) ;
#75598 = CYLINDRICAL_SURFACE ( 'NONE', #25805, 2.499999999999998668 ) ;
#75599 = ORIENTED_EDGE ( 'NONE', *, *, #46036, .F. ) ;
#75600 = CARTESIAN_POINT ( 'NONE',  ( -18.95781532540867076, -7.450117396690965066, -1.500000000000002220 ) ) ;
#75601 = EDGE_LOOP ( 'NONE', ( #5367, #16614, #13664, #95157 ) ) ;
#75602 = CARTESIAN_POINT ( 'NONE',  ( 16.23347398924790497, -16.23827457187686463, -1.500000000000002220 ) ) ;
#75603 = DIRECTION ( 'NONE',  ( -0.000000000000000000, 1.000000000000000000, -0.000000000000000000 ) ) ;
#75604 = ORIENTED_EDGE ( 'NONE', *, *, #37907, .T. ) ;
#75605 = CARTESIAN_POINT ( 'NONE',  ( -101.5468792378191978, -25.24282061761980955, 6.236250683194342059 ) ) ;
#75606 = CIRCLE ( 'NONE', #18911, 84.48086791635431325 ) ;
#75607 = CARTESIAN_POINT ( 'NONE',  ( 22.02124265030973760, -7.835183881457444599, 16.20402280011862217 ) ) ;
#75608 = B_SPLINE_CURVE_WITH_KNOTS ( 'NONE', 3,
 ( #16647, #15649, #46618, #78032 ),
 .UNSPECIFIED., .F., .F.,
 ( 4, 4 ),
 ( 0.5001430643975933732, 0.5091494956697090180 ),
 .UNSPECIFIED. ) ;
#75609 = CARTESIAN_POINT ( 'NONE',  ( -86.62287095715004170, -24.65952944569304606, 1.056160979905700348 ) ) ;
#75611 = ORIENTED_EDGE ( 'NONE', *, *, #98456, .T. ) ;
#75610 = CARTESIAN_POINT ( 'NONE',  ( 10.81949470224598997, -18.29866561848832518, 11.49999999999999645 ) ) ;
#75612 = ORIENTED_EDGE ( 'NONE', *, *, #95148, .T. ) ;
#75613 = CARTESIAN_POINT ( 'NONE',  ( 19.86420646539740176, -9.926203236129387264, 11.49999999999998934 ) ) ;
#75614 = CARTESIAN_POINT ( 'NONE',  ( -20.60669311552257810, 0.8253496925510150906, -1.500000000000002220 ) ) ;
#75615 = CIRCLE ( 'NONE', #88615, 3.500000000000000000 ) ;
#75616 = ADVANCED_FACE ( 'NONE', ( #56654 ), #92873, .T. ) ;
#75617 = B_SPLINE_CURVE_WITH_KNOTS ( 'NONE', 3,
 ( #73279, #88003, #18482, #34712, #94606, #3282 ),
 .UNSPECIFIED., .F., .F.,
 ( 4, 2, 4 ),
 ( 0.000000000000000000, 0.001380764517854761930, 0.002761529035709523860 ),
 .UNSPECIFIED. ) ;
#75618 = ORIENTED_EDGE ( 'NONE', *, *, #13274, .F. ) ;
#75619 = EDGE_LOOP ( 'NONE', ( #24466, #4764, #50096, #60415 ) ) ;
#75620 = DIRECTION ( 'NONE',  ( 4.095491270384932624E-17, 0.5144957554275265688, -0.8574929257125440962 ) ) ;
#75621 = CARTESIAN_POINT ( 'NONE',  ( 2.832419239133125544, -5.876774720514421624, 21.23415460623727213 ) ) ;
#75622 = ORIENTED_EDGE ( 'NONE', *, *, #64838, .F. ) ;
#75623 = ADVANCED_FACE ( 'NONE', ( #68121 ), #89458, .T. ) ;
#75624 = VECTOR ( 'NONE', #95619, 1000.000000000000227 ) ;
#75625 = AXIS2_PLACEMENT_3D ( 'NONE', #61579, #53962, #80793 ) ;
#75626 = ORIENTED_EDGE ( 'NONE', *, *, #74744, .F. ) ;
#75627 = CARTESIAN_POINT ( 'NONE',  ( -6.660000000000001030, -10.15233964170348457, 1.310587897985993955 ) ) ;
#75628 = CARTESIAN_POINT ( 'NONE',  ( -111.5172617135973354, -24.15620529776629510, 10.23563542870659582 ) ) ;
#75629 = CARTESIAN_POINT ( 'NONE',  ( 14.78821595474767747, -4.792189181182639146, -27.68628040864140516 ) ) ;
#75630 = CARTESIAN_POINT ( 'NONE',  ( 16.93201058511109380, 12.15574511561022852, -1.500000000000002220 ) ) ;
#75631 = CARTESIAN_POINT ( 'NONE',  ( 16.38291735060997567, -14.39268585342195905, 11.49999999999999645 ) ) ;
#75632 = CARTESIAN_POINT ( 'NONE',  ( -51.16262983862578295, -25.06317656708942820, 7.418605103709588811 ) ) ;
#75633 = CARTESIAN_POINT ( 'NONE',  ( -52.52287095715009002, -24.33832256527048088, 0.1851278514138577636 ) ) ;
#75634 = CARTESIAN_POINT ( 'NONE',  ( 11.36419782745769069, 19.35538867594532775, -1.500000000000002220 ) ) ;
#75635 = EDGE_CURVE ( 'NONE', #53330, #55838, #58680, .T. ) ;
#75636 = CIRCLE ( 'NONE', #12261, 9.999999999999991118 ) ;
#75637 = ADVANCED_FACE ( 'NONE', ( #98047 ), #66647, .F. ) ;
#75638 = CARTESIAN_POINT ( 'NONE',  ( -3.108974358974355923, -6.376774720514427841, 21.75000000000001066 ) ) ;
#75639 = ORIENTED_EDGE ( 'NONE', *, *, #46717, .T. ) ;
#75640 = CARTESIAN_POINT ( 'NONE',  ( -75.52287095715009002, -24.82558206586143967, 1.605769216559449930 ) ) ;
#75641 = CARTESIAN_POINT ( 'NONE',  ( -50.38191529551148307, -25.11033443737753146, 2.832404817301930056 ) ) ;
#75642 = EDGE_CURVE ( 'NONE', #77501, #55598, #11660, .T. ) ;
#75643 = ORIENTED_EDGE ( 'NONE', *, *, #18756, .F. ) ;
#75644 = EDGE_LOOP ( 'NONE', ( #91495, #57545, #40834, #62219, #58506, #8745, #87618, #11146 ) ) ;
#75645 = FACE_OUTER_BOUND ( 'NONE', #67038, .T. ) ;
#75646 = ORIENTED_EDGE ( 'NONE', *, *, #82231, .T. ) ;
#75647 = CARTESIAN_POINT ( 'NONE',  ( -18.72683625574626376, -10.08736549105613278, -1.500000000000002220 ) ) ;
#75648 = EDGE_LOOP ( 'NONE', ( #49900, #89149, #37718, #94473 ) ) ;
#75649 = CARTESIAN_POINT ( 'NONE',  ( -6.680782769985652791, -5.876774720514411854, 19.46295461892502132 ) ) ;
#75650 = CARTESIAN_POINT ( 'NONE',  ( -2.129267666952235682, 20.92775224702969439, 11.49999999999998934 ) ) ;
#75651 = CARTESIAN_POINT ( 'NONE',  ( -55.62287095715004170, -23.47596703998600631, 11.44779298504227505 ) ) ;
#75652 = CARTESIAN_POINT ( 'NONE',  ( -100.4326965455115044, -25.18492896333868103, 3.293943116708551777 ) ) ;
#75653 = FACE_OUTER_BOUND ( 'NONE', #57683, .T. ) ;
#75654 = CARTESIAN_POINT ( 'NONE',  ( -17.33335002049248530, 13.43749923854009509, -1.500000000000002220 ) ) ;
#75655 = CARTESIAN_POINT ( 'NONE',  ( -87.55830571644068527, -23.73766607897671932, -1.055555164236430032 ) ) ;
#75656 = VERTEX_POINT ( 'NONE', #59018 ) ;
#75657 = CARTESIAN_POINT ( 'NONE',  ( -122.6263441853496943, -23.73791477778912551, 11.05961554403169878 ) ) ;
#75658 = ADVANCED_FACE ( 'NONE', ( #6206 ), #37161, .T. ) ;
#75659 = CIRCLE ( 'NONE', #98407, 130.7884398600581335 ) ;
#75660 = CARTESIAN_POINT ( 'NONE',  ( -120.5228709571500758, -23.84047902841604483, -0.8780736468305403442 ) ) ;
#75661 = CARTESIAN_POINT ( 'NONE',  ( -39.52287095715008292, -23.48783264082476308, -1.443836473390098574 ) ) ;
#75662 = AXIS2_PLACEMENT_3D ( 'NONE', #94904, #55867, #16779 ) ;
#75663 = CARTESIAN_POINT ( 'NONE',  ( -30.61243602696747956, -24.47944986445295612, 9.440663514584128890 ) ) ;
#75664 = CARTESIAN_POINT ( 'NONE',  ( -13.45305159987462851, 16.49040971879131234, -1.500000000000002220 ) ) ;
#75665 = CARTESIAN_POINT ( 'NONE',  ( -47.62287095715004881, -24.66019654487199020, 8.947790411086133489 ) ) ;
#75666 = CARTESIAN_POINT ( 'NONE',  ( -107.6339985510269059, -23.48786465467241413, 11.44779295918253759 ) ) ;
#75667 = EDGE_CURVE ( 'NONE', #71524, #68399, #60362, .T. ) ;
#75668 = CARTESIAN_POINT ( 'NONE',  ( -29.62287096154833677, -23.39681786206389447, 11.44779298504227860 ) ) ;
#75669 = CARTESIAN_POINT ( 'NONE',  ( -33.51256534245839447, -23.73766607897670866, -1.055555164236444687 ) ) ;
#75670 = CARTESIAN_POINT ( 'NONE',  ( -9.984083066403742990, 20.14924292131567185, -1.500000000000002220 ) ) ;
#75671 = B_SPLINE_SURFACE_WITH_KNOTS ( 'NONE', 3, 1, ( 
 ( #35155, #64632 ),
 ( #41266, #4201 ),
 ( #57003, #34158 ),
 ( #33143, #17421 ),
 ( #40759, #10811 ),
 ( #2712, #42775 ),
 ( #88441, #72219 ),
 ( #18914, #26030 ),
 ( #96048, #73708 ),
 ( #17927, #66126 ),
 ( #81321, #79313 ),
 ( #26542, #2214 ),
 ( #87938, #95546 ),
 ( #11802, #48884 ),
 ( #3221, #86928 ),
 ( #49893, #9808 ),
 ( #33652, #25028 ),
 ( #56002, #64126 ),
 ( #79812, #18422 ) ),
 .UNSPECIFIED., .F., .F., .F.,
 ( 4, 1, 1, 1, 1, 1, 1, 1, 1, 1, 1, 1, 1, 1, 1, 1, 4 ),
 ( 2, 2 ),
 ( 0.000000000000000000, 0.06542114375888925804, 0.1287083718818818057, 0.1902361418635387103, 0.2507244020335389068, 0.3106371794134432096, 0.3707664082897241253, 0.4316147444123512589, 0.4935229735663542727, 0.5558834553775323650, 0.6173423673185097771, 0.6786680390972755772, 0.7407113595451459975, 0.8029853625127446604, 0.8668025802655175971, 0.9323471713458875154, 1.000000000000000000 ),
 ( 0.000000000000000000, 1.000000000000000000 ),
 .UNSPECIFIED. ) ;
#75672 = EDGE_CURVE ( 'NONE', #70772, #35113, #36661, .T. ) ;
#75673 = CARTESIAN_POINT ( 'NONE',  ( -57.52287095715008292, -23.47593901973090524, -1.443836447538997092 ) ) ;
#75674 = ORIENTED_EDGE ( 'NONE', *, *, #52862, .F. ) ;
#75675 = FACE_OUTER_BOUND ( 'NONE', #66547, .T. ) ;
#75676 = CARTESIAN_POINT ( 'NONE',  ( -15.21066300689680872, 12.40131300380995860, 11.49999999999999645 ) ) ;
#75677 = CARTESIAN_POINT ( 'NONE',  ( -78.52287095715004739, -24.66019654487199375, 8.947790411086119278 ) ) ;
#75678 = CARTESIAN_POINT ( 'NONE',  ( -82.52287095715000476, -24.34917612407037524, 0.1852690917478629073 ) ) ;
#75679 = EDGE_LOOP ( 'NONE', ( #61169, #45249, #69416, #82274 ) ) ;
#75680 = EDGE_CURVE ( 'NONE', #52968, #57568, #16934, .T. ) ;
#75681 = CARTESIAN_POINT ( 'NONE',  ( -88.54822851708769349, -24.35071581493543746, 9.817618358456025263 ) ) ;
#75682 = CARTESIAN_POINT ( 'NONE',  ( -108.6228709571500417, -24.66019654487199730, 8.947790411086124607 ) ) ;
#75683 = CARTESIAN_POINT ( 'NONE',  ( -99.38203303823797796, -25.25095903933959463, 5.782495831883606385 ) ) ;
#75684 = VECTOR ( 'NONE', #72457, 1000.000000000000227 ) ;
#75686 = EDGE_CURVE ( 'NONE', #35831, #56695, #98001, .T. ) ;
#75685 = CARTESIAN_POINT ( 'NONE',  ( -26.36060433830035876, -24.68582954907684268, 7.705587838995554328 ) ) ;
#75687 = CARTESIAN_POINT ( 'NONE',  ( -16.88869819569221065, 10.18974688345344148, -1.500000000000002220 ) ) ;
#75688 = EDGE_CURVE ( 'NONE', #31325, #83369, #5966, .T. ) ;
#75689 = ORIENTED_EDGE ( 'NONE', *, *, #29834, .T. ) ;
#75690 = LINE ( 'NONE', #59999, #47235 ) ;
#75691 = DIRECTION ( 'NONE',  ( 0.000000000000000000, 0.000000000000000000, 1.000000000000000000 ) ) ;
#75692 = CIRCLE ( 'NONE', #88692, 251.9358649670780892 ) ;
#75693 = APPROVAL_STATUS ( 'not_yet_approved' ) ;
#75694 = ORIENTED_EDGE ( 'NONE', *, *, #65048, .T. ) ;
#75695 = CARTESIAN_POINT ( 'NONE',  ( -124.5228709571500616, -23.47596703998600631, 11.44779298504227860 ) ) ;
#75696 = CARTESIAN_POINT ( 'NONE',  ( -1.359786310227693251, -6.376774720514417183, 20.62654306927474579 ) ) ;
#75697 = CARTESIAN_POINT ( 'NONE',  ( 282.9764569301858046, 3.316774720514426900, 20.79159422840526616 ) ) ;
#75698 = DIRECTION ( 'NONE',  ( 0.000000000000000000, 0.000000000000000000, -1.000000000000000000 ) ) ;
#75699 = CARTESIAN_POINT ( 'NONE',  ( -45.58953762381671737, -24.99156044556202261, 7.747789690856172307 ) ) ;
#75700 = VECTOR ( 'NONE', #50230, 1000.000000000000000 ) ;
#75701 = CARTESIAN_POINT ( 'NONE',  ( -119.5228709571500758, -23.47596703998600631, 11.44779298504227860 ) ) ;
#75702 = CARTESIAN_POINT ( 'NONE',  ( -120.5562042904833930, -23.47593901973091235, -1.443836447538997536 ) ) ;
#75703 = CARTESIAN_POINT ( 'NONE',  ( 19.86680303116296287, 2.261939200664708327, -1.500000000000002220 ) ) ;
#75704 = CARTESIAN_POINT ( 'NONE',  ( -125.6228709571500275, -24.92604778743017846, 8.074972756849355449 ) ) ;
#75705 = CARTESIAN_POINT ( 'NONE',  ( -89.40841769935767047, -29.50249691823240994, 6.409318347766594037 ) ) ;
#75706 = ORIENTED_EDGE ( 'NONE', *, *, #35569, .F. ) ;
#75707 = DIRECTION ( 'NONE',  ( -0.000000000000000000, -1.000000000000000000, -0.000000000000000000 ) ) ;
#75708 = CARTESIAN_POINT ( 'NONE',  ( -107.5228709571501042, -23.47593901973090524, -1.443836447538996426 ) ) ;
#75709 = CARTESIAN_POINT ( 'NONE',  ( -80.55273171905794527, -24.15602025860895807, 10.28564288303536145 ) ) ;
#75710 = CARTESIAN_POINT ( 'NONE',  ( -49.62287095715005592, -23.73934037231756733, 11.05740245334328975 ) ) ;
#75711 = CARTESIAN_POINT ( 'NONE',  ( -81.50567729269914707, -24.34968618360933945, 0.1864209137778954084 ) ) ;
#75712 = CARTESIAN_POINT ( 'NONE',  ( -27.75512989467660674, -24.60093890593964261, 1.629583950786930968 ) ) ;
#75713 = CARTESIAN_POINT ( 'NONE',  ( -45.52287095715007581, -25.00182538069144655, 7.747789668545101094 ) ) ;
#75714 = CARTESIAN_POINT ( 'NONE',  ( 0.000000000000000000, -7.835183881457442823, 0.000000000000000000 ) ) ;
#75715 = CARTESIAN_POINT ( 'NONE',  ( -127.5212392067688540, -24.34968618360935011, 0.1864209137778923830 ) ) ;
#75716 = ORIENTED_EDGE ( 'NONE', *, *, #70416, .T. ) ;
#75717 = CARTESIAN_POINT ( 'NONE',  ( -11.05657426389776354, 17.00066307926000420, 11.49999999999998934 ) ) ;
#75718 = CARTESIAN_POINT ( 'NONE',  ( -70.18583440245234328, -25.31468095713259103, 4.854010836220668423 ) ) ;
#75719 = CARTESIAN_POINT ( 'NONE',  ( 22.11414358107865397, 4.215138183568805985, -16.31598992311990415 ) ) ;
#75720 = VECTOR ( 'NONE', #44235, 1000.000000000000000 ) ;
#75721 = CARTESIAN_POINT ( 'NONE',  ( -27.96875734969026084, -6.143225279485574397, 23.50402280011861933 ) ) ;
#75722 = ORIENTED_EDGE ( 'NONE', *, *, #95020, .F. ) ;
#75723 = DIRECTION ( 'NONE',  ( -1.000000000000000000, -3.773278334444167608E-23, -8.201307833595939069E-29 ) ) ;
#75724 = CARTESIAN_POINT ( 'NONE',  ( -51.62287095715005592, -29.50248528299804818, 1.056150453629033370 ) ) ;
#75725 = CARTESIAN_POINT ( 'NONE',  ( -12.53166870608491479, 15.75175023352509385, -1.500000000000002220 ) ) ;
#75726 = CARTESIAN_POINT ( 'NONE',  ( 9.660767377612277329, -18.76748907076374095, 11.49999999999999645 ) ) ;
#75728 = MANIFOLD_SOLID_BREP ( 'Kes-Ekstr\X2\00fc\X0\zyon3', #51698 ) ;
#75727 = AXIS2_PLACEMENT_3D ( 'NONE', #85041, #69324, #86547 ) ;
#75729 = CARTESIAN_POINT ( 'NONE',  ( 8.000000000000003553, -5.876774720514426953, 0.000000000000000000 ) ) ;
#75730 = CARTESIAN_POINT ( 'NONE',  ( -70.56769529849768219, -23.48786465467241058, 11.44779295918254824 ) ) ;
#75731 = CARTESIAN_POINT ( 'NONE',  ( -20.36895902721504825, -8.506870616244709637, -1.500000000000002220 ) ) ;
#75732 = CARTESIAN_POINT ( 'NONE',  ( -4.863915844574979275, 19.94883092034378791, 11.49999999999998934 ) ) ;
#75733 = CARTESIAN_POINT ( 'NONE',  ( -35.55620429048339304, -24.99132157543166244, 2.256160258750668390 ) ) ;
#75734 = EDGE_CURVE ( 'NONE', #24351, #62056, #87862, .T. ) ;
#75735 = DIRECTION ( 'NONE',  ( 1.000000000000000000, 0.000000000000000000, 0.000000000000000000 ) ) ;
#75736 = VERTEX_POINT ( 'NONE', #30497 ) ;
#75737 = CARTESIAN_POINT ( 'NONE',  ( -28.47875734969026240, -5.965225279485572685, 26.43402280011862615 ) ) ;
#75738 = ORIENTED_EDGE ( 'NONE', *, *, #70764, .F. ) ;
#75739 = CARTESIAN_POINT ( 'NONE',  ( 21.57151214508649772, 3.625915217019311583E-15, 0.000000000000000000 ) ) ;
#75740 = CARTESIAN_POINT ( 'NONE',  ( -129.6228709571500417, -23.47596703998600631, 11.44779298504227683 ) ) ;
#75741 = EDGE_CURVE ( 'NONE', #75171, #53102, #48, .T. ) ;
#75742 = EDGE_LOOP ( 'NONE', ( #40836, #55471, #53432, #66106 ) ) ;
#75743 = VERTEX_POINT ( 'NONE', #37615 ) ;
#75744 = LINE ( 'NONE', #13851, #35645 ) ;
#75745 = DIRECTION ( 'NONE',  ( -1.000000000000000000, -0.000000000000000000, -0.000000000000000000 ) ) ;
#75746 = CARTESIAN_POINT ( 'NONE',  ( -0.2112149364088803105, -6.376774720514410077, 19.49357334786886398 ) ) ;
#75747 = CARTESIAN_POINT ( 'NONE',  ( 19.36870410414886479, 7.000668502413378569, -1.500000000000002220 ) ) ;
#75748 = ADVANCED_FACE ( 'NONE', ( #76162 ), #99498, .T. ) ;
#75749 = CARTESIAN_POINT ( 'NONE',  ( -2.376235263977734657, 21.45616117177731041, 11.49999999999999645 ) ) ;
#75750 = ORIENTED_EDGE ( 'NONE', *, *, #31022, .T. ) ;
#75751 = CARTESIAN_POINT ( 'NONE',  ( -70.74026866089612042, -25.30511070033976395, 4.894904393956083233 ) ) ;
#75752 = DIRECTION ( 'NONE',  ( -1.000000000000000000, 0.000000000000000000, -0.000000000000000000 ) ) ;
#75753 = CARTESIAN_POINT ( 'NONE',  ( -7.140196579304709523, 21.16591527347414115, -1.500000000000002220 ) ) ;
#75754 = EDGE_CURVE ( 'NONE', #23443, #46454, #43544, .T. ) ;
#75755 = AXIS2_PLACEMENT_3D ( 'NONE', #91404, #96656, #6175 ) ;
#75756 = EDGE_CURVE ( 'NONE', #9193, #49692, #13763, .T. ) ;
#75757 = CARTESIAN_POINT ( 'NONE',  ( -74.62287095715005592, -29.50248528299804818, 1.056150453629036701 ) ) ;
#75758 = DIRECTION ( 'NONE',  ( -3.773278334453079030E-23, 0.9999999999976377785, 2.173523156925979128E-06 ) ) ;
#75759 = ORIENTED_EDGE ( 'NONE', *, *, #80632, .F. ) ;
#75760 = DIRECTION ( 'NONE',  ( 0.000000000000000000, 2.173523156925980399E-06, -0.9999999999976378895 ) ) ;
#75761 = LINE ( 'NONE', #46324, #71834 ) ;
#75762 = EDGE_CURVE ( 'NONE', #82244, #43107, #38108, .T. ) ;
#75763 = CARTESIAN_POINT ( 'NONE',  ( 19.40856703110355852, -7.758221025823637262, -1.500000000000002220 ) ) ;
#75764 = ORIENTED_EDGE ( 'NONE', *, *, #71100, .T. ) ;
#75766 = ORIENTED_EDGE ( 'NONE', *, *, #69276, .F. ) ;
#75765 = CARTESIAN_POINT ( 'NONE',  ( -86.50206692487462590, -24.65952944569304961, 1.056160979905701680 ) ) ;
#75767 = ORIENTED_EDGE ( 'NONE', *, *, #98562, .T. ) ;
#75768 = CARTESIAN_POINT ( 'NONE',  ( -100.5908655779713712, -24.40133493613050319, 9.663955038902802386 ) ) ;
#75769 = CARTESIAN_POINT ( 'NONE',  ( 6.139388171429570384, 20.22809724653347985, -1.500000000000002220 ) ) ;
#75770 = ORIENTED_EDGE ( 'NONE', *, *, #36044, .T. ) ;
#75771 = CARTESIAN_POINT ( 'NONE',  ( -117.5527649515685340, -24.51314013834316086, 0.6176544820404215042 ) ) ;
#75772 = CARTESIAN_POINT ( 'NONE',  ( -96.62287095715005592, -29.50247984919015209, -1.443849546365050029 ) ) ;
#75773 = CARTESIAN_POINT ( 'NONE',  ( -3.523925741820590929, 21.50064390955241578, -1.500000000000002220 ) ) ;
#75774 = CARTESIAN_POINT ( 'NONE',  ( 9.450000000000002842, -2.000000000000001332, 19.19609335255483629 ) ) ;
#75775 = VECTOR ( 'NONE', #86178, 1000.000000000000000 ) ;
#75776 = CARTESIAN_POINT ( 'NONE',  ( -76.55889698137454502, -23.73791477778911840, 11.05961554403170766 ) ) ;
#75777 = LINE ( 'NONE', #6276, #23811 ) ;
#75778 = CARTESIAN_POINT ( 'NONE',  ( -20.93004649427559016, -6.003493321846349318, -1.500000000000002220 ) ) ;
#75779 = CARTESIAN_POINT ( 'NONE',  ( -71.64734380851882634, -25.31639660058803543, 5.762066634805036003 ) ) ;
#75781 = ORIENTED_EDGE ( 'NONE', *, *, #5547, .T. ) ;
#75780 = CARTESIAN_POINT ( 'NONE',  ( 4.697571063781373013, 21.84268702631108994, 11.49999999999999645 ) ) ;
#75782 = CARTESIAN_POINT ( 'NONE',  ( -55.62287095715005592, -23.47593901973091235, -1.443836447539007972 ) ) ;
#75783 = DIRECTION ( 'NONE',  ( -1.000000000000000000, 0.000000000000000000, 0.000000000000000000 ) ) ;
#75784 = EDGE_CURVE ( 'NONE', #51543, #42958, #29994, .T. ) ;
#75785 = CARTESIAN_POINT ( 'NONE',  ( 32.33465265239741626, -4.457608646344818126, 0.9133233228923198777 ) ) ;
#75786 = ORIENTED_EDGE ( 'NONE', *, *, #49450, .T. ) ;
#75787 = B_SPLINE_CURVE_WITH_KNOTS ( 'NONE', 3,
 ( #49965, #65696, #97117, #41338 ),
 .UNSPECIFIED., .F., .F.,
 ( 4, 4 ),
 ( 0.000000000000000000, 9.999999999999592548E-05 ),
 .UNSPECIFIED. ) ;
#75788 = VERTEX_POINT ( 'NONE', #44740 ) ;
#75789 = EDGE_CURVE ( 'NONE', #85381, #99016, #59363, .T. ) ;
#75790 = ORIENTED_EDGE ( 'NONE', *, *, #55778, .F. ) ;
#75791 = DIRECTION ( 'NONE',  ( -0.000000000000000000, -1.000000000000000000, -0.000000000000000000 ) ) ;
#75792 = CARTESIAN_POINT ( 'NONE',  ( 16.79009078985406234, 12.93418496121567252, -1.500000000000002220 ) ) ;
#75793 = FACE_OUTER_BOUND ( 'NONE', #18399, .T. ) ;
#75794 = CARTESIAN_POINT ( 'NONE',  ( 8.286623624103266097E-13, -23.05000000000000426, -1.500000000000002220 ) ) ;
#75795 = EDGE_CURVE ( 'NONE', #73004, #95213, #65323, .T. ) ;
#75796 = CARTESIAN_POINT ( 'NONE',  ( -124.5228709571500616, -24.64898659630368627, 1.056161002820833028 ) ) ;
#75797 = PLANE ( 'NONE',  #44357 ) ;
#75798 = CARTESIAN_POINT ( 'NONE',  ( -14.46832242630667942, -12.86894606327920876, 11.49999999999998934 ) ) ;
#75799 = CARTESIAN_POINT ( 'NONE',  ( -38.52287095715006870, -24.50216790748204332, 0.6166512839542463986 ) ) ;
#75800 = ORIENTED_EDGE ( 'NONE', *, *, #80073, .F. ) ;
#75801 = CARTESIAN_POINT ( 'NONE',  ( -3.206006181753352724, -19.19236486397402430, 11.49999999999999645 ) ) ;
#75802 = CARTESIAN_POINT ( 'NONE',  ( -69.52287095715006160, -24.33832256527049154, 0.1851278514138574860 ) ) ;
#75803 = EDGE_LOOP ( 'NONE', ( #11604, #5291, #67019, #99945 ) ) ;
#75804 = CARTESIAN_POINT ( 'NONE',  ( 3.020285327128866992, -5.876774720514406525, 19.15473963397401391 ) ) ;
#75805 = DIRECTION ( 'NONE',  ( -3.773278334444167608E-23, 1.000000000000000000, 0.000000000000000000 ) ) ;
#75806 = VECTOR ( 'NONE', #38857, 1000.000000000000000 ) ;
#75807 = CARTESIAN_POINT ( 'NONE',  ( -65.05438548721849656, -5.356774720514425603, 23.50402280011858736 ) ) ;
#75809 = EDGE_CURVE ( 'NONE', #23547, #4551, #82788, .T. ) ;
#75808 = CARTESIAN_POINT ( 'NONE',  ( -30.64427850938831099, -23.47596703998600276, 11.44779298504227683 ) ) ;
#75810 = CARTESIAN_POINT ( 'NONE',  ( -14.21210043416151159, 13.53504130633199765, -1.500000000000002220 ) ) ;
#75811 = B_SPLINE_SURFACE_WITH_KNOTS ( 'NONE', 3, 1, ( 
 ( #87759, #48204 ),
 ( #57331, #72046 ),
 ( #1526, #41091 ),
 ( #2530, #64452 ),
 ( #49213, #32465 ),
 ( #88260, #71037 ),
 ( #80645, #64952 ),
 ( #63951, #95365 ),
 ( #48714, #18243 ),
 ( #33462, #11131 ),
 ( #56828, #9628 ),
 ( #80143, #10633 ),
 ( #41594, #79133 ),
 ( #3033, #42100 ),
 ( #55822, #71539 ) ),
 .UNSPECIFIED., .F., .F., .F.,
 ( 4, 1, 1, 1, 1, 1, 1, 1, 1, 1, 1, 1, 4 ),
 ( 2, 2 ),
 ( 0.000000000000000000, 0.1183849129606683315, 0.2344384882140509996, 0.3525851839391772602, 0.4731673593536162015, 0.5350581108286729393, 0.5975237332646003985, 0.6605170696247790740, 0.7251603465314728769, 0.7908841475025374379, 0.8587744642336310186, 0.9282339358416601405, 1.000000000000000000 ),
 ( 0.000000000000000000, 1.000000000000000000 ),
 .UNSPECIFIED. ) ;
#75812 = CARTESIAN_POINT ( 'NONE',  ( -33.62287095715005592, -23.48786465467240347, 11.44779295918255535 ) ) ;
#75813 = EDGE_LOOP ( 'NONE', ( #4742, #33519, #48222, #85989 ) ) ;
#75814 = CARTESIAN_POINT ( 'NONE',  ( -10.34410514300256523, -18.92461576200269491, -1.500000000000002220 ) ) ;
#75815 = DIRECTION ( 'NONE',  ( 0.000000000000000000, 0.000000000000000000, -1.000000000000000000 ) ) ;
#75816 = DIRECTION ( 'NONE',  ( 7.994117400814786717E-16, 0.000000000000000000, -1.000000000000000000 ) ) ;
#75817 = DIRECTION ( 'NONE',  ( 0.000000000000000000, -0.9999999999976377785, -2.173523156925979975E-06 ) ) ;
#75818 = EDGE_CURVE ( 'NONE', #1680, #94949, #21773, .T. ) ;
#75819 = CARTESIAN_POINT ( 'NONE',  ( -100.4326965455115044, -25.18439335745797436, 3.293943117872703663 ) ) ;
#75820 = CARTESIAN_POINT ( 'NONE',  ( -22.55714481399219906, -4.634528848986672500, -1.500000000000002220 ) ) ;
#75821 = APPROVAL_DATE_TIME ( #60130, #77331 ) ;
#75822 = DIRECTION ( 'NONE',  ( 0.000000000000000000, -1.000000000000000000, 0.000000000000000000 ) ) ;
#75823 = CARTESIAN_POINT ( 'NONE',  ( -88.62287095715004170, -23.47596703998600631, 11.44779298504227860 ) ) ;
#75824 = CARTESIAN_POINT ( 'NONE',  ( 11.25103634530202790, -16.72154935384561725, 11.49999999999999645 ) ) ;
#75825 = CARTESIAN_POINT ( 'NONE',  ( -84.62287095715008434, -23.95044443724992789, 10.65354141964649592 ) ) ;
#75826 = FACE_OUTER_BOUND ( 'NONE', #87009, .T. ) ;
#75827 = CARTESIAN_POINT ( 'NONE',  ( -4.854568188115255367, -5.876774720514410077, 19.46611907402017394 ) ) ;
#75828 = CARTESIAN_POINT ( 'NONE',  ( -118.6228709571500559, -29.50250786944525672, 11.44777988621622811 ) ) ;
#75829 = B_SPLINE_CURVE_WITH_KNOTS ( 'NONE', 3,
 ( #1114, #40176, #2127, #85845, #39663, #107 ),
 .UNSPECIFIED., .F., .F.,
 ( 4, 2, 4 ),
 ( 1.570887131794638196E-05, 0.001396322306279761073, 0.002776935741241575838 ),
 .UNSPECIFIED. ) ;
#75830 = CARTESIAN_POINT ( 'NONE',  ( -110.9011049686103263, -25.18425615697176667, 3.445933459401032906 ) ) ;
#75831 = EDGE_CURVE ( 'NONE', #28831, #803, #84686, .T. ) ;
#75832 = CARTESIAN_POINT ( 'NONE',  ( 14.69432462292611952, 13.40460087117274490, -1.500000000000002220 ) ) ;
#75833 = LINE ( 'NONE', #67250, #60940 ) ;
#75834 = CARTESIAN_POINT ( 'NONE',  ( -15.39140670439391378, -12.39996395878027791, -1.500000000000002220 ) ) ;
#75835 = AXIS2_PLACEMENT_3D ( 'NONE', #26788, #89191, #49149 ) ;
#75836 = DIRECTION ( 'NONE',  ( 0.000000000000000000, 1.478457507934778393E-16, -1.000000000000000000 ) ) ;
#75837 = CARTESIAN_POINT ( 'NONE',  ( -0.9078848932494473223, -6.376774720514411854, 19.67454710845354171 ) ) ;
#75838 = PLANE ( 'NONE',  #3757 ) ;
#75839 = CARTESIAN_POINT ( 'NONE',  ( 12.98984941077313415, -16.12360325096057423, 11.49999999999999645 ) ) ;
#75840 = CARTESIAN_POINT ( 'NONE',  ( -128.5562042904834357, -24.64965694238575722, 8.947790433994187609 ) ) ;
#75841 = AXIS2_PLACEMENT_3D ( 'NONE', #24473, #91985, #7748 ) ;
#75842 = CARTESIAN_POINT ( 'NONE',  ( 12.92500000000000249, 14.50000000000000000, 24.00000000000000000 ) ) ;
#75843 = CARTESIAN_POINT ( 'NONE',  ( -79.58953762381672448, -23.47596703998600276, 11.44779298504227683 ) ) ;
#75844 = B_SPLINE_CURVE_WITH_KNOTS ( 'NONE', 3,
 ( #27864, #16000, #99239, #76397 ),
 .UNSPECIFIED., .F., .F.,
 ( 4, 4 ),
 ( 0.000000000000000000, 1.000000000000000000 ),
 .UNSPECIFIED. ) ;
#75845 = CARTESIAN_POINT ( 'NONE',  ( 0.6941480231959694658, 22.73124288027050710, 11.49999999999999645 ) ) ;
#75846 = ORIENTED_EDGE ( 'NONE', *, *, #43975, .T. ) ;
#75847 = CARTESIAN_POINT ( 'NONE',  ( -78.58953762381671027, -24.65952944569304606, 1.056160979905698571 ) ) ;
#75848 = CARTESIAN_POINT ( 'NONE',  ( 29.71615239255367413, 4.563867803339911156, 27.78418661847934246 ) ) ;
#75849 = CARTESIAN_POINT ( 'NONE',  ( 9.409760114191467295, 17.86087837679851020, 11.49999999999998934 ) ) ;
#75850 = CARTESIAN_POINT ( 'NONE',  ( -63.49151771392492805, -24.65952944569304250, 1.056160979905695463 ) ) ;
#75851 = DIRECTION ( 'NONE',  ( -3.773278334444167608E-23, 1.000000000000000000, 0.000000000000000000 ) ) ;
#75852 = EDGE_LOOP ( 'NONE', ( #68439, #92565, #61045, #44923 ) ) ;
#75853 = ORIENTED_EDGE ( 'NONE', *, *, #62652, .F. ) ;
#75854 = CARTESIAN_POINT ( 'NONE',  ( -0.001774553997815280816, -6.376774720514413630, 19.59623724171353487 ) ) ;
#75855 = CARTESIAN_POINT ( 'NONE',  ( 1.119804705421552748, 22.86502198858056545, 11.49999999999998934 ) ) ;
#75856 = CARTESIAN_POINT ( 'NONE',  ( -111.3631985155635249, -25.27898041276672814, 4.195814472291353070 ) ) ;
#75857 = CARTESIAN_POINT ( 'NONE',  ( 17.62533924669398999, -12.40915598911231577, -1.500000000000002220 ) ) ;
#75858 = CIRCLE ( 'NONE', #83977, 1.020000000000000018 ) ;
#75859 = CARTESIAN_POINT ( 'NONE',  ( -123.5563712463038115, -23.73766607897670866, -1.055555164236449350 ) ) ;
#75860 = CARTESIAN_POINT ( 'NONE',  ( -34.53827696482609610, -24.34968618360933590, 0.1864209137778841396 ) ) ;
#75861 = CARTESIAN_POINT ( 'NONE',  ( 20.36350155627077640, -4.707376482769925374, 11.49999999999999645 ) ) ;
#75862 = VERTEX_POINT ( 'NONE', #16276 ) ;
#75863 = CARTESIAN_POINT ( 'NONE',  ( -43.52287095715004739, -23.48783264083374078, -1.443836473376152840 ) ) ;
#75864 = B_SPLINE_CURVE_WITH_KNOTS ( 'NONE', 3,
 ( #61291, #91216, #22190, #30824, #29320, #28827, #68883, #36933, #60292, #75981, #52664, #5984, #83095, #59792 ),
 .UNSPECIFIED., .F., .F.,
 ( 4, 2, 2, 2, 2, 2, 4 ),
 ( 6.992893892674702526E-18, 0.0001898996604258977995, 0.0003797993208517886059, 0.0007595986417035701646, 0.001139397962555351723, 0.001329297622981238762, 0.001519197283407126018 ),
 .UNSPECIFIED. ) ;
#75865 = CARTESIAN_POINT ( 'NONE',  ( -17.28599015371049674, 13.57978550619682956, -1.500000000000002220 ) ) ;
#75866 = CARTESIAN_POINT ( 'NONE',  ( -105.6281865643600497, -24.52399227489126687, 9.353111116836517525 ) ) ;
#75867 = CARTESIAN_POINT ( 'NONE',  ( -29.05583327267715532, -24.79700080848643040, 6.516963030855588812 ) ) ;
#75868 = VERTEX_POINT ( 'NONE', #38614 ) ;
#75869 = DIRECTION ( 'NONE',  ( 0.000000000000000000, 0.000000000000000000, 1.000000000000000000 ) ) ;
#75870 = EDGE_CURVE ( 'NONE', #89308, #27813, #2076, .T. ) ;
#75871 = PLANE ( 'NONE',  #75353 ) ;
#75872 = ORIENTED_EDGE ( 'NONE', *, *, #99713, .T. ) ;
#75873 = FACE_OUTER_BOUND ( 'NONE', #6890, .T. ) ;
#75874 = ADVANCED_FACE ( 'NONE', ( #63989 ), #16777, .T. ) ;
#75875 = ORIENTED_EDGE ( 'NONE', *, *, #7994, .F. ) ;
#75876 = ADVANCED_FACE ( 'NONE', ( #8674 ), #46738, .F. ) ;
#75877 = ORIENTED_EDGE ( 'NONE', *, *, #63427, .F. ) ;
#75878 = CARTESIAN_POINT ( 'NONE',  ( -106.6228709571501128, -23.73907113216991860, -1.053371485793221929 ) ) ;
#75879 = DIRECTION ( 'NONE',  ( -0.000000000000000000, 1.000000000000000000, -0.000000000000000000 ) ) ;
#75880 = DIRECTION ( 'NONE',  ( -0.000000000000000000, 1.000000000000000000, -0.000000000000000000 ) ) ;
#75881 = CARTESIAN_POINT ( 'NONE',  ( 14.85214116200856083, 13.97194181870810326, -1.500000000000002220 ) ) ;
#75882 = EDGE_CURVE ( 'NONE', #68195, #51970, #68379, .T. ) ;
#75883 = VERTEX_POINT ( 'NONE', #47236 ) ;
#75884 = CARTESIAN_POINT ( 'NONE',  ( -2.889365861140832159, -5.876774720514409189, 19.43823095447973870 ) ) ;
#75885 = CARTESIAN_POINT ( 'NONE',  ( -8.349999999999971223, 27.69999999999999574, 0.000000000000000000 ) ) ;
#75886 = EDGE_CURVE ( 'NONE', #49859, #66424, #2399, .T. ) ;
#75887 = CARTESIAN_POINT ( 'NONE',  ( 17.91726403014145319, 0.000000000000000000, -1.691563534834430227 ) ) ;
#75888 = CARTESIAN_POINT ( 'NONE',  ( -25.67463369986340993, -24.84696307844978946, 6.403790676681452965 ) ) ;
#75889 = ORIENTED_EDGE ( 'NONE', *, *, #25894, .F. ) ;
#75890 = DIRECTION ( 'NONE',  ( 1.000000000000000000, 3.773278334444166432E-23, 8.201307841325785021E-29 ) ) ;
#75891 = CARTESIAN_POINT ( 'NONE',  ( -28.79021057664958505, -24.63645989546533954, 7.906029157777645366 ) ) ;
#75892 = CARTESIAN_POINT ( 'NONE',  ( 14.74948264216024008, 14.65492983226340407, 11.49999999999998934 ) ) ;
#75893 = EDGE_LOOP ( 'NONE', ( #97392, #18945, #14910, #52336 ) ) ;
#75895 = EDGE_LOOP ( 'NONE', ( #15707, #85533, #46138, #76143 ) ) ;
#75894 = CARTESIAN_POINT ( 'NONE',  ( 4.486687842132109694, -6.376774720514410077, 18.98221446873611029 ) ) ;
#75896 = B_SPLINE_SURFACE_WITH_KNOTS ( 'NONE', 3, 1, ( 
 ( #30797, #100276 ),
 ( #13561, #22662 ),
 ( #5954, #68860 ),
 ( #67872, #52638 ),
 ( #98801, #23161 ),
 ( #6462, #61265 ),
 ( #83574, #60267 ),
 ( #53650, #53150 ),
 ( #14565, #30286 ),
 ( #84574, #69862 ),
 ( #37419, #45038 ),
 ( #76453, #38404 ),
 ( #54153, #99301 ),
 ( #60761, #91683 ),
 ( #85076, #99778 ),
 ( #15065, #46523 ),
 ( #46033, #76954 ),
 ( #7952, #38906 ),
 ( #342, #31290 ),
 ( #90699, #21177 ),
 ( #63775, #32794 ),
 ( #25175, #86578 ),
 ( #39904, #17569 ),
 ( #18069, #95197 ),
 ( #70869, #78956 ),
 ( #79467, #48031 ),
 ( #1359, #9958 ) ),
 .UNSPECIFIED., .F., .F., .F.,
 ( 4, 1, 1, 1, 1, 1, 1, 1, 1, 1, 1, 1, 1, 1, 1, 1, 1, 1, 1, 1, 1, 1, 1, 1, 4 ),
 ( 2, 2 ),
 ( 0.000000000000000000, 0.03382411656725048399, 0.06729808750146204499, 0.1002802584818396348, 0.1330193052712239643, 0.1657361602733768979, 0.1987916522134082209, 0.2323715308488600861, 0.2664085106932945202, 0.3010156638683363362, 0.3361963658896798268, 0.3719718800539335568, 0.4085735935688276088, 0.4463941065015575305, 0.4852253093620474411, 0.5253715673688824639, 0.5672243359416908604, 0.6110807138143398154, 0.6577496272202332239, 0.7070202039764021951, 0.7592353208322853986, 0.8144842367739216771, 0.8732268335334771869, 0.9349367103827220804, 1.000000000000000000 ),
 ( 0.000000000000000000, 1.000000000000000000 ),
 .UNSPECIFIED. ) ;
#75897 = CARTESIAN_POINT ( 'NONE',  ( -68.52287095715006160, -24.64965694238407323, 8.947790433994200043 ) ) ;
#75898 = ORIENTED_EDGE ( 'NONE', *, *, #57077, .F. ) ;
#75899 = ORIENTED_EDGE ( 'NONE', *, *, #24017, .F. ) ;
#75900 = LINE ( 'NONE', #69296, #21886 ) ;
#75901 = DIRECTION ( 'NONE',  ( 0.7071067811865476838, 0.000000000000000000, -0.7071067811865474617 ) ) ;
#75902 = CARTESIAN_POINT ( 'NONE',  ( 0.4325450954222598288, 0.000000000000000000, 0.000000000000000000 ) ) ;
#75903 = CARTESIAN_POINT ( 'NONE',  ( -106.6228709571500559, -29.50248528299804818, 1.056150453629043584 ) ) ;
#75904 = CARTESIAN_POINT ( 'NONE',  ( -92.54896780759155206, -24.35071581493542681, 9.817618358456023486 ) ) ;
#75905 = CARTESIAN_POINT ( 'NONE',  ( -95.62287095715005592, -23.47596703998600631, 11.44779298504227860 ) ) ;
#75907 = VERTEX_POINT ( 'NONE', #54856 ) ;
#75906 = CARTESIAN_POINT ( 'NONE',  ( 4.116201370682176730, 21.75534844777131838, 11.49999999999999645 ) ) ;
#75908 = DIRECTION ( 'NONE',  ( -0.1311553622875919756, 6.845827386180409975E-16, -0.9913618264504692190 ) ) ;
#75909 = CARTESIAN_POINT ( 'NONE',  ( -9.675873947287982446, 20.46574270456686406, -1.500000000000002220 ) ) ;
#75910 = AXIS2_PLACEMENT_3D ( 'NONE', #58013, #50391, #45761 ) ;
#75912 = ORIENTED_EDGE ( 'NONE', *, *, #68908, .F. ) ;
#75911 = CARTESIAN_POINT ( 'NONE',  ( -27.97447329329273558, -24.82855238255122998, 7.574514681721855602 ) ) ;
#75913 = ORIENTED_EDGE ( 'NONE', *, *, #45327, .F. ) ;
#75914 = CARTESIAN_POINT ( 'NONE',  ( -10.36589631659242627, -6.376774720514426065, 27.85486277704324110 ) ) ;
#75915 = CARTESIAN_POINT ( 'NONE',  ( -8.609638109768802394, 18.19638482192696216, -1.500000000000002220 ) ) ;
#75916 = CARTESIAN_POINT ( 'NONE',  ( 6.660000000000001030, 8.793627758918228565, -2.994553991265763049 ) ) ;
#75917 = ORIENTED_EDGE ( 'NONE', *, *, #1162, .T. ) ;
#75918 = VECTOR ( 'NONE', #16445, 1000.000000000000114 ) ;
#75919 = CARTESIAN_POINT ( 'NONE',  ( -103.6228709571500559, -24.64965695001469115, 8.947790433994178727 ) ) ;
#75920 = CARTESIAN_POINT ( 'NONE',  ( 12.52526618502215250, 18.50471055633022388, -1.500000000000002220 ) ) ;
#75921 = ORIENTED_EDGE ( 'NONE', *, *, #39676, .T. ) ;
#75922 = ORIENTED_EDGE ( 'NONE', *, *, #74447, .T. ) ;
#75923 = DIRECTION ( 'NONE',  ( 0.000000000000000000, 0.000000000000000000, 1.000000000000000000 ) ) ;
#75924 = FACE_OUTER_BOUND ( 'NONE', #23093, .T. ) ;
#75925 = DIRECTION ( 'NONE',  ( 0.000000000000000000, -1.000000000000000000, 0.000000000000000000 ) ) ;
#75926 = EDGE_CURVE ( 'NONE', #11110, #100229, #71582, .T. ) ;
#75927 = CARTESIAN_POINT ( 'NONE',  ( -96.62287095715015539, -24.35013146730205236, 9.818937971375108376 ) ) ;
#75928 = LINE ( 'NONE', #28270, #69082 ) ;
#75930 = AXIS2_PLACEMENT_3D ( 'NONE', #104, #39159, #70116 ) ;
#75929 = CARTESIAN_POINT ( 'NONE',  ( 12.07855387261060898, -15.37489856218140183, 11.49999999999998934 ) ) ;
#75931 = CARTESIAN_POINT ( 'NONE',  ( -85.62287095715005592, -29.50248528299804818, 1.056150453629040253 ) ) ;
#75932 = CARTESIAN_POINT ( 'NONE',  ( -10.41973078503355588, 18.78793304046337198, 11.49999999999998934 ) ) ;
#75933 = CARTESIAN_POINT ( 'NONE',  ( -25.68905881183481199, -24.92775057940327343, 3.430378144321810208 ) ) ;
#75934 = FACE_OUTER_BOUND ( 'NONE', #72653, .T. ) ;
#75935 = CARTESIAN_POINT ( 'NONE',  ( 3.509873074917118085, 0.3587747205144265483, 29.15869884040363758 ) ) ;
#75936 = EDGE_CURVE ( 'NONE', #85295, #3492, #40630, .T. ) ;
#75937 = CARTESIAN_POINT ( 'NONE',  ( -12.24191887126339751, 19.33842681661653984, -1.500000000000002220 ) ) ;
#75938 = EDGE_CURVE ( 'NONE', #11540, #78378, #77162, .T. ) ;
#75939 = LINE ( 'NONE', #35412, #93650 ) ;
#75940 = CARTESIAN_POINT ( 'NONE',  ( -91.52287095715006160, -23.48786465467241769, 11.44779295918254292 ) ) ;
#75941 = CARTESIAN_POINT ( 'NONE',  ( -19.59816365915598979, -3.832847594873297403, 11.49999999999999645 ) ) ;
#75942 = CARTESIAN_POINT ( 'NONE',  ( -64.62287095715005592, -24.64898659630528499, 1.056161002820822592 ) ) ;
#75943 = B_SPLINE_CURVE_WITH_KNOTS ( 'NONE', 3,
 ( #69128, #15330, #25340, #76719 ),
 .UNSPECIFIED., .F., .F.,
 ( 4, 4 ),
 ( 0.000000000000000000, 9.999999999998897304E-05 ),
 .UNSPECIFIED. ) ;
#75944 = CARTESIAN_POINT ( 'NONE',  ( -74.63458368284264566, -24.15620529776628800, 10.23563542870659937 ) ) ;
#75945 = CARTESIAN_POINT ( 'NONE',  ( 2.872281323269014752, -16.94322527948557422, 1.999999999999999556 ) ) ;
#75946 = ORIENTED_EDGE ( 'NONE', *, *, #91723, .F. ) ;
#75947 = DIRECTION ( 'NONE',  ( 0.000000000000000000, -0.9999999999976377785, -2.173523156925979975E-06 ) ) ;
#75948 = DIRECTION ( 'NONE',  ( -1.000000000000000000, 0.000000000000000000, 0.000000000000000000 ) ) ;
#75949 = CARTESIAN_POINT ( 'NONE',  ( -21.72135255055207281, 0.4632500610043824851, 11.49999999999998934 ) ) ;
#75950 = LINE ( 'NONE', #60755, #15574 ) ;
#75951 = CARTESIAN_POINT ( 'NONE',  ( -16.13938233076020268, 11.07636124087057183, -1.500000000000002220 ) ) ;
#75952 = PLANE ( 'NONE',  #32906 ) ;
#75953 = ORIENTED_EDGE ( 'NONE', *, *, #23117, .F. ) ;
#75954 = COORDINATED_UNIVERSAL_TIME_OFFSET ( 0, 0, .AHEAD. ) ;
#75955 = CARTESIAN_POINT ( 'NONE',  ( -28.47875734969025885, 5.965225279485572685, -0.08597719988137125791 ) ) ;
#75956 = CARTESIAN_POINT ( 'NONE',  ( -71.70841769935766763, -25.25720466352798255, 6.192981421160952848 ) ) ;
#75957 = CARTESIAN_POINT ( 'NONE',  ( -1.317410511717131971, -20.46822056820986546, 11.49999999999999645 ) ) ;
#75958 = LINE ( 'NONE', #6464, #10078 ) ;
#75959 = B_SPLINE_CURVE_WITH_KNOTS ( 'NONE', 3,
 ( #66101, #97017, #65101, #56478, #88414, #96515 ),
 .UNSPECIFIED., .F., .F.,
 ( 4, 2, 4 ),
 ( 1.570755371633875854E-05, 0.001396183895866087970, 0.002776660238015836880 ),
 .UNSPECIFIED. ) ;
#75960 = LINE ( 'NONE', #90703, #88559 ) ;
#75961 = ORIENTED_EDGE ( 'NONE', *, *, #71933, .T. ) ;
#75962 = LINE ( 'NONE', #59771, #70250 ) ;
#75963 = LINE ( 'NONE', #53157, #2431 ) ;
#75964 = CARTESIAN_POINT ( 'NONE',  ( -116.5222327913904934, -23.48786465467241769, 11.44779295918253759 ) ) ;
#75965 = VECTOR ( 'NONE', #27768, 1000.000000000000000 ) ;
#75966 = LINE ( 'NONE', #59776, #37039 ) ;
#75967 = CARTESIAN_POINT ( 'NONE',  ( -124.6228709571499991, -24.51387760970725083, 9.387446482453405849 ) ) ;
#75968 = AXIS2_PLACEMENT_3D ( 'NONE', #23030, #8329, #39274 ) ;
#75969 = ADVANCED_FACE ( 'NONE', ( #1063 ), #78656, .T. ) ;
#75970 = CARTESIAN_POINT ( 'NONE',  ( 21.63105218614105851, 7.968772182826888262, 11.49999999999999645 ) ) ;
#75971 = CARTESIAN_POINT ( 'NONE',  ( 12.37853024107498534, -19.16169124346054176, -1.500000000000002220 ) ) ;
#75972 = FACE_OUTER_BOUND ( 'NONE', #43455, .T. ) ;
#75973 = CARTESIAN_POINT ( 'NONE',  ( -5.023036858974361252, -6.376774720514410077, 19.14743589743590846 ) ) ;
#75974 = CARTESIAN_POINT ( 'NONE',  ( -49.54611987101804971, -25.25386647804926099, 3.777482285138224150 ) ) ;
#75975 = VECTOR ( 'NONE', #13069, 1000.000000000000114 ) ;
#75976 = CARTESIAN_POINT ( 'NONE',  ( -115.5228709571501611, -24.92579138211019796, 1.929029949965660684 ) ) ;
#75977 = CARTESIAN_POINT ( 'NONE',  ( -99.37735140507533060, -25.30157721269421955, 5.086082750430767518 ) ) ;
#75978 = CARTESIAN_POINT ( 'NONE',  ( -0.1377007522546883911, -21.91379463844567965, 11.49999999999998934 ) ) ;
#75979 = DIRECTION ( 'NONE',  ( -0.9872275723272648795, 0.000000000000000000, -0.1593164160933056017 ) ) ;
#75980 = DIRECTION ( 'NONE',  ( 0.6392559695863496705, 0.000000000000000000, 0.7689940216596069522 ) ) ;
#75981 = CARTESIAN_POINT ( 'NONE',  ( -41.40626431004942276, -25.30540310050566077, 4.501526219705256793 ) ) ;
#75982 = CARTESIAN_POINT ( 'NONE',  ( -58.52287095715006160, -24.64898659630528499, 1.056161002820822592 ) ) ;
#75983 = CARTESIAN_POINT ( 'NONE',  ( -112.6228709571500417, -23.72747288104441665, -1.053458166803660889 ) ) ;
#75984 = CARTESIAN_POINT ( 'NONE',  ( -122.6228709571500417, -23.48786465467242124, 11.44779295918253759 ) ) ;
#75985 = VERTEX_POINT ( 'NONE', #40123 ) ;
#75986 = EDGE_CURVE ( 'NONE', #68982, #82055, #88298, .T. ) ;
#75987 = VECTOR ( 'NONE', #56805, 1000.000000000000000 ) ;
#75988 = CARTESIAN_POINT ( 'NONE',  ( 20.35601985306173134, -1.938729116259007679, -1.500000000000002220 ) ) ;
#75989 = ORIENTED_EDGE ( 'NONE', *, *, #16612, .F. ) ;
#75990 = VERTEX_POINT ( 'NONE', #31499 ) ;
#75991 = ORIENTED_EDGE ( 'NONE', *, *, #77257, .T. ) ;
#75992 = ORIENTED_EDGE ( 'NONE', *, *, #48402, .T. ) ;
#75993 = CARTESIAN_POINT ( 'NONE',  ( 3.314627170985911420, 22.80399709308638023, -1.500000000000002220 ) ) ;
#75994 = FACE_OUTER_BOUND ( 'NONE', #76187, .T. ) ;
#75995 = CARTESIAN_POINT ( 'NONE',  ( -17.27845874757997535, -10.49745931960568335, -1.500000000000002220 ) ) ;
#75996 = ADVANCED_FACE ( 'NONE', ( #54353 ), #1571, .F. ) ;
#75997 = ORIENTED_EDGE ( 'NONE', *, *, #83318, .F. ) ;
#75998 = CARTESIAN_POINT ( 'NONE',  ( -48.52287095715004028, -23.95044443724991723, 10.65354141964649237 ) ) ;
#75999 = CARTESIAN_POINT ( 'NONE',  ( -46.52287095715006160, -24.64898659630367561, 1.056161002820821038 ) ) ;
#76000 = EDGE_CURVE ( 'NONE', #65103, #81032, #554, .T. ) ;
#76001 = CARTESIAN_POINT ( 'NONE',  ( -0.02075734969026423599, 3.316774720514426456, -0.08597719988137648983 ) ) ;
#76002 = DIRECTION ( 'NONE',  ( 0.000000000000000000, -0.9999999999976377785, -2.173523156925979975E-06 ) ) ;
#76004 = ORIENTED_EDGE ( 'NONE', *, *, #33632, .F. ) ;
#76003 = CARTESIAN_POINT ( 'NONE',  ( -19.04320821261859464, -9.809917703373946196, 11.49999999999999645 ) ) ;
#76005 = DIRECTION ( 'NONE',  ( 0.000000000000000000, -1.000000000000000000, 0.000000000000000000 ) ) ;
#76006 = B_SPLINE_CURVE_WITH_KNOTS ( 'NONE', 3,
 ( #59403, #91841, #37059, #38056, #21320, #44183 ),
 .UNSPECIFIED., .F., .F.,
 ( 4, 2, 4 ),
 ( 6.391158118958419274E-06, 0.001387004593080778557, 0.002767618028042598960 ),
 .UNSPECIFIED. ) ;
#76007 = CARTESIAN_POINT ( 'NONE',  ( -61.62365995700092469, -24.66019654487199375, 8.947790411086119278 ) ) ;
#76008 = EDGE_CURVE ( 'NONE', #38439, #84685, #67846, .T. ) ;
#76009 = ORIENTED_EDGE ( 'NONE', *, *, #8562, .F. ) ;
#76010 = EDGE_CURVE ( 'NONE', #66631, #39813, #98262, .T. ) ;
#76011 = CARTESIAN_POINT ( 'NONE',  ( -9.423985339279758122, -18.44656043379632848, 11.49999999999998934 ) ) ;
#76014 = ORIENTED_EDGE ( 'NONE', *, *, #46036, .T. ) ;
#76013 = VECTOR ( 'NONE', #10440, 1000.000000000000000 ) ;
#76012 = CARTESIAN_POINT ( 'NONE',  ( -70.30743997983631743, -25.24386760754551418, 3.513016081743164598 ) ) ;
#76015 = CARTESIAN_POINT ( 'NONE',  ( -91.52287095715006160, -23.48786465467241769, 11.44779295918254292 ) ) ;
#76016 = ORIENTED_EDGE ( 'NONE', *, *, #67007, .T. ) ;
#76017 = CARTESIAN_POINT ( 'NONE',  ( 4.468667172983064262, -6.376774720514401196, 18.40700896291420463 ) ) ;
#76018 = VERTEX_POINT ( 'NONE', #41135 ) ;
#76019 = EDGE_CURVE ( 'NONE', #34838, #29304, #21417, .T. ) ;
#76020 = CARTESIAN_POINT ( 'NONE',  ( 19.17116566557315949, -10.70166234769870961, 11.49999999999999645 ) ) ;
#76021 = CARTESIAN_POINT ( 'NONE',  ( -37.60092905518352069, -23.96169478059712432, 10.65365249895718591 ) ) ;
#76022 = CARTESIAN_POINT ( 'NONE',  ( 19.88857169258762170, 10.62688394266798930, -1.500000000000002220 ) ) ;
#76023 = CARTESIAN_POINT ( 'NONE',  ( -15.18370147500227496, -14.46048895944246127, 11.49999999999998934 ) ) ;
#76024 = CARTESIAN_POINT ( 'NONE',  ( 5.641025641025643189, -5.876774720514419847, 20.78665865384615330 ) ) ;
#76025 = FACE_OUTER_BOUND ( 'NONE', #93909, .T. ) ;
#76026 = CARTESIAN_POINT ( 'NONE',  ( 5.641025641025643189, -6.376774720514420736, 20.78665865384615330 ) ) ;
#76027 = VERTEX_POINT ( 'NONE', #59225 ) ;
#76028 = ORIENTED_EDGE ( 'NONE', *, *, #92041, .F. ) ;
#76029 = ORIENTED_EDGE ( 'NONE', *, *, #45791, .F. ) ;
#76030 = CARTESIAN_POINT ( 'NONE',  ( -66.56566039321768358, -23.48783264082476308, -1.443836473390097463 ) ) ;
#76031 = CARTESIAN_POINT ( 'NONE',  ( 11.78165356204951131, -17.99452314462042324, -1.500000000000002220 ) ) ;
#76032 = CARTESIAN_POINT ( 'NONE',  ( -105.5228709571500900, -23.84081130425358097, 10.88220057483157888 ) ) ;
#76033 = EDGE_LOOP ( 'NONE', ( #38591, #26093, #79033, #49959 ) ) ;
#76034 = CARTESIAN_POINT ( 'NONE',  ( -9.089321149825819290, -19.05894737874082168, -1.500000000000002220 ) ) ;
#76035 = CARTESIAN_POINT ( 'NONE',  ( -83.55620429048340725, -24.64898659630529210, 1.056161002820828809 ) ) ;
#76036 = FACE_BOUND ( 'NONE', #5425, .T. ) ;
#76038 = CARTESIAN_POINT ( 'NONE',  ( -100.5228709571500900, -23.48783264082477018, -1.443836473390086583 ) ) ;
#76037 = VECTOR ( 'NONE', #58650, 1000.000000000000114 ) ;
#76039 = DIRECTION ( 'NONE',  ( 0.000000000000000000, 0.000000000000000000, 1.000000000000000000 ) ) ;
#76040 = CARTESIAN_POINT ( 'NONE',  ( -42.22287095715005734, -23.47593901973090169, -1.443836447538997980 ) ) ;
#76041 = CARTESIAN_POINT ( 'NONE',  ( -0.8124730928778809425, -22.15030348749839817, -1.500000000000002220 ) ) ;
#76042 = CARTESIAN_POINT ( 'NONE',  ( -8.151702937934075521, -9.871032969692315362, 1.282000701945956500 ) ) ;
#76043 = B_SPLINE_CURVE_WITH_KNOTS ( 'NONE', 3,
 ( #72601, #12175, #19290, #95427 ),
 .UNSPECIFIED., .F., .F.,
 ( 4, 4 ),
 ( 0.000000000000000000, 1.000000000000000000 ),
 .UNSPECIFIED. ) ;
#76044 = EDGE_CURVE ( 'NONE', #99009, #21700, #75424, .T. ) ;
#76045 = VERTEX_POINT ( 'NONE', #11172 ) ;
#76046 = CARTESIAN_POINT ( 'NONE',  ( -2.889365861140832159, -6.376774720514410077, 19.43823095447973870 ) ) ;
#76047 = DIRECTION ( 'NONE',  ( -0.000000000000000000, -1.000000000000000000, -0.000000000000000000 ) ) ;
#76048 = CARTESIAN_POINT ( 'NONE',  ( 30.53060340732035982, 4.751309003483179083, 17.08946163269322227 ) ) ;
#76049 = AXIS2_PLACEMENT_3D ( 'NONE', #31, #47213, #76635 ) ;
#76050 = EDGE_CURVE ( 'NONE', #41368, #46438, #41213, .T. ) ;
#76051 = PLANE ( 'NONE',  #28500 ) ;
#76052 = AXIS2_PLACEMENT_3D ( 'NONE', #90465, #45298, #22427 ) ;
#76053 = CARTESIAN_POINT ( 'NONE',  ( 12.19879910451502703, -15.15100395215988449, 11.49999999999998934 ) ) ;
#76054 = VECTOR ( 'NONE', #58295, 1000.000000000000227 ) ;
#76055 = CARTESIAN_POINT ( 'NONE',  ( 20.74164082462262471, 5.259929546262127609, -1.500000000000002220 ) ) ;
#76056 = CARTESIAN_POINT ( 'NONE',  ( -62.50954302324786482, -23.96119346886881019, -0.6495511937832096905 ) ) ;
#76057 = FACE_OUTER_BOUND ( 'NONE', #72681, .T. ) ;
#76058 = B_SPLINE_CURVE_WITH_KNOTS ( 'NONE', 3,
 ( #9602, #34442, #63413, #63919, #19200, #3004 ),
 .UNSPECIFIED., .F., .F.,
 ( 4, 2, 4 ),
 ( 0.000000000000000000, 0.001380901958385387027, 0.002761803916770774053 ),
 .UNSPECIFIED. ) ;
#76059 = EDGE_CURVE ( 'NONE', #6656, #25133, #3075, .T. ) ;
#76060 = CARTESIAN_POINT ( 'NONE',  ( -79.62287095715004170, -24.65952944569304606, 1.056160979905697461 ) ) ;
#76061 = FACE_OUTER_BOUND ( 'NONE', #52045, .T. ) ;
#76062 = CARTESIAN_POINT ( 'NONE',  ( 16.66146196086182130, -15.28366505690825328, -1.500000000000002220 ) ) ;
#76063 = CIRCLE ( 'NONE', #8132, 22.69500000000000384 ) ;
#76064 = ORIENTED_EDGE ( 'NONE', *, *, #65149, .T. ) ;
#76065 = ADVANCED_FACE ( 'NONE', ( #10172 ), #72087, .T. ) ;
#76066 = CARTESIAN_POINT ( 'NONE',  ( 30.53060340732036337, -1.477225279485574028, -8.442346167188908623 ) ) ;
#76067 = CARTESIAN_POINT ( 'NONE',  ( -40.62287095715005592, -23.47596703998600276, 11.44779298504227505 ) ) ;
#76068 = CARTESIAN_POINT ( 'NONE',  ( 19.51516567812286596, -3.327523070855789911, 11.49999999999999645 ) ) ;
#76069 = DIRECTION ( 'NONE',  ( -0.000000000000000000, -1.000000000000000000, -0.000000000000000000 ) ) ;
#76070 = ORIENTED_EDGE ( 'NONE', *, *, #19882, .F. ) ;
#76071 = CARTESIAN_POINT ( 'NONE',  ( -28.98875734969026396, -0.3587747205144262708, 0.1180228001186258285 ) ) ;
#76072 = CARTESIAN_POINT ( 'NONE',  ( -32.62287095715005592, -24.66019654487199020, 8.947790411086137041 ) ) ;
#76073 = CARTESIAN_POINT ( 'NONE',  ( 10.55456386191721663, 18.89434267519128596, -1.500000000000002220 ) ) ;
#76074 = CARTESIAN_POINT ( 'NONE',  ( -26.95875550904777285, -24.78998600965948640, 7.383661286321142825 ) ) ;
#76075 = CARTESIAN_POINT ( 'NONE',  ( 3.148799746435844593, 19.17640706095922098, -1.500000000000002220 ) ) ;
#76076 = CARTESIAN_POINT ( 'NONE',  ( -80.52287095715007581, -24.52323809116984421, 9.355190652339421931 ) ) ;
#76077 = LINE ( 'NONE', #21287, #36078 ) ;
#76078 = CARTESIAN_POINT ( 'NONE',  ( -2.602694502683683631, -19.63732897141692391, -1.500000000000002220 ) ) ;
#76079 = ORIENTED_EDGE ( 'NONE', *, *, #87701, .F. ) ;
#76080 = CARTESIAN_POINT ( 'NONE',  ( -20.32193514540556123, 0.06534614623005505218, 11.49999999999999645 ) ) ;
#76081 = CARTESIAN_POINT ( 'NONE',  ( -111.5562042904833788, -24.66019654487199730, 8.947790411086124607 ) ) ;
#76082 = CC_DESIGN_DATE_AND_TIME_ASSIGNMENT ( #60504, #85821, ( #19046 ) ) ;
#76083 = CARTESIAN_POINT ( 'NONE',  ( -60.52287095715007581, -25.00182538069855198, 7.747789668514453609 ) ) ;
#76084 = EDGE_LOOP ( 'NONE', ( #41902, #58158, #68053, #32494, #96817, #44686 ) ) ;
#76085 = B_SPLINE_SURFACE_WITH_KNOTS ( 'NONE', 3, 1, ( 
 ( #32148, #63628 ),
 ( #71727, #2720 ),
 ( #72729, #2221 ),
 ( #79820, #86936 ),
 ( #41789, #72226 ),
 ( #71226, #63123 ),
 ( #94049, #40766 ),
 ( #10317, #24535 ),
 ( #94546, #17427 ),
 ( #55504, #57514 ),
 ( #41272, #79322 ),
 ( #86441, #96059 ),
 ( #78807, #64134 ),
 ( #18922, #87440 ),
 ( #9816, #17933 ) ),
 .UNSPECIFIED., .F., .F., .F.,
 ( 4, 1, 1, 1, 1, 1, 1, 1, 1, 1, 1, 1, 4 ),
 ( 2, 2 ),
 ( 0.000000000000000000, 0.07594930733582139215, 0.1485490724434445076, 0.2189955450926088787, 0.2861189618869318663, 0.3518258552346302803, 0.4160741612610824314, 0.4782648099120661023, 0.5403245897751369764, 0.6604051854372985364, 0.7746061160792699907, 0.8871865992555415525, 1.000000000000000000 ),
 ( 0.000000000000000000, 1.000000000000000000 ),
 .UNSPECIFIED. ) ;
#76086 = CARTESIAN_POINT ( 'NONE',  ( -0.06447947376607357506, -22.21526254151202551, 0.5319095616429412310 ) ) ;
#76087 = CARTESIAN_POINT ( 'NONE',  ( -95.52287095715004739, -24.91570333825769978, 8.075032458260361423 ) ) ;
#76088 = CARTESIAN_POINT ( 'NONE',  ( -49.35191700208513765, -25.31601870270916521, 5.185240284718970472 ) ) ;
#76089 = DIRECTION ( 'NONE',  ( 1.000000000000000000, 0.000000000000000000, 0.000000000000000000 ) ) ;
#76090 = CARTESIAN_POINT ( 'NONE',  ( -51.06408614287066428, -25.14734643380794310, 6.959314159085416840 ) ) ;
#76091 = CARTESIAN_POINT ( 'NONE',  ( -11.36185547594953249, 16.55520930037988592, -1.500000000000002220 ) ) ;
#76092 = DIRECTION ( 'NONE',  ( 0.000000000000000000, 0.9999999999976377785, 2.173523156925979128E-06 ) ) ;
#76093 = ORIENTED_EDGE ( 'NONE', *, *, #41439, .T. ) ;
#76094 = CARTESIAN_POINT ( 'NONE',  ( -36.52287095715006870, -24.50216790748205398, 0.6166512839542417357 ) ) ;
#76095 = CARTESIAN_POINT ( 'NONE',  ( -9.150087108448493822, 20.98025145036519845, 11.49999999999999645 ) ) ;
#76096 = DIRECTION ( 'NONE',  ( 0.000000000000000000, 0.000000000000000000, 1.000000000000000000 ) ) ;
#76097 = CARTESIAN_POINT ( 'NONE',  ( 11.96754062809080743, 2.682774720514426559, -27.06850815473629979 ) ) ;
#76098 = CARTESIAN_POINT ( 'NONE',  ( -28.84663072490566194, -5.965225279485572685, 28.73989617533406715 ) ) ;
#76099 = CARTESIAN_POINT ( 'NONE',  ( -71.55620429048337883, -24.64898659630528854, 1.056161002820825701 ) ) ;
#76100 = VECTOR ( 'NONE', #78042, 1000.000000000000000 ) ;
#76101 = CARTESIAN_POINT ( 'NONE',  ( 6.499999999999992895, 1.999999999999998668, 2.499999999999999112 ) ) ;
#76102 = B_SPLINE_CURVE_WITH_KNOTS ( 'NONE', 3,
 ( #2226, #9309, #64139, #12189, #10322, #4099 ),
 .UNSPECIFIED., .F., .F.,
 ( 4, 2, 4 ),
 ( 1.570887131794333942E-05, 0.001396322306279758904, 0.002776935741241574537 ),
 .UNSPECIFIED. ) ;
#76103 = CARTESIAN_POINT ( 'NONE',  ( -111.5562042904834072, -23.47596703998600631, 11.44779298504227683 ) ) ;
#76104 = ORIENTED_EDGE ( 'NONE', *, *, #97236, .T. ) ;
#76105 = CARTESIAN_POINT ( 'NONE',  ( -9.871001836803966256, -17.81128643866572148, -1.500000000000002220 ) ) ;
#76106 = VERTEX_POINT ( 'NONE', #5428 ) ;
#76107 = EDGE_CURVE ( 'NONE', #71192, #1547, #70043, .T. ) ;
#76108 = CARTESIAN_POINT ( 'NONE',  ( 9.743704349311032686, 20.77413290702584092, 11.49999999999998934 ) ) ;
#76109 = FACE_OUTER_BOUND ( 'NONE', #34620, .T. ) ;
#76110 = ORIENTED_EDGE ( 'NONE', *, *, #21239, .T. ) ;
#76111 = AXIS2_PLACEMENT_3D ( 'NONE', #2683, #3682, #87403 ) ;
#76112 = CARTESIAN_POINT ( 'NONE',  ( 32.98733314340959311, -0.3587747205144265483, 2.074222136288530027 ) ) ;
#76113 = CARTESIAN_POINT ( 'NONE',  ( 32.15269211224249091, -4.540774720514427543, 3.401810532325273417 ) ) ;
#76114 = VECTOR ( 'NONE', #3532, 1000.000000000000000 ) ;
#76115 = CARTESIAN_POINT ( 'NONE',  ( 8.286623624103266097E-13, -23.05000000000000426, -1.500000000000002220 ) ) ;
#76117 = ORIENTED_EDGE ( 'NONE', *, *, #83908, .T. ) ;
#76116 = CARTESIAN_POINT ( 'NONE',  ( -18.64022381217131397, 10.26305532446727753, 11.49999999999999645 ) ) ;
#76118 = ADVANCED_FACE ( 'NONE', ( #87800 ), #95906, .F. ) ;
#76119 = VECTOR ( 'NONE', #79359, 1000.000000000000114 ) ;
#76120 = ORIENTED_EDGE ( 'NONE', *, *, #90586, .F. ) ;
#76121 = CARTESIAN_POINT ( 'NONE',  ( 21.18294168759468832, 6.642818831845659133, -1.500000000000002220 ) ) ;
#76122 = ADVANCED_FACE ( 'NONE', ( #10675 ), #18286, .T. ) ;
#76123 = CARTESIAN_POINT ( 'NONE',  ( 9.220172233967117492, 18.46515239161685784, -1.500000000000002220 ) ) ;
#76125 = ORIENTED_EDGE ( 'NONE', *, *, #15843, .F. ) ;
#76124 = VECTOR ( 'NONE', #64618, 1000.000000000000000 ) ;
#76126 = ORIENTED_EDGE ( 'NONE', *, *, #85670, .F. ) ;
#76127 = CARTESIAN_POINT ( 'NONE',  ( 9.843544857143434967, 5.965225279485572685, -27.49819965379373343 ) ) ;
#76128 = CARTESIAN_POINT ( 'NONE',  ( 3.552327343495968570, -5.876774720514426953, 21.81288606793570395 ) ) ;
#76129 = VERTEX_POINT ( 'NONE', #57374 ) ;
#76130 = VERTEX_POINT ( 'NONE', #88302 ) ;
#76131 = CARTESIAN_POINT ( 'NONE',  ( -127.2834285841887834, -25.28334328158019417, 4.245358510314064304 ) ) ;
#76132 = CARTESIAN_POINT ( 'NONE',  ( 14.83405752585509596, -4.881907540129173384, -27.54622755360215791 ) ) ;
#76133 = CARTESIAN_POINT ( 'NONE',  ( 19.16185898538474675, 8.078635803559651052, -1.500000000000002220 ) ) ;
#76134 = EDGE_CURVE ( 'NONE', #100298, #7254, #36364, .T. ) ;
#76135 = CARTESIAN_POINT ( 'NONE',  ( 19.23208339725441007, -10.27600428404867827, 11.49999999999999645 ) ) ;
#76136 = CARTESIAN_POINT ( 'NONE',  ( -51.93008262322722857, -25.24431853135508774, 6.222446891247057188 ) ) ;
#76137 = CARTESIAN_POINT ( 'NONE',  ( -78.50133211539314004, -24.51419770103157347, 9.386484678747175181 ) ) ;
#76138 = CARTESIAN_POINT ( 'NONE',  ( -3.368041826647835357, -22.21310627845187824, 11.49999999999998934 ) ) ;
#76139 = CARTESIAN_POINT ( 'NONE',  ( -51.26061221361337061, -25.31296648395201032, 4.199398687311516554 ) ) ;
#76140 = ORIENTED_EDGE ( 'NONE', *, *, #94626, .T. ) ;
#76141 = CARTESIAN_POINT ( 'NONE',  ( -50.52287095715007581, -25.00182538069144655, 7.747789668545104647 ) ) ;
#76142 = CARTESIAN_POINT ( 'NONE',  ( -69.52287095715010423, -23.95044443724993144, 10.65354141964649237 ) ) ;
#76143 = ORIENTED_EDGE ( 'NONE', *, *, #37676, .T. ) ;
#76144 = ORIENTED_EDGE ( 'NONE', *, *, #88693, .F. ) ;
#76145 = B_SPLINE_CURVE_WITH_KNOTS ( 'NONE', 3,
 ( #84898, #167, #93502, #23478, #32110, #46343, #45849, #77274, #54460, #77767, #85394, #94010, #15884, #46848, #78272 ),
 .UNSPECIFIED., .F., .F.,
 ( 4, 1, 1, 1, 1, 1, 1, 1, 1, 1, 1, 1, 4 ),
 ( 0.000000000000000000, 0.09781818961471311358, 0.1997260534018265310, 0.3052763574779380207, 0.4158114905382894744, 0.4744722311435595752, 0.5372738797760960860, 0.6036574205596552112, 0.6742988630901243230, 0.7498344853162268731, 0.8285984767571009657, 0.9123777781577814272, 1.000000000000000000 ),
 .UNSPECIFIED. ) ;
#76146 = CARTESIAN_POINT ( 'NONE',  ( -46.64649981546305924, -23.96169478059712432, 10.65365249895718414 ) ) ;
#76147 = ORIENTED_EDGE ( 'NONE', *, *, #98132, .T. ) ;
#76148 = CARTESIAN_POINT ( 'NONE',  ( -4.607724273132460802, 20.83226218841027944, -1.500000000000002220 ) ) ;
#76149 = ORIENTED_EDGE ( 'NONE', *, *, #65149, .F. ) ;
#76150 = CARTESIAN_POINT ( 'NONE',  ( -6.100820854657341918, -5.876774720514414518, 19.76359802465961124 ) ) ;
#76151 = CARTESIAN_POINT ( 'NONE',  ( -11.62490142266122639, -17.50836435561060256, 11.49999999999998934 ) ) ;
#76152 = CARTESIAN_POINT ( 'NONE',  ( -126.6228709571500559, -29.50248528299804818, 1.056150453629047137 ) ) ;
#76153 = CARTESIAN_POINT ( 'NONE',  ( -99.74425588205387783, -25.21639837048163457, 3.531259653993959802 ) ) ;
#76154 = CARTESIAN_POINT ( 'NONE',  ( -65.52287095715006160, -24.99156044556202616, 7.747789690856173195 ) ) ;
#76155 = CARTESIAN_POINT ( 'NONE',  ( -21.09739860443290382, 5.981408608369527258, -1.500000000000002220 ) ) ;
#76156 = FACE_OUTER_BOUND ( 'NONE', #52555, .T. ) ;
#76157 = ORIENTED_EDGE ( 'NONE', *, *, #51988, .F. ) ;
#76158 = CARTESIAN_POINT ( 'NONE',  ( -122.5222492067709368, -23.48786465467241769, 11.44779295918253581 ) ) ;
#76159 = EDGE_CURVE ( 'NONE', #93802, #21835, #35100, .T. ) ;
#76160 = EDGE_CURVE ( 'NONE', #49308, #70398, #77915, .T. ) ;
#76161 = CARTESIAN_POINT ( 'NONE',  ( -2.704906987277321040, 0.3587747205144061757, -28.92935364444904778 ) ) ;
#76162 = FACE_OUTER_BOUND ( 'NONE', #72443, .T. ) ;
#76163 = CARTESIAN_POINT ( 'NONE',  ( -10.27973282203687688, -22.47507199546397416, 10.47594215909544957 ) ) ;
#76164 = CARTESIAN_POINT ( 'NONE',  ( 21.14028111218437900, -2.610574537768086234, -1.500000000000002220 ) ) ;
#76165 = CARTESIAN_POINT ( 'NONE',  ( -98.58489322720483017, -24.66019654487200086, 8.947790411086119278 ) ) ;
#76166 = CARTESIAN_POINT ( 'NONE',  ( -51.92287095715006018, -23.47596703998600631, 11.44779298504227683 ) ) ;
#76167 = VECTOR ( 'NONE', #64693, 1000.000000000000000 ) ;
#76168 = ADVANCED_FACE ( 'NONE', ( #8424, #45997, #83544 ), #7417, .F. ) ;
#76169 = CARTESIAN_POINT ( 'NONE',  ( -90.62287095715011276, -24.62226745350440282, 0.9660975649728149595 ) ) ;
#76170 = CARTESIAN_POINT ( 'NONE',  ( -33.57507691967732200, -24.65952944569304606, 1.056160979905695907 ) ) ;
#76171 = CARTESIAN_POINT ( 'NONE',  ( 22.01961411883556252, 4.383451955130949429, -1.500000000000002220 ) ) ;
#76172 = ADVANCED_FACE ( 'NONE', ( #69828 ), #30759, .F. ) ;
#76173 = FACE_OUTER_BOUND ( 'NONE', #24724, .T. ) ;
#76174 = ORIENTED_EDGE ( 'NONE', *, *, #38024, .T. ) ;
#76175 = CARTESIAN_POINT ( 'NONE',  ( -81.52287095715001897, -24.66019654487199375, 8.947790411086126383 ) ) ;
#76176 = CARTESIAN_POINT ( 'NONE',  ( 14.10018531369908423, 13.67006465538575277, 11.49999999999999645 ) ) ;
#76177 = CARTESIAN_POINT ( 'NONE',  ( -68.62287095715005592, -23.47593901973091235, -1.443836447539006196 ) ) ;
#76178 = VECTOR ( 'NONE', #70144, 1000.000000000000000 ) ;
#76179 = DIRECTION ( 'NONE',  ( -3.773278334453079030E-23, 0.9999999999976377785, 2.173523156925979128E-06 ) ) ;
#76180 = VERTEX_POINT ( 'NONE', #46992 ) ;
#76181 = CARTESIAN_POINT ( 'NONE',  ( -121.5228709571500048, -23.47593901973090524, -1.443836447538996204 ) ) ;
#76182 = FACE_OUTER_BOUND ( 'NONE', #50237, .T. ) ;
#76183 = CARTESIAN_POINT ( 'NONE',  ( -100.1102081092206930, -25.25095791289925629, 5.264240324507090563 ) ) ;
#76184 = CARTESIAN_POINT ( 'NONE',  ( -25.85390067486408583, -24.79634013197061648, 6.939180248999893053 ) ) ;
#76185 = CARTESIAN_POINT ( 'NONE',  ( -19.50520112914412252, -2.896358124273927359, -1.500000000000002220 ) ) ;
#76186 = VECTOR ( 'NONE', #48626, 1000.000000000000114 ) ;
#76187 = EDGE_LOOP ( 'NONE', ( #10476, #56701, #56900, #64913 ) ) ;
#76188 = VECTOR ( 'NONE', #51684, 1000.000000000000000 ) ;
#76189 = CARTESIAN_POINT ( 'NONE',  ( -108.5895376238167245, -23.47596703998600631, 11.44779298504227683 ) ) ;
#76190 = LINE ( 'NONE', #68597, #17271 ) ;
#76191 = ADVANCED_FACE ( 'NONE', ( #91159 ), #69323, .F. ) ;
#76192 = CIRCLE ( 'NONE', #3374, 3.549999999999999378 ) ;
#76193 = PERSON_AND_ORGANIZATION_ROLE ( 'design_owner' ) ;
#76194 = VERTEX_POINT ( 'NONE', #53618 ) ;
#76195 = PLANE ( 'NONE',  #7825 ) ;
#76196 = VECTOR ( 'NONE', #18588, 1000.000000000000114 ) ;
#76197 = LINE ( 'NONE', #74219, #97687 ) ;
#76198 = CARTESIAN_POINT ( 'NONE',  ( -55.48854651988001763, -24.63355581998386157, 0.9682620441943822209 ) ) ;
#76199 = CARTESIAN_POINT ( 'NONE',  ( 32.58581522646812090, -4.151341569991283897, -4.025368652865530805 ) ) ;
#76200 = CARTESIAN_POINT ( 'NONE',  ( -6.752792875861700850, -6.376774720514411854, 19.46247113826586528 ) ) ;
#76201 = EDGE_CURVE ( 'NONE', #37481, #16105, #311, .T. ) ;
#76202 = CARTESIAN_POINT ( 'NONE',  ( -70.32437837831572836, -25.31201590703328463, 5.314180722553312641 ) ) ;
#76203 = CARTESIAN_POINT ( 'NONE',  ( -107.5162164984105004, -24.15543982623908192, -0.2315651400026443874 ) ) ;
#76204 = CARTESIAN_POINT ( 'NONE',  ( -18.20579941527595480, -8.200869797747142087, 11.49999999999998934 ) ) ;
#76205 = LINE ( 'NONE', #37655, #98517 ) ;
#76206 = CARTESIAN_POINT ( 'NONE',  ( -45.53828599902652741, -24.52399227489127043, 9.353111116836528183 ) ) ;
#76207 = ORIENTED_EDGE ( 'NONE', *, *, #62015, .T. ) ;
#76208 = EDGE_CURVE ( 'NONE', #54393, #53605, #10146, .T. ) ;
#76209 = EDGE_CURVE ( 'NONE', #77370, #85031, #39375, .T. ) ;
#76210 = CARTESIAN_POINT ( 'NONE',  ( -119.6264739001214821, -23.96119346886881019, -0.6495511937832016969 ) ) ;
#76211 = CARTESIAN_POINT ( 'NONE',  ( -80.58318537203670928, -24.83644354573579349, 8.397322867130101898 ) ) ;
#76212 = CARTESIAN_POINT ( 'NONE',  ( -127.2832169593331741, -25.28351172706441830, 5.756926109542241043 ) ) ;
#76213 = CARTESIAN_POINT ( 'NONE',  ( -39.58693056125937915, -24.34968618360933235, 0.1864209137778788383 ) ) ;
#76214 = CARTESIAN_POINT ( 'NONE',  ( -27.85310647731327904, -25.26026286786085961, 1.631227119663390068 ) ) ;
#76215 = CARTESIAN_POINT ( 'NONE',  ( -2.188401442307694289, -5.876774720514411854, 19.46153846153846700 ) ) ;
#76216 = DIRECTION ( 'NONE',  ( -1.000000000000000000, -0.000000000000000000, -0.000000000000000000 ) ) ;
#76217 = CARTESIAN_POINT ( 'NONE',  ( -47.62287095715004881, -29.50248528299804818, 1.056150453629033370 ) ) ;
#76218 = EDGE_LOOP ( 'NONE', ( #86542, #52974, #34732, #65292 ) ) ;
#76219 = CARTESIAN_POINT ( 'NONE',  ( -20.02346298389695534, -3.155783441878276196, -1.500000000000002220 ) ) ;
#76220 = EDGE_CURVE ( 'NONE', #76129, #88212, #77417, .T. ) ;
#76221 = CARTESIAN_POINT ( 'NONE',  ( -72.52287095715007581, -29.50248528299804818, 1.056150453629036701 ) ) ;
#76222 = CARTESIAN_POINT ( 'NONE',  ( 20.84816453548659609, 4.362175914522286035, -17.34246194398105345 ) ) ;
#76223 = CARTESIAN_POINT ( 'NONE',  ( -99.62287095715004170, -24.50216790748097750, 0.6166512839513834665 ) ) ;
#76224 = VERTEX_POINT ( 'NONE', #62227 ) ;
#76225 = CARTESIAN_POINT ( 'NONE',  ( -60.52287095715006160, -29.50248789122583659, 2.256150453626215580 ) ) ;
#76226 = CARTESIAN_POINT ( 'NONE',  ( -63.62287095715004881, -24.50216790748097395, 0.6166512839513691446 ) ) ;
#76227 = CARTESIAN_POINT ( 'NONE',  ( -15.79248070760165490, 12.47733877207048181, -1.500000000000002220 ) ) ;
#76228 = CARTESIAN_POINT ( 'NONE',  ( -18.71117167593497399, 9.704403692310313190, 11.49999999999999645 ) ) ;
#76229 = DIRECTION ( 'NONE',  ( -0.000000000000000000, -1.000000000000000000, -0.000000000000000000 ) ) ;
#76230 = CARTESIAN_POINT ( 'NONE',  ( 21.00647827173414939, 6.864759178008983831, -1.500000000000002220 ) ) ;
#76231 = AXIS2_PLACEMENT_3D ( 'NONE', #39208, #22965, #38711 ) ;
#76232 = ADVANCED_FACE ( 'NONE', ( #61233 ), #6431, .F. ) ;
#76233 = CARTESIAN_POINT ( 'NONE',  ( -19.38928925021375349, 6.733644070511561885, 11.49999999999998934 ) ) ;
#76234 = CARTESIAN_POINT ( 'NONE',  ( -66.62287095715005592, -24.66019654487199020, 8.947790411086131712 ) ) ;
#76235 = CARTESIAN_POINT ( 'NONE',  ( -53.62287095715006302, -24.34917612406836795, 0.1852690917426561001 ) ) ;
#76236 = ORIENTED_EDGE ( 'NONE', *, *, #24130, .T. ) ;
#76237 = DIRECTION ( 'NONE',  ( -0.000000000000000000, -1.000000000000000000, -0.000000000000000000 ) ) ;
#76238 = VERTEX_POINT ( 'NONE', #85541 ) ;
#76239 = ADVANCED_FACE ( 'NONE', ( #100244 ), #60731, .T. ) ;
#76240 = DIRECTION ( 'NONE',  ( -3.773278334453080206E-23, 0.9999999999976377785, 2.173523156925979975E-06 ) ) ;
#76241 = CARTESIAN_POINT ( 'NONE',  ( -29.62287095715004881, -23.39678932012542845, -1.443836140311830940 ) ) ;
#76242 = EDGE_LOOP ( 'NONE', ( #39687, #97062, #27737, #37978 ) ) ;
#76243 = VERTEX_POINT ( 'NONE', #68332 ) ;
#76244 = DIRECTION ( 'NONE',  ( 0.000000000000000000, 0.000000000000000000, 1.000000000000000000 ) ) ;
#76245 = CARTESIAN_POINT ( 'NONE',  ( -63.62287095715003460, -23.73907113216990794, -1.053371485793231699 ) ) ;
#76246 = CARTESIAN_POINT ( 'NONE',  ( -68.60259347313552780, -23.73791477778911840, 11.05961554403170943 ) ) ;
#76247 = CARTESIAN_POINT ( 'NONE',  ( -11.82494684808912844, 16.90534455221803967, -1.500000000000002220 ) ) ;
#76248 = EDGE_CURVE ( 'NONE', #16861, #62297, #99267, .T. ) ;
#76249 = CARTESIAN_POINT ( 'NONE',  ( 2.319523670979641849, -21.48760272935114557, 11.49999999999999645 ) ) ;
#76250 = ORIENTED_EDGE ( 'NONE', *, *, #17455, .T. ) ;
#76251 = DIRECTION ( 'NONE',  ( 1.000000000000000000, 3.773278334444167608E-23, 8.201307833595939069E-29 ) ) ;
#76252 = PLANE ( 'NONE',  #91791 ) ;
#76253 = CARTESIAN_POINT ( 'NONE',  ( -2.124831620219566730, 22.23837930986240607, 11.49999999999998934 ) ) ;
#76254 = ADVANCED_FACE ( 'NONE', ( #23129 ), #22629, .T. ) ;
#76255 = CARTESIAN_POINT ( 'NONE',  ( -79.76746806413464697, -25.12205757671817352, 6.852562942996416773 ) ) ;
#76256 = CARTESIAN_POINT ( 'NONE',  ( -84.56294249096249871, -23.48783264082476308, -1.443836473390094799 ) ) ;
#76257 = VERTEX_POINT ( 'NONE', #32759 ) ;
#76258 = DIRECTION ( 'NONE',  ( -3.773278334453079618E-23, 0.9999999999976377785, 2.173523156925979975E-06 ) ) ;
#76259 = CIRCLE ( 'NONE', #66605, 28.96799999999999287 ) ;
#76260 = CARTESIAN_POINT ( 'NONE',  ( -49.61441931870202637, -23.48786465467241058, 11.44779295918254824 ) ) ;
#76261 = VECTOR ( 'NONE', #87498, 1000.000000000000000 ) ;
#76262 = CARTESIAN_POINT ( 'NONE',  ( -7.158894406585330827, 19.61798520005962487, 11.49999999999998934 ) ) ;
#76263 = ORIENTED_EDGE ( 'NONE', *, *, #6221, .F. ) ;
#76265 = ORIENTED_EDGE ( 'NONE', *, *, #21034, .T. ) ;
#76264 = CARTESIAN_POINT ( 'NONE',  ( -86.59170088307759272, -24.15543982623907482, -0.2315651400026493556 ) ) ;
#76266 = ORIENTED_EDGE ( 'NONE', *, *, #2594, .T. ) ;
#76267 = CARTESIAN_POINT ( 'NONE',  ( -96.62287095715005592, -23.47593901973091235, -1.443836447539001089 ) ) ;
#76268 = CARTESIAN_POINT ( 'NONE',  ( -13.58512445790048417, 16.25115196636789250, -1.500000000000002220 ) ) ;
#76269 = VERTEX_POINT ( 'NONE', #18533 ) ;
#76270 = DIRECTION ( 'NONE',  ( -1.000000000000000000, -1.734723475976806848E-16, -0.000000000000000000 ) ) ;
#76271 = CARTESIAN_POINT ( 'NONE',  ( -99.69221343823950576, -25.12215628115585631, 6.884718414011108401 ) ) ;
#76272 = CARTESIAN_POINT ( 'NONE',  ( 21.79142754302170815, -0.6654467836950721527, 11.49999999999998934 ) ) ;
#76273 = CARTESIAN_POINT ( 'NONE',  ( -129.6228709571500701, -23.48786465467241769, 11.44779295918253581 ) ) ;
#76274 = CARTESIAN_POINT ( 'NONE',  ( -81.55620429048339304, -24.64898659630528854, 1.056161002820828143 ) ) ;
#76275 = CARTESIAN_POINT ( 'NONE',  ( -33.22287095715005734, -23.47593901973090169, -1.443836447538998202 ) ) ;
#76276 = CARTESIAN_POINT ( 'NONE',  ( -20.56741719582323213, 7.008553436993695485, -1.500000000000002220 ) ) ;
#76277 = CARTESIAN_POINT ( 'NONE',  ( -0.5830141525297981575, -6.376774720514410077, 19.15054976246387497 ) ) ;
#76279 = EDGE_LOOP ( 'NONE', ( #23710, #94622, #37056, #56578, #69184, #25425, #92810 ) ) ;
#76278 = CARTESIAN_POINT ( 'NONE',  ( -12.45998644600372884, -18.51849504856558681, 11.49999999999999645 ) ) ;
#76280 = PLANE ( 'NONE',  #82643 ) ;
#76281 = LINE ( 'NONE', #23479, #8669 ) ;
#76282 = DIRECTION ( 'NONE',  ( 0.000000000000000000, 1.000000000000000000, 0.000000000000000000 ) ) ;
#76283 = ORIENTED_EDGE ( 'NONE', *, *, #55442, .T. ) ;
#76284 = ORIENTED_EDGE ( 'NONE', *, *, #4204, .T. ) ;
#76285 = ADVANCED_FACE ( 'NONE', ( #79932 ), #33767, .F. ) ;
#76286 = ORIENTED_EDGE ( 'NONE', *, *, #94131, .F. ) ;
#76287 = CARTESIAN_POINT ( 'NONE',  ( -85.58953762381672448, -23.48786465467241413, 11.44779295918254114 ) ) ;
#76288 = CARTESIAN_POINT ( 'NONE',  ( -14.68016216564755894, -15.32010671487267572, -1.500000000000002220 ) ) ;
#76289 = CARTESIAN_POINT ( 'NONE',  ( -113.6228709571500417, -23.48783264082479150, -1.443836473390060160 ) ) ;
#76290 = CARTESIAN_POINT ( 'NONE',  ( -79.46053308078880661, -25.27791892412682984, 7.192626743707448256 ) ) ;
#76291 = DIRECTION ( 'NONE',  ( 0.000000000000000000, 1.000000000000000000, 0.000000000000000000 ) ) ;
#76292 = LINE ( 'NONE', #92521, #42695 ) ;
#76293 = CARTESIAN_POINT ( 'NONE',  ( -16.26263985875334228, -10.51264992557365829, -1.500000000000002220 ) ) ;
#76294 = CARTESIAN_POINT ( 'NONE',  ( -45.66178508354857968, -23.85016227208580375, -0.8807180028928391913 ) ) ;
#76295 = VERTEX_POINT ( 'NONE', #10421 ) ;
#76296 = CARTESIAN_POINT ( 'NONE',  ( -7.106217341473486826, 18.08270997100935418, 11.49999999999999645 ) ) ;
#76297 = CARTESIAN_POINT ( 'NONE',  ( -108.2228709571500644, -23.47596703998600631, 11.44779298504227860 ) ) ;
#76298 = VERTEX_POINT ( 'NONE', #17032 ) ;
#76299 = CARTESIAN_POINT ( 'NONE',  ( 3.559170184186323915, -6.376774720514402972, 18.55412939673608719 ) ) ;
#76300 = CARTESIAN_POINT ( 'NONE',  ( 3.252808283508203058, -6.376774720514402972, 18.30939203766361345 ) ) ;
#76301 = FACE_OUTER_BOUND ( 'NONE', #31251, .T. ) ;
#76302 = CARTESIAN_POINT ( 'NONE',  ( -130.5728709571500303, -23.47596703998600276, 11.44779298504227505 ) ) ;
#76303 = CARTESIAN_POINT ( 'NONE',  ( -16.92291128558595048, 9.936001969431544012, 11.49999999999998934 ) ) ;
#76304 = CARTESIAN_POINT ( 'NONE',  ( -66.52287095715006160, -23.48786465467241769, 11.44779295918254647 ) ) ;
#76305 = ORIENTED_EDGE ( 'NONE', *, *, #38409, .T. ) ;
#76306 = CARTESIAN_POINT ( 'NONE',  ( -8.857468890034409625, -19.66367526556523870, -1.500000000000002220 ) ) ;
#76307 = PLANE ( 'NONE',  #31758 ) ;
#76308 = CARTESIAN_POINT ( 'NONE',  ( -40.48996144562239863, -24.40034930558990922, 0.3402023900116037947 ) ) ;
#76309 = AXIS2_PLACEMENT_3D ( 'NONE', #11800, #26541, #73707 ) ;
#76310 = FACE_OUTER_BOUND ( 'NONE', #11824, .T. ) ;
#76311 = CARTESIAN_POINT ( 'NONE',  ( -5.126879528927636542, -22.49243673399587351, -1.500000000000002220 ) ) ;
#76312 = EDGE_CURVE ( 'NONE', #36801, #25844, #62970, .T. ) ;
#76313 = SECURITY_CLASSIFICATION_LEVEL ( 'unclassified' ) ;
#76314 = CARTESIAN_POINT ( 'NONE',  ( -93.54681100557382933, -24.51314013834316796, 0.6176544820404163971 ) ) ;
#76315 = CARTESIAN_POINT ( 'NONE',  ( -49.53589543791687788, -24.51314013834316086, 0.6176544820404130665 ) ) ;
#76316 = CARTESIAN_POINT ( 'NONE',  ( -19.13055903301823335, -6.388282315271819556, 11.49999999999999645 ) ) ;
#76317 = DIRECTION ( 'NONE',  ( 0.000000000000000000, 0.000000000000000000, -1.000000000000000000 ) ) ;
#76318 = CARTESIAN_POINT ( 'NONE',  ( 22.02124265030973760, 3.456774720514426136, 15.05402280011862004 ) ) ;
#76319 = CARTESIAN_POINT ( 'NONE',  ( -111.7736932848194726, -25.29824102673524067, 4.173604034445157929 ) ) ;
#76320 = CARTESIAN_POINT ( 'NONE',  ( -32.62287095715004881, -24.64898659630367206, 1.056161002820817485 ) ) ;
#76321 = CARTESIAN_POINT ( 'NONE',  ( -76.62287095715007013, -23.48783264082478084, -1.443836473390065489 ) ) ;
#76322 = CARTESIAN_POINT ( 'NONE',  ( 19.88832268942539017, -0.5522253751840191516, 11.49999999999998934 ) ) ;
#76324 = EDGE_CURVE ( 'NONE', #84765, #84975, #99243, .T. ) ;
#76323 = CARTESIAN_POINT ( 'NONE',  ( 8.971512145086499856, -1.028487854913500810, 3.750000000000000000 ) ) ;
#76325 = CARTESIAN_POINT ( 'NONE',  ( -5.448126336921106372, -18.99418723138115084, -1.500000000000002220 ) ) ;
#76326 = EDGE_CURVE ( 'NONE', #69692, #67443, #48397, .T. ) ;
#76327 = CARTESIAN_POINT ( 'NONE',  ( -42.53975314095062288, -24.34968618360933590, 0.1864209137778841952 ) ) ;
#76328 = EDGE_CURVE ( 'NONE', #20641, #23622, #57120, .T. ) ;
#76331 = EDGE_CURVE ( 'NONE', #43735, #11601, #99038, .T. ) ;
#76330 = UNCERTAINTY_MEASURE_WITH_UNIT (LENGTH_MEASURE( 1.000000000000000082E-05 ), #59020, 'distance_accuracy_value', 'NONE');
#76329 = AXIS2_PLACEMENT_3D ( 'NONE', #34902, #11551, #79571 ) ;
#76332 = CARTESIAN_POINT ( 'NONE',  ( -40.07089665442598658, -25.10925601320060352, 2.873458142001279914 ) ) ;
#76333 = CARTESIAN_POINT ( 'NONE',  ( -5.576923076923074873, -6.376774720514427841, 21.75000000000000711 ) ) ;
#76334 = CARTESIAN_POINT ( 'NONE',  ( 2.909938941155331360, -20.50406750007545398, 11.49999999999999645 ) ) ;
#76335 = CARTESIAN_POINT ( 'NONE',  ( -58.52287095715004739, -23.47593901973090169, -1.443836447538997092 ) ) ;
#76336 = CARTESIAN_POINT ( 'NONE',  ( -7.641025641025638748, -6.376774720514427841, 21.75000000000001066 ) ) ;
#76337 = CARTESIAN_POINT ( 'NONE',  ( 17.32531159343115945, 14.66459048539768162, 11.49999999999999645 ) ) ;
#76338 = ORIENTED_EDGE ( 'NONE', *, *, #94435, .T. ) ;
#76339 = CARTESIAN_POINT ( 'NONE',  ( -60.62287095715004881, -25.00158670708908915, 2.256160236439166855 ) ) ;
#76340 = CARTESIAN_POINT ( 'NONE',  ( -70.19984806589197035, -25.12381722767544190, 7.096917652772970264 ) ) ;
#76341 = CARTESIAN_POINT ( 'NONE',  ( -20.08517628505838815, -1.856936949192496300, -1.500000000000002220 ) ) ;
#76342 = EDGE_CURVE ( 'NONE', #11758, #47988, #63742, .T. ) ;
#76343 = CARTESIAN_POINT ( 'NONE',  ( -63.58766835849188936, -24.34968618360933590, 0.1864209137778804204 ) ) ;
#76344 = PLANE ( 'NONE',  #28567 ) ;
#76345 = ORIENTED_EDGE ( 'NONE', *, *, #76602, .T. ) ;
#76346 = VERTEX_POINT ( 'NONE', #86046 ) ;
#76347 = EDGE_CURVE ( 'NONE', #2790, #64651, #88059, .T. ) ;
#76348 = LINE ( 'NONE', #68756, #53389 ) ;
#76349 = CARTESIAN_POINT ( 'NONE',  ( 22.81499323874321661, -2.031749852351878882, 11.49999999999998934 ) ) ;
#76350 = CARTESIAN_POINT ( 'NONE',  ( -50.49777224651334961, -25.27420563618652238, 3.296419135251263732 ) ) ;
#76351 = CARTESIAN_POINT ( 'NONE',  ( 5.568959250215116619, -20.88136358707659923, -1.500000000000002220 ) ) ;
#76352 = FACE_OUTER_BOUND ( 'NONE', #9354, .T. ) ;
#76353 = DIRECTION ( 'NONE',  ( 0.000000000000000000, -1.000000000000000000, 0.000000000000000000 ) ) ;
#76354 = CARTESIAN_POINT ( 'NONE',  ( -19.40224465947428456, -7.824916089261592766, 11.49999999999999645 ) ) ;
#76355 = EDGE_LOOP ( 'NONE', ( #78834, #38742, #7865, #43264 ) ) ;
#76356 = CARTESIAN_POINT ( 'NONE',  ( -70.27422298781921484, -25.31612420447723011, 4.851635139248643647 ) ) ;
#76357 = CARTESIAN_POINT ( 'NONE',  ( 7.855769811932122870, -20.56199346058834720, 11.49999999999998934 ) ) ;
#76358 = ADVANCED_FACE ( 'NONE', ( #80439 ), #47494, .T. ) ;
#76359 = PLANE ( 'NONE',  #94911 ) ;
#76360 = CARTESIAN_POINT ( 'NONE',  ( -27.75582626765746497, -24.79700316727673126, 7.602201205707691756 ) ) ;
#76361 = VERTEX_POINT ( 'NONE', #70831 ) ;
#76362 = CARTESIAN_POINT ( 'NONE',  ( 4.531089049250198286, -6.376774720514404748, 18.46391971337801508 ) ) ;
#76363 = CARTESIAN_POINT ( 'NONE',  ( -90.58449365438282541, -24.83644354573578994, 8.397322867130100121 ) ) ;
#76364 = ORIENTED_EDGE ( 'NONE', *, *, #98386, .T. ) ;
#76365 = CARTESIAN_POINT ( 'NONE',  ( -72.63059420557763701, -24.35071581493543036, 9.817618358456032368 ) ) ;
#76366 = EDGE_LOOP ( 'NONE', ( #21203, #79167, #44473, #44430 ) ) ;
#76367 = ORIENTED_EDGE ( 'NONE', *, *, #73163, .T. ) ;
#76368 = CARTESIAN_POINT ( 'NONE',  ( -59.62287095715004881, -23.47593901973091235, -1.443836447539007972 ) ) ;
#76369 = CARTESIAN_POINT ( 'NONE',  ( -95.62287095715004170, -24.63345952396256777, 9.038047939301502964 ) ) ;
#76370 = CARTESIAN_POINT ( 'NONE',  ( -57.54252097118408216, -24.34968618360933590, 0.1864209137778796155 ) ) ;
#76371 = CARTESIAN_POINT ( 'NONE',  ( 8.813945691637787405, 18.49579627399651471, -1.500000000000002220 ) ) ;
#76372 = ADVANCED_FACE ( 'NONE', ( #1320 ), #24637, .T. ) ;
#76373 = ORIENTED_EDGE ( 'NONE', *, *, #48536, .T. ) ;
#76374 = CYLINDRICAL_SURFACE ( 'NONE', #34750, 130.2784398600581710 ) ;
#76375 = B_SPLINE_CURVE_WITH_KNOTS ( 'NONE', 3,
 ( #14067, #6472, #68374, #29802 ),
 .UNSPECIFIED., .F., .F.,
 ( 4, 4 ),
 ( 0.000000000000000000, 0.0001000000000000167422 ),
 .UNSPECIFIED. ) ;
#76376 = CARTESIAN_POINT ( 'NONE',  ( -60.62287095715004881, -23.47593901973091235, -1.443836447539007972 ) ) ;
#76377 = DIRECTION ( 'NONE',  ( 1.000000000000000000, 3.491481338843133355E-15, 2.352173255807796056E-16 ) ) ;
#76378 = CARTESIAN_POINT ( 'NONE',  ( 19.02167141253037030, -11.55642654327076535, 11.49999999999998934 ) ) ;
#76379 = ADVANCED_FACE ( 'NONE', ( #9416 ), #47894, .F. ) ;
#76380 = CARTESIAN_POINT ( 'NONE',  ( -4.165021623707020559, -6.376774720514417183, 20.26087634804756377 ) ) ;
#76381 = CARTESIAN_POINT ( 'NONE',  ( -88.62287095715004170, -23.96177878511308634, 10.65340807706329507 ) ) ;
#76382 = ORIENTED_EDGE ( 'NONE', *, *, #38645, .F. ) ;
#76383 = DIRECTION ( 'NONE',  ( 1.000000000000000000, 0.000000000000000000, 0.000000000000000000 ) ) ;
#76384 = CARTESIAN_POINT ( 'NONE',  ( -28.66728577581702808, -24.63646007072033228, 7.986660916366364660 ) ) ;
#76385 = CARTESIAN_POINT ( 'NONE',  ( 20.75994597877129877, -1.272245555857973054, -1.500000000000002220 ) ) ;
#76386 = AXIS2_PLACEMENT_3D ( 'NONE', #98666, #91061, #52512 ) ;
#76387 = ORIENTED_EDGE ( 'NONE', *, *, #34067, .F. ) ;
#76389 = EDGE_LOOP ( 'NONE', ( #95816, #59353, #60953, #93235, #89236, #26115, #87213, #23863, #26839, #21321, #81982 ) ) ;
#76388 = CARTESIAN_POINT ( 'NONE',  ( 4.214857194124448370, -6.376774720514402972, 18.65898740197609840 ) ) ;
#76390 = CARTESIAN_POINT ( 'NONE',  ( -27.96875734969026084, -3.316774720514426456, 0.7300228001186309656 ) ) ;
#76391 = ORIENTED_EDGE ( 'NONE', *, *, #18968, .F. ) ;
#76392 = ORIENTED_EDGE ( 'NONE', *, *, #93816, .T. ) ;
#76393 = CARTESIAN_POINT ( 'NONE',  ( 7.293136219020367683, 10.80195425911416329, -0.9450485415980990345 ) ) ;
#76394 = CARTESIAN_POINT ( 'NONE',  ( -4.700032041049139409, -6.144890974841530351, 8.999999999999998224 ) ) ;
#76395 = CARTESIAN_POINT ( 'NONE',  ( -118.1692044365139367, -25.21250203164488468, 3.500954016957965820 ) ) ;
#76396 = CARTESIAN_POINT ( 'NONE',  ( -100.7317701684513764, -25.25419550244751221, 7.544845661441120122 ) ) ;
#76397 = CARTESIAN_POINT ( 'NONE',  ( -91.62287095715004170, -23.47593901973091235, -1.443836447539002865 ) ) ;
#76398 = FACE_OUTER_BOUND ( 'NONE', #67820, .T. ) ;
#76400 = ORIENTED_EDGE ( 'NONE', *, *, #4819, .T. ) ;
#76399 = CARTESIAN_POINT ( 'NONE',  ( 21.58644828898399481, -4.983269013152989757, 11.49999999999999645 ) ) ;
#76401 = CARTESIAN_POINT ( 'NONE',  ( 11.16000000000000014, -10.15233964170348457, 0.003711184059992174607 ) ) ;
#76402 = CARTESIAN_POINT ( 'NONE',  ( -11.22117850230010738, 19.66027149220947123, -1.500000000000002220 ) ) ;
#76404 = ORIENTED_EDGE ( 'NONE', *, *, #63430, .F. ) ;
#76403 = CARTESIAN_POINT ( 'NONE',  ( -36.62287095715005592, -24.64898659630367916, 1.056161002820819261 ) ) ;
#76405 = AXIS2_PLACEMENT_3D ( 'NONE', #77801, #39258, #70218 ) ;
#76406 = VERTEX_POINT ( 'NONE', #19031 ) ;
#76407 = CC_DESIGN_APPROVAL ( #42673, ( #57026 ) ) ;
#76408 = MANIFOLD_SOLID_BREP ( 'CirPattern1', #1506 ) ;
#76409 = DIRECTION ( 'NONE',  ( -0.000000000000000000, 1.000000000000000000, 0.000000000000000000 ) ) ;
#76410 = B_SPLINE_CURVE_WITH_KNOTS ( 'NONE', 3,
 ( #76273, #51464, #82399, #66212 ),
 .UNSPECIFIED., .F., .F.,
 ( 4, 4 ),
 ( 0.000000000000000000, 0.0001000000000000444977 ),
 .UNSPECIFIED. ) ;
#76411 = CARTESIAN_POINT ( 'NONE',  ( -18.22032804147677254, 8.545885342870345625, 11.49999999999998934 ) ) ;
#76412 = LINE ( 'NONE', #8414, #11693 ) ;
#76413 = ORIENTED_EDGE ( 'NONE', *, *, #93165, .T. ) ;
#76414 = PLANE ( 'NONE',  #95693 ) ;
#76415 = CARTESIAN_POINT ( 'NONE',  ( -18.97848940637192428, 11.77069306843248064, -1.500000000000002220 ) ) ;
#76416 = ORIENTED_EDGE ( 'NONE', *, *, #36138, .T. ) ;
#76417 = ORIENTED_EDGE ( 'NONE', *, *, #680, .F. ) ;
#76418 = FACE_OUTER_BOUND ( 'NONE', #46959, .T. ) ;
#76419 = CARTESIAN_POINT ( 'NONE',  ( -119.5895376238167387, -23.48786465467241769, 11.44779295918253759 ) ) ;
#76420 = CARTESIAN_POINT ( 'NONE',  ( -85.58953762381672448, -23.47596703998600631, 11.44779298504227683 ) ) ;
#76421 = CARTESIAN_POINT ( 'NONE',  ( 32.54628039735602130, 5.044004387208919304, -11.78547710168594165 ) ) ;
#76422 = CARTESIAN_POINT ( 'NONE',  ( 13.36367879947601445, -6.376774720514426953, 20.00000000000000355 ) ) ;
#76423 = CARTESIAN_POINT ( 'NONE',  ( 12.76379665850700640, 14.79237594083867080, -1.500000000000002220 ) ) ;
#76424 = DIRECTION ( 'NONE',  ( 0.000000000000000000, 0.000000000000000000, -1.000000000000000000 ) ) ;
#76425 = CARTESIAN_POINT ( 'NONE',  ( -11.48222599368078889, -18.13851731312990267, 11.49999999999998934 ) ) ;
#76426 = CARTESIAN_POINT ( 'NONE',  ( -3.826923076923078426, -5.876774720514409189, 19.19230769230769695 ) ) ;
#76427 = CARTESIAN_POINT ( 'NONE',  ( -46.52287095715006160, -23.47596703998600631, 11.44779298504229104 ) ) ;
#76429 = B_SPLINE_CURVE_WITH_KNOTS ( 'NONE', 3,
 ( #10404, #10913, #72316, #64219, #64731, #94639, #95145, #42384, #24616, #17011, #25632, #49489, #40853, #95647 ),
 .UNSPECIFIED., .F., .F.,
 ( 4, 2, 2, 2, 2, 2, 4 ),
 ( 1.411962612463446054E-17, 0.0001805495034875036512, 0.0003610990069749931536, 0.0007221980139500113523, 0.001083297020925029714, 0.001263846524412529570, 0.001444396027900029860 ),
 .UNSPECIFIED. ) ;
#76428 = CARTESIAN_POINT ( 'NONE',  ( -118.5228709571500758, -23.47593901973090524, -1.443836447538996204 ) ) ;
#76430 = CARTESIAN_POINT ( 'NONE',  ( 7.980177114813061579, 21.45908683785374649, -1.500000000000002220 ) ) ;
#76431 = VECTOR ( 'NONE', #7394, 1000.000000000000000 ) ;
#76432 = DATE_AND_TIME ( #15040, #22926 ) ;
#76433 = CARTESIAN_POINT ( 'NONE',  ( -120.5895376238167245, -25.00158670708909980, 2.256160236439166411 ) ) ;
#76434 = CARTESIAN_POINT ( 'NONE',  ( 3.675000000000004707, 1.999999999999998224, 18.24068255301867936 ) ) ;
#76435 = CARTESIAN_POINT ( 'NONE',  ( -12.66726347749767179, -15.43046242340049545, 11.49999999999999645 ) ) ;
#76436 = CARTESIAN_POINT ( 'NONE',  ( -120.5228709571500616, -29.50248528299804818, 1.056150453629045360 ) ) ;
#76437 = EDGE_CURVE ( 'NONE', #50685, #45688, #58604, .T. ) ;
#76438 = EDGE_CURVE ( 'NONE', #96494, #87248, #66238, .T. ) ;
#76439 = CARTESIAN_POINT ( 'NONE',  ( -63.52287095715003318, -23.48783264082477018, -1.443836473390091690 ) ) ;
#76440 = PLANE ( 'NONE',  #35915 ) ;
#76441 = EDGE_LOOP ( 'NONE', ( #4884, #11477, #97385, #81238 ) ) ;
#76442 = DIRECTION ( 'NONE',  ( -1.000000000000000000, -0.000000000000000000, -0.000000000000000000 ) ) ;
#76443 = CARTESIAN_POINT ( 'NONE',  ( -65.52287095715009002, -24.92604778743017491, 8.074972756849353672 ) ) ;
#76444 = EDGE_CURVE ( 'NONE', #88649, #33103, #12414, .T. ) ;
#76445 = CARTESIAN_POINT ( 'NONE',  ( -20.56741719582323213, 7.008553436993695485, -1.500000000000002220 ) ) ;
#76446 = CARTESIAN_POINT ( 'NONE',  ( -78.52287095715006160, -23.48786465467241769, 11.44779295918254469 ) ) ;
#76447 = CARTESIAN_POINT ( 'NONE',  ( -11.77723790057865116, -15.68276428244051779, -1.500000000000002220 ) ) ;
#76448 = ADVANCED_FACE ( 'NONE', ( #67228 ), #16749, .T. ) ;
#76449 = CARTESIAN_POINT ( 'NONE',  ( -99.89883556272337728, -25.14992886684538931, 7.003669732127485226 ) ) ;
#76450 = ADVANCED_FACE ( 'NONE', ( #67727 ), #7800, .F. ) ;
#76451 = COORDINATED_UNIVERSAL_TIME_OFFSET ( 0, 0, .AHEAD. ) ;
#76452 = LINE ( 'NONE', #6957, #4653 ) ;
#76453 = CARTESIAN_POINT ( 'NONE',  ( 3.050049012211247579, -6.376774720514426065, 21.53019692557248632 ) ) ;
#76454 = CARTESIAN_POINT ( 'NONE',  ( -7.444040098415714013, -19.11467064512029879, 11.49999999999999645 ) ) ;
#76455 = DIRECTION ( 'NONE',  ( -0.09824042138329623641, -2.980407940728110405E-17, 0.9951627101165078093 ) ) ;
#76456 = AXIS2_PLACEMENT_3D ( 'NONE', #12805, #29531, #99530 ) ;
#76457 = FACE_OUTER_BOUND ( 'NONE', #1132, .T. ) ;
#76458 = VERTEX_POINT ( 'NONE', #91039 ) ;
#76459 = CARTESIAN_POINT ( 'NONE',  ( -30.48631411044201656, -23.47596703823905528, 11.44698924286007369 ) ) ;
#76460 = CARTESIAN_POINT ( 'NONE',  ( 3.675000000000004707, 1.999999999999998224, 24.00000000000000000 ) ) ;
#76461 = LINE ( 'NONE', #67382, #84097 ) ;
#76462 = FACE_OUTER_BOUND ( 'NONE', #11714, .T. ) ;
#76463 = PLANE ( 'NONE',  #28992 ) ;
#76464 = APPROVAL_PERSON_ORGANIZATION ( #41926, #9079, #40906 ) ;
#76465 = CARTESIAN_POINT ( 'NONE',  ( 32.33465265239741626, 4.457608646344818126, 0.9133233228923198777 ) ) ;
#76466 = B_SPLINE_CURVE_WITH_KNOTS ( 'NONE', 3,
 ( #23894, #79686, #86799, #10183, #25404, #79184 ),
 .UNSPECIFIED., .F., .F.,
 ( 4, 2, 4 ),
 ( 6.391158118959990520E-06, 0.001387004593080781592, 0.002767618028042603297 ),
 .UNSPECIFIED. ) ;
#76467 = AXIS2_PLACEMENT_3D ( 'NONE', #7954, #76455, #61764 ) ;
#76468 = EDGE_CURVE ( 'NONE', #76683, #98076, #20318, .T. ) ;
#76469 = CARTESIAN_POINT ( 'NONE',  ( 10.36671515591691950, -20.60271000134967068, 11.49999999999999645 ) ) ;
#76470 = CARTESIAN_POINT ( 'NONE',  ( 18.64237364862239943, 13.12531859369229359, -1.500000000000002220 ) ) ;
#76471 = CARTESIAN_POINT ( 'NONE',  ( 3.296548071537245495, -6.376774720514426065, 21.29143507544719682 ) ) ;
#76472 = CARTESIAN_POINT ( 'NONE',  ( -105.6228709571500843, -24.51163499207180507, 0.6490370598555564863 ) ) ;
#76473 = CARTESIAN_POINT ( 'NONE',  ( -104.5562042904833930, -24.66019654487199730, 8.947790411086124607 ) ) ;
#76474 = LOCAL_TIME ( 0, 54, 15.00000000000000000, #42297 ) ;
#76475 = CARTESIAN_POINT ( 'NONE',  ( -110.2929128916653525, -25.15277794460069316, 6.986250878905948980 ) ) ;
#76476 = CARTESIAN_POINT ( 'NONE',  ( -99.50663065733192525, -25.31582213395984837, 4.996268174089572689 ) ) ;
#76477 = CARTESIAN_POINT ( 'NONE',  ( -3.478157889954244464, -21.63767827151469447, 11.49999999999998934 ) ) ;
#76478 = CARTESIAN_POINT ( 'NONE',  ( -5.293508136514246232, -5.876774720514408301, 19.18727597066021318 ) ) ;
#76479 = CARTESIAN_POINT ( 'NONE',  ( -87.51421109775209572, -23.96169478059713498, 10.65365249895718058 ) ) ;
#76480 = CARTESIAN_POINT ( 'NONE',  ( 11.22434917415779054, 4.132774715458839232, -26.87660878605755599 ) ) ;
#76481 = CARTESIAN_POINT ( 'NONE',  ( -78.55878933397490016, -23.73766607897670511, -1.055555164236459342 ) ) ;
#76482 = CARTESIAN_POINT ( 'NONE',  ( -117.6228709571500559, -23.72747288104441665, -1.053458166803660667 ) ) ;
#76483 = ORIENTED_EDGE ( 'NONE', *, *, #94242, .T. ) ;
#76484 = CARTESIAN_POINT ( 'NONE',  ( 20.35601985306173134, -1.938729116259007679, 11.49999999999998934 ) ) ;
#76485 = EDGE_LOOP ( 'NONE', ( #15071, #4183, #40238, #42458 ) ) ;
#76486 = ORIENTED_EDGE ( 'NONE', *, *, #14227, .T. ) ;
#76487 = ORIENTED_EDGE ( 'NONE', *, *, #91288, .F. ) ;
#76488 = ORIENTED_EDGE ( 'NONE', *, *, #20837, .T. ) ;
#76489 = CARTESIAN_POINT ( 'NONE',  ( -21.01138170180016118, -9.542296329091309204, 11.49999999999998934 ) ) ;
#76490 = CARTESIAN_POINT ( 'NONE',  ( -41.48151182693364802, -25.18341647909762671, 3.283321612209681550 ) ) ;
#76491 = CARTESIAN_POINT ( 'NONE',  ( 12.36038202409810438, -16.04522380935875248, -1.500000000000002220 ) ) ;
#76492 = ORIENTED_EDGE ( 'NONE', *, *, #53376, .T. ) ;
#76493 = CARTESIAN_POINT ( 'NONE',  ( -29.26901259668666100, -25.11027012358568911, 6.759032221908313431 ) ) ;
#76494 = CARTESIAN_POINT ( 'NONE',  ( -46.62287095715004881, -24.64898659630528499, 1.056161002820821038 ) ) ;
#76495 = ADVANCED_FACE ( 'NONE', ( #13907 ), #44885, .T. ) ;
#76496 = CARTESIAN_POINT ( 'NONE',  ( -93.62287095715007013, -23.47596703998600631, 11.44779298504227860 ) ) ;
#76497 = CARTESIAN_POINT ( 'NONE',  ( -70.54637579065081354, -24.40034930558990922, 0.3402023900116040167 ) ) ;
#76499 = VERTEX_POINT ( 'NONE', #6307 ) ;
#76498 = CARTESIAN_POINT ( 'NONE',  ( 0.5228555243449846124, 21.43159495547403282, 11.49999999999999645 ) ) ;
#76500 = CARTESIAN_POINT ( 'NONE',  ( -48.52287095715006160, -29.50248528299804818, 1.056150453629033370 ) ) ;
#76501 = CARTESIAN_POINT ( 'NONE',  ( -61.60404647597454186, -23.73791477778911840, 11.05961554403170943 ) ) ;
#76502 = ORIENTED_EDGE ( 'NONE', *, *, #24224, .T. ) ;
#76503 = CARTESIAN_POINT ( 'NONE',  ( -18.06733440434376092, 10.15830956056102963, -1.500000000000002220 ) ) ;
#76504 = EDGE_CURVE ( 'NONE', #97458, #89315, #37263, .T. ) ;
#76505 = VERTEX_POINT ( 'NONE', #22507 ) ;
#76507 = ORIENTED_EDGE ( 'NONE', *, *, #82199, .F. ) ;
#76506 = CARTESIAN_POINT ( 'NONE',  ( 0.000000000000000000, -5.876774720514426953, 0.000000000000000000 ) ) ;
#76508 = AXIS2_PLACEMENT_3D ( 'NONE', #7534, #86158, #47112 ) ;
#76509 = B_SPLINE_SURFACE_WITH_KNOTS ( 'NONE', 3, 3, ( 
 ( #51017, #58138, #33275, #42908 ),
 ( #95184, #88080, #11444, #4344 ),
 ( #73354, #34788, #35294, #41402 ),
 ( #57143, #72857, #49526, #27677 ),
 ( #81953, #12437, #90561, #22028 ),
 ( #5325, #36288, #21041, #66758 ),
 ( #60634, #97676, #13429, #68730 ) ),
 .UNSPECIFIED., .F., .F., .F.,
 ( 4, 3, 4 ),
 ( 4, 4 ),
 ( 0.7945040050992250302, 0.8970133687736510097, 0.9995227324480769893 ),
 ( 0.9797429635068189979, 0.9812080024286750080 ),
 .UNSPECIFIED. ) ;
#76510 = CARTESIAN_POINT ( 'NONE',  ( 15.29947330337540556, -3.405372460181236960, -27.16854002387011491 ) ) ;
#76511 = EDGE_LOOP ( 'NONE', ( #91744, #35945, #17398, #25386 ) ) ;
#76512 = CARTESIAN_POINT ( 'NONE',  ( -55.52287095715006160, -24.91570333825770689, 8.075032458260354318 ) ) ;
#76513 = CARTESIAN_POINT ( 'NONE',  ( -65.50513712851758896, -24.15503026093916361, -0.2815557561904382111 ) ) ;
#76514 = CARTESIAN_POINT ( 'NONE',  ( 0.3405503412851532130, 21.98688381012616233, 11.49999999999999645 ) ) ;
#76515 = FACE_OUTER_BOUND ( 'NONE', #31591, .T. ) ;
#76516 = CARTESIAN_POINT ( 'NONE',  ( 21.16815136333514502, -7.790938087775149512, 11.49999999999998934 ) ) ;
#76517 = CARTESIAN_POINT ( 'NONE',  ( -4.092705237139750984, -20.55955383578756113, 11.49999999999998934 ) ) ;
#76518 = CARTESIAN_POINT ( 'NONE',  ( -109.1607220907064004, -25.31604877966584155, 4.925676078390490709 ) ) ;
#76519 = CARTESIAN_POINT ( 'NONE',  ( 5.671135738765417322, -6.376774720514422512, 20.99074880795119924 ) ) ;
#76520 = ORIENTED_EDGE ( 'NONE', *, *, #17155, .T. ) ;
#76521 = AXIS2_PLACEMENT_3D ( 'NONE', #2464, #64889, #19168 ) ;
#76522 = ORIENTED_EDGE ( 'NONE', *, *, #59809, .F. ) ;
#76523 = EDGE_LOOP ( 'NONE', ( #61832, #38440, #31220, #94706 ) ) ;
#76524 = TOROIDAL_SURFACE ( 'NONE', #29520, 3.060000000000000053, 2.040000000000000036 ) ;
#76525 = DIRECTION ( 'NONE',  ( -0.8369330630277744820, 1.189580657286399882E-06, -0.5473052603525132564 ) ) ;
#76526 = CARTESIAN_POINT ( 'NONE',  ( 16.66814584454133907, -13.58961022886752978, -1.500000000000002220 ) ) ;
#76527 = CARTESIAN_POINT ( 'NONE',  ( -90.62287095715004170, -23.84081130438200091, 10.88220057463249191 ) ) ;
#76528 = VERTEX_POINT ( 'NONE', #14902 ) ;
#76529 = CARTESIAN_POINT ( 'NONE',  ( 13.68530018921192060, -16.06810839794082924, -1.500000000000002220 ) ) ;
#76530 = CARTESIAN_POINT ( 'NONE',  ( -127.6228709571500559, -29.50250243563736774, 8.947779886222132717 ) ) ;
#76531 = CARTESIAN_POINT ( 'NONE',  ( -64.60341764832335798, -23.73766607897670156, -1.055555164236459564 ) ) ;
#76532 = CARTESIAN_POINT ( 'NONE',  ( -83.60405270194971195, -23.48786465467241413, 11.44779295918254469 ) ) ;
#76533 = DIRECTION ( 'NONE',  ( 0.000000000000000000, 0.000000000000000000, 1.000000000000000000 ) ) ;
#76534 = CARTESIAN_POINT ( 'NONE',  ( -99.66129388137581202, -25.14737294716416471, 3.044676272356992008 ) ) ;
#76535 = CARTESIAN_POINT ( 'NONE',  ( -7.477829544921322125, 20.88912457518834742, -1.500000000000002220 ) ) ;
#76536 = CARTESIAN_POINT ( 'NONE',  ( -8.160000000000001918, -9.799686150098729343, 1.264356398917767743 ) ) ;
#76537 = ORIENTED_EDGE ( 'NONE', *, *, #94440, .T. ) ;
#76538 = CARTESIAN_POINT ( 'NONE',  ( -51.77186309286971522, -25.31633219839644156, 5.562993592441398683 ) ) ;
#76539 = CARTESIAN_POINT ( 'NONE',  ( -73.52287095715007581, -24.66019654487199730, 8.947790411086121054 ) ) ;
#76540 = CARTESIAN_POINT ( 'NONE',  ( -43.62287095715004881, -24.65952944569304606, 1.056160979905692576 ) ) ;
#76541 = DIRECTION ( 'NONE',  ( 0.000000000000000000, -0.9999999999976377785, -2.173523156925979975E-06 ) ) ;
#76542 = VECTOR ( 'NONE', #14529, 1000.000000000000114 ) ;
#76543 = CARTESIAN_POINT ( 'NONE',  ( 5.650214204171827070, -18.61605495904187535, 11.49999999999998934 ) ) ;
#76544 = ORGANIZATION ( 'NAUO-ORG2', 'UNSPECIFIED', 'UNSPECIFIED' ) ;
#76545 = CARTESIAN_POINT ( 'NONE',  ( -20.51402961445061734, 6.013860829077147585, -1.500000000000002220 ) ) ;
#76546 = CARTESIAN_POINT ( 'NONE',  ( -62.49924954558335344, -24.34968618360933945, 0.1864209137778798930 ) ) ;
#76547 = LINE ( 'NONE', #54248, #88477 ) ;
#76548 = CARTESIAN_POINT ( 'NONE',  ( -20.27875734969026311, -4.776774720514394446, 24.00402280011862288 ) ) ;
#76549 = LINE ( 'NONE', #44628, #94386 ) ;
#76550 = CARTESIAN_POINT ( 'NONE',  ( 4.564784964189898098, -22.25151590922551748, -1.500000000000002220 ) ) ;
#76551 = AXIS2_PLACEMENT_3D ( 'NONE', #67352, #97783, #28275 ) ;
#76552 = EDGE_LOOP ( 'NONE', ( #34222, #88659, #35594, #17358 ) ) ;
#76553 = PLANE ( 'NONE',  #48265 ) ;
#76554 = DIRECTION ( 'NONE',  ( 0.000000000000000000, -2.173523156925980399E-06, 0.9999999999976378895 ) ) ;
#76555 = CARTESIAN_POINT ( 'NONE',  ( -17.21045110277357182, -9.822940424218707278, 11.49999999999999645 ) ) ;
#76556 = EDGE_CURVE ( 'NONE', #53799, #64682, #38743, .T. ) ;
#76557 = VECTOR ( 'NONE', #80900, 1000.000000000000000 ) ;
#76558 = LINE ( 'NONE', #6568, #3617 ) ;
#76559 = B_SPLINE_CURVE_WITH_KNOTS ( 'NONE', 3,
 ( #65915, #80609, #50666, #11099, #96832, #73502 ),
 .UNSPECIFIED., .F., .F.,
 ( 4, 2, 4 ),
 ( 6.384118678604741492E-06, 0.001386860460828369997, 0.002767336802978134520 ),
 .UNSPECIFIED. ) ;
#76560 = ORIENTED_EDGE ( 'NONE', *, *, #15538, .F. ) ;
#76561 = DIRECTION ( 'NONE',  ( -0.9822594791677485837, 0.000000000000000000, 0.1875268396392986980 ) ) ;
#76562 = EDGE_CURVE ( 'NONE', #95664, #4551, #11725, .T. ) ;
#76563 = CARTESIAN_POINT ( 'NONE',  ( -28.98875734969026041, -3.316774720514426456, 26.43402280011862615 ) ) ;
#76564 = CARTESIAN_POINT ( 'NONE',  ( 19.28387207504633949, -9.851753786812027514, 11.49999999999998934 ) ) ;
#76565 = DIRECTION ( 'NONE',  ( 3.773278334444166432E-23, -1.000000000000000000, 0.000000000000000000 ) ) ;
#76566 = CARTESIAN_POINT ( 'NONE',  ( 16.42231304340664266, 10.40281881132301045, -1.500000000000002220 ) ) ;
#76567 = B_SPLINE_CURVE_WITH_KNOTS ( 'NONE', 3,
 ( #95001, #93997, #3178, #55453 ),
 .UNSPECIFIED., .F., .F.,
 ( 4, 4 ),
 ( 0.2907075871721704341, 0.2997140184442859678 ),
 .UNSPECIFIED. ) ;
#76568 = EDGE_CURVE ( 'NONE', #93974, #48086, #64047, .T. ) ;
#76569 = CARTESIAN_POINT ( 'NONE',  ( 11.62916340711181284, 0.3587747205144265483, 28.75961759920349792 ) ) ;
#76570 = CARTESIAN_POINT ( 'NONE',  ( -82.62287095715007013, -24.66019654487199375, 8.947790411086128159 ) ) ;
#76571 = CARTESIAN_POINT ( 'NONE',  ( 6.388261542594571019, -18.74682169789839392, -1.500000000000002220 ) ) ;
#76572 = EDGE_LOOP ( 'NONE', ( #51338, #81894, #41388, #47961 ) ) ;
#76573 = EDGE_CURVE ( 'NONE', #63613, #47693, #81427, .T. ) ;
#76574 = CARTESIAN_POINT ( 'NONE',  ( -13.46841296510753061, 15.22696965993213070, 11.49999999999999645 ) ) ;
#76575 = FACE_OUTER_BOUND ( 'NONE', #35987, .T. ) ;
#76576 = EDGE_CURVE ( 'NONE', #14843, #44696, #61506, .T. ) ;
#76577 = CARTESIAN_POINT ( 'NONE',  ( 33.24104357593923709, -3.536202174476160920, -12.73333860248705740 ) ) ;
#76578 = EDGE_LOOP ( 'NONE', ( #34849, #52804, #28415, #69499 ) ) ;
#76579 = CARTESIAN_POINT ( 'NONE',  ( -0.1187647035275026935, -21.51249758272363621, -1.017619990082605952 ) ) ;
#76580 = DIRECTION ( 'NONE',  ( 0.000000000000000000, -0.9999999999976377785, -2.173523156925979975E-06 ) ) ;
#76581 = CARTESIAN_POINT ( 'NONE',  ( -48.95379770480546711, -25.25214592170422279, 5.698183657943237890 ) ) ;
#76582 = DIRECTION ( 'NONE',  ( 1.000000000000000000, -0.000000000000000000, -0.000000000000000000 ) ) ;
#76583 = CARTESIAN_POINT ( 'NONE',  ( -82.52287095715006160, -23.47596703998600631, 11.44779298504228571 ) ) ;
#76584 = CARTESIAN_POINT ( 'NONE',  ( -18.39468835979788608, -8.022455445098881199, 11.49999999999998934 ) ) ;
#76585 = EDGE_CURVE ( 'NONE', #43203, #27745, #96732, .T. ) ;
#76586 = LINE ( 'NONE', #67506, #96944 ) ;
#76587 = VECTOR ( 'NONE', #1639, 1000.000000000000000 ) ;
#76588 = VERTEX_POINT ( 'NONE', #16914 ) ;
#76589 = DIRECTION ( 'NONE',  ( -1.000000000000000000, -0.000000000000000000, -0.000000000000000000 ) ) ;
#76590 = CARTESIAN_POINT ( 'NONE',  ( 0.5590224530292132732, -22.91010021869659852, 11.49999999999999645 ) ) ;
#76591 = CARTESIAN_POINT ( 'NONE',  ( 18.72737137862276313, -12.84423604280260278, -1.500000000000002220 ) ) ;
#76592 = CARTESIAN_POINT ( 'NONE',  ( -30.47287095715008221, -24.04764615585419207, -0.4449263091658831604 ) ) ;
#76593 = AXIS2_PLACEMENT_3D ( 'NONE', #86325, #31530, #85824 ) ;
#76594 = CARTESIAN_POINT ( 'NONE',  ( 26.73860345374794534, -1.682774720514426114, -7.113848178280766099 ) ) ;
#76595 = CARTESIAN_POINT ( 'NONE',  ( -38.58103285119013037, -24.51419770103157703, 9.386484678747176957 ) ) ;
#76596 = CARTESIAN_POINT ( 'NONE',  ( 30.56047832681638354, -2.297196155479634516, 24.67598410064775649 ) ) ;
#76597 = DIRECTION ( 'NONE',  ( -0.6599726524652352877, 0.000000000000000000, 0.7512896232465892110 ) ) ;
#76598 = DIRECTION ( 'NONE',  ( -1.000000000000000000, -3.773278334444167608E-23, -8.201307833595939069E-29 ) ) ;
#76599 = ORIENTED_EDGE ( 'NONE', *, *, #29700, .T. ) ;
#76600 = CARTESIAN_POINT ( 'NONE',  ( 19.83649001621966335, 4.521578618930774951, 11.49999999999998934 ) ) ;
#76601 = ORIENTED_EDGE ( 'NONE', *, *, #47500, .F. ) ;
#76602 = EDGE_CURVE ( 'NONE', #81766, #94651, #62599, .T. ) ;
#76603 = CARTESIAN_POINT ( 'NONE',  ( 20.74614131242519477, 9.816050768296040729, -1.500000000000002220 ) ) ;
#76604 = CARTESIAN_POINT ( 'NONE',  ( -78.62287095715005592, -29.50247984919015209, -1.443849546365053582 ) ) ;
#76605 = ORIENTED_EDGE ( 'NONE', *, *, #29316, .F. ) ;
#76606 = DIRECTION ( 'NONE',  ( 0.06486421869277853025, 0.000000000000000000, -0.9978940991575084851 ) ) ;
#76607 = CARTESIAN_POINT ( 'NONE',  ( -77.55021002596484436, -24.15620529776628800, 10.23563542870659937 ) ) ;
#76608 = CARTESIAN_POINT ( 'NONE',  ( -51.50148419838348701, -24.15620529776627734, 10.23563542870660470 ) ) ;
#76610 = ORIENTED_EDGE ( 'NONE', *, *, #97862, .F. ) ;
#76609 = CARTESIAN_POINT ( 'NONE',  ( 1.567330217057175901, -21.20382687294985047, 11.49999999999999645 ) ) ;
#76611 = LOCAL_TIME ( 0, 54, 15.00000000000000000, #80969 ) ;
#76612 = VERTEX_POINT ( 'NONE', #40755 ) ;
#76613 = CARTESIAN_POINT ( 'NONE',  ( 4.129723114849880083, -21.82631191821171512, -1.500000000000002220 ) ) ;
#76614 = CARTESIAN_POINT ( 'NONE',  ( -20.24099117049231467, 3.958469829285517161, -1.500000000000002220 ) ) ;
#76615 = EDGE_LOOP ( 'NONE', ( #51912, #87777, #50563, #24581 ) ) ;
#76617 = VERTEX_POINT ( 'NONE', #32134 ) ;
#76616 = CIRCLE ( 'NONE', #29631, 251.4258649670780699 ) ;
#76618 = LINE ( 'NONE', #23333, #57645 ) ;
#76619 = EDGE_CURVE ( 'NONE', #5489, #89924, #59179, .T. ) ;
#76620 = CARTESIAN_POINT ( 'NONE',  ( -36.62287095715005592, -24.64898659630367916, 1.056161002820819261 ) ) ;
#76621 = ORIENTED_EDGE ( 'NONE', *, *, #54136, .T. ) ;
#76622 = CARTESIAN_POINT ( 'NONE',  ( -49.68342748179477297, -25.16659734855911523, 6.901253476643402607 ) ) ;
#76623 = ORIENTED_EDGE ( 'NONE', *, *, #48794, .F. ) ;
#76624 = CIRCLE ( 'NONE', #24781, 19.30000000000000071 ) ;
#76625 = CARTESIAN_POINT ( 'NONE',  ( -126.7287200997190837, -25.23482084814632387, 3.690491797312001943 ) ) ;
#76626 = CARTESIAN_POINT ( 'NONE',  ( -88.62287095715002749, -24.66019654487199730, 8.947790411086128159 ) ) ;
#76627 = CARTESIAN_POINT ( 'NONE',  ( -14.03827505669662479, 15.38897104800697591, -1.500000000000002220 ) ) ;
#76629 = ADVANCED_FACE ( 'NONE', ( #8303 ), #15910, .T. ) ;
#76628 = CARTESIAN_POINT ( 'NONE',  ( 6.829227106855087825, -20.66181959361685827, 11.49999999999999645 ) ) ;
#76630 = CARTESIAN_POINT ( 'NONE',  ( -40.39532865008378337, -25.18518669035473323, 3.295758758853348791 ) ) ;
#76631 = CARTESIAN_POINT ( 'NONE',  ( -71.52287095715007581, -24.65952944569304606, 1.056160979905697239 ) ) ;
#76632 = CARTESIAN_POINT ( 'NONE',  ( -18.83616483605274539, -12.25834331966736102, -1.500000000000002220 ) ) ;
#76633 = CARTESIAN_POINT ( 'NONE',  ( -51.26061221361337061, -25.26334635016775465, 4.199398795162026410 ) ) ;
#76634 = ORIENTED_EDGE ( 'NONE', *, *, #58977, .F. ) ;
#76635 = DIRECTION ( 'NONE',  ( -0.9913618264504691080, 0.000000000000000000, 0.1311553622875927805 ) ) ;
#76636 = CARTESIAN_POINT ( 'NONE',  ( 32.23865423223558935, 4.540774720514431095, 2.161924922174277341 ) ) ;
#76637 = B_SPLINE_SURFACE_WITH_KNOTS ( 'NONE', 3, 3, ( 
 ( #29556, #12333, #36677, #29058 ),
 ( #67641, #74243, #14321, #98563 ),
 ( #66663, #4240, #52406, #83342 ),
 ( #13825, #6219, #46285, #94838 ),
 ( #100043, #76710, #40568, #38161 ),
 ( #68629, #30554, #79111, #33440 ),
 ( #61024, #64428, #10106, #48181 ) ),
 .UNSPECIFIED., .F., .F., .F.,
 ( 4, 3, 4 ),
 ( 4, 4 ),
 ( 0.0004766839783822563858, 0.1029713700210899974, 0.2054660560637977251 ),
 ( 0.07951422430824672816, 0.08056363658127665972 ),
 .UNSPECIFIED. ) ;
#76638 = ORIENTED_EDGE ( 'NONE', *, *, #19771, .F. ) ;
#76639 = ORIENTED_EDGE ( 'NONE', *, *, #65140, .F. ) ;
#76640 = APPROVAL ( #47528, 'UNKNOWN' ) ;
#76641 = ORIENTED_EDGE ( 'NONE', *, *, #41518, .T. ) ;
#76642 = CARTESIAN_POINT ( 'NONE',  ( -20.89022842043660688, 4.291957016416017900, -1.500000000000002220 ) ) ;
#76643 = VERTEX_POINT ( 'NONE', #12288 ) ;
#76644 = CARTESIAN_POINT ( 'NONE',  ( -19.58807393344005376, -7.628504261335002923, 11.49999999999998934 ) ) ;
#76645 = CARTESIAN_POINT ( 'NONE',  ( -30.41986401503926274, -24.82632770740921302, 1.633466014234818076 ) ) ;
#76646 = CARTESIAN_POINT ( 'NONE',  ( -41.46355252140796210, -25.18431046067977874, 4.097885018056865114 ) ) ;
#76647 = CARTESIAN_POINT ( 'NONE',  ( -65.52287095715006160, -23.47596703998600631, 11.44779298504228748 ) ) ;
#76648 = CARTESIAN_POINT ( 'NONE',  ( 3.689792033372774060, 21.67897595795444587, -1.500000000000002220 ) ) ;
#76649 = CARTESIAN_POINT ( 'NONE',  ( -87.59490587792481620, -23.96119346886882084, -0.6495511937831871530 ) ) ;
#76650 = ORIENTED_EDGE ( 'NONE', *, *, #21007, .F. ) ;
#76651 = FACE_OUTER_BOUND ( 'NONE', #67583, .T. ) ;
#76652 = VECTOR ( 'NONE', #38593, 1000.000000000000114 ) ;
#76653 = CARTESIAN_POINT ( 'NONE',  ( 31.74473449900405697, -4.976825198871215328, -4.259190951192157293 ) ) ;
#76654 = CARTESIAN_POINT ( 'NONE',  ( -84.56294652207583340, -23.48786465467241769, 11.44779295918254647 ) ) ;
#76655 = CARTESIAN_POINT ( 'NONE',  ( -130.5728709571501724, -25.14064729901805251, 2.712351064733618866 ) ) ;
#76656 = CARTESIAN_POINT ( 'NONE',  ( -20.43222813077822408, -23.69307752509138965, 9.440663514584134219 ) ) ;
#76657 = CARTESIAN_POINT ( 'NONE',  ( -9.338289970059909351, 19.12570833482435617, -1.500000000000002220 ) ) ;
#76658 = PLANE ( 'NONE',  #20733 ) ;
#76659 = DIRECTION ( 'NONE',  ( -3.773278334453080206E-23, 0.9999999999976377785, 2.173523156925979975E-06 ) ) ;
#76660 = CARTESIAN_POINT ( 'NONE',  ( -90.62287095715004170, -23.47593901973091235, -1.443836447539002865 ) ) ;
#76661 = CARTESIAN_POINT ( 'NONE',  ( -33.52641739661655151, -24.65952944569304606, 1.056160979905695907 ) ) ;
#76662 = CARTESIAN_POINT ( 'NONE',  ( 1.861690257272737847, 22.46465895387273903, -1.500000000000002220 ) ) ;
#76663 = DIRECTION ( 'NONE',  ( -0.000000000000000000, -0.9513357669802769978, 0.3081562241202474572 ) ) ;
#76664 = VERTEX_POINT ( 'NONE', #88935 ) ;
#76665 = DIRECTION ( 'NONE',  ( -0.000000000000000000, -1.000000000000000000, -0.000000000000000000 ) ) ;
#76666 = CARTESIAN_POINT ( 'NONE',  ( 13.00645856128228495, 14.71372164842801844, 11.49999999999999645 ) ) ;
#76667 = DIRECTION ( 'NONE',  ( 0.000000000000000000, 0.000000000000000000, -1.000000000000000000 ) ) ;
#76668 = FACE_OUTER_BOUND ( 'NONE', #9144, .T. ) ;
#76669 = ORIENTED_EDGE ( 'NONE', *, *, #4204, .F. ) ;
#76670 = CARTESIAN_POINT ( 'NONE',  ( -88.58575907974172026, -24.51419770103157703, 9.386484678747176957 ) ) ;
#76671 = CARTESIAN_POINT ( 'NONE',  ( -126.7289109336821866, -25.33574223958540017, 6.311323082738798718 ) ) ;
#76672 = CARTESIAN_POINT ( 'NONE',  ( -88.87103898935609436, -25.22174524493127734, 6.695141717414601068 ) ) ;
#76673 = VECTOR ( 'NONE', #90324, 1000.000000000000000 ) ;
#76674 = CARTESIAN_POINT ( 'NONE',  ( -9.502044936771568473, -17.27029980899984452, 11.49999999999998934 ) ) ;
#76675 = B_SPLINE_CURVE_WITH_KNOTS ( 'NONE', 3,
 ( #17026, #9410, #40373, #100238 ),
 .UNSPECIFIED., .F., .F.,
 ( 4, 4 ),
 ( 0.000000000000000000, 9.999999999998897304E-05 ),
 .UNSPECIFIED. ) ;
#76676 = ORIENTED_EDGE ( 'NONE', *, *, #8757, .F. ) ;
#76677 = EDGE_CURVE ( 'NONE', #15184, #96261, #65621, .T. ) ;
#76678 = CARTESIAN_POINT ( 'NONE',  ( 10.86431179148764770, 6.376774720514933215, -28.05678185045468709 ) ) ;
#76679 = FACE_OUTER_BOUND ( 'NONE', #88147, .T. ) ;
#76680 = EDGE_CURVE ( 'NONE', #17192, #53455, #31302, .T. ) ;
#76681 = VECTOR ( 'NONE', #75836, 1000.000000000000000 ) ;
#76682 = COORDINATED_UNIVERSAL_TIME_OFFSET ( 0, 0, .AHEAD. ) ;
#76683 = VERTEX_POINT ( 'NONE', #19410 ) ;
#76684 = CARTESIAN_POINT ( 'NONE',  ( -79.62287095715005592, -29.50247984919015209, -1.443849546365053582 ) ) ;
#76685 = DIRECTION ( 'NONE',  ( -0.000000000000000000, 1.000000000000000000, -0.000000000000000000 ) ) ;
#76686 = CARTESIAN_POINT ( 'NONE',  ( -55.48003037949258953, -24.92564183028978775, 1.928384488918253092 ) ) ;
#76687 = DIRECTION ( 'NONE',  ( 0.9975640502598247528, -0.06975647374411753088, 0.000000000000000000 ) ) ;
#76688 = DIRECTION ( 'NONE',  ( -1.334402673828313093E-16, -0.000000000000000000, -1.000000000000000000 ) ) ;
#76689 = DIRECTION ( 'NONE',  ( 0.000000000000000000, -0.000000000000000000, -1.000000000000000000 ) ) ;
#76690 = AXIS2_PLACEMENT_3D ( 'NONE', #85159, #55736, #100362 ) ;
#76691 = B_SPLINE_CURVE_WITH_KNOTS ( 'NONE', 3,
 ( #86443, #85946, #84441, #99648 ),
 .UNSPECIFIED., .F., .F.,
 ( 4, 4 ),
 ( 0.000000000000000000, 9.999999999996123101E-05 ),
 .UNSPECIFIED. ) ;
#76692 = DIRECTION ( 'NONE',  ( -3.773278334444167608E-23, 1.000000000000000000, 0.000000000000000000 ) ) ;
#76693 = CARTESIAN_POINT ( 'NONE',  ( 19.98059151383774434, -0.7942727526097331792, 11.49999999999998934 ) ) ;
#76694 = ADVANCED_FACE ( 'NONE', ( #72717, #73216 ), #74691, .F. ) ;
#76695 = DIRECTION ( 'NONE',  ( 0.000000000000000000, 0.000000000000000000, -1.000000000000000000 ) ) ;
#76696 = CARTESIAN_POINT ( 'NONE',  ( -51.68123905711060928, -25.28846605061042396, 4.189028613740050311 ) ) ;
#76697 = EDGE_LOOP ( 'NONE', ( #2714, #74910, #71312, #68937, #33068 ) ) ;
#76698 = CARTESIAN_POINT ( 'NONE',  ( -119.5893898853676802, -24.34968618360934656, 0.1864209137778924386 ) ) ;
#76699 = DIRECTION ( 'NONE',  ( -0.000000000000000000, 1.000000000000000000, -0.000000000000000000 ) ) ;
#76700 = CARTESIAN_POINT ( 'NONE',  ( 29.73860345376318293, 5.356514366721292220, 19.42370904364366169 ) ) ;
#76701 = CARTESIAN_POINT ( 'NONE',  ( -100.5228709571501184, -24.92604778743017846, 8.074972756849364330 ) ) ;
#76702 = DIRECTION ( 'NONE',  ( 0.000000000000000000, 1.000000000000000000, 0.000000000000000000 ) ) ;
#76703 = CARTESIAN_POINT ( 'NONE',  ( -3.108974358974359475, -6.376774720514417183, 20.36458333333334281 ) ) ;
#76704 = B_SPLINE_CURVE_WITH_KNOTS ( 'NONE', 3,
 ( #45698, #84245, #16242, #23336, #47203, #46704 ),
 .UNSPECIFIED., .F., .F.,
 ( 4, 2, 4 ),
 ( 1.570887131794638196E-05, 0.001396322306279758904, 0.002776935741241571502 ),
 .UNSPECIFIED. ) ;
#76705 = B_SPLINE_SURFACE_WITH_KNOTS ( 'NONE', 3, 3, ( 
 ( #59573, #90504, #37221, #15365 ),
 ( #29597, #45341, #38207, #13870 ),
 ( #75273, #51954, #46328, #20982 ),
 ( #6757, #5766, #98608, #44841 ),
 ( #37713, #68671, #99592, #30095 ),
 ( #61068, #22466, #53457, #84385 ),
 ( #14865, #45833, #23464, #41226 ) ),
 .UNSPECIFIED., .F., .F., .F.,
 ( 4, 3, 4 ),
 ( 4, 4 ),
 ( 0.7945040050992236980, 0.8970133687736500105, 0.9995227324480763231 ),
 ( 0.6296540010513237418, 0.6309574156764954367 ),
 .UNSPECIFIED. ) ;
#76706 = LINE ( 'NONE', #67637, #88444 ) ;
#76707 = CARTESIAN_POINT ( 'NONE',  ( 0.3085469314987323020, -5.876774720514413630, 19.52341893546493523 ) ) ;
#76708 = ORIENTED_EDGE ( 'NONE', *, *, #56606, .T. ) ;
#76709 = CARTESIAN_POINT ( 'NONE',  ( -12.33117494125061242, 16.09929768045241261, 11.49999999999998934 ) ) ;
#76710 = CARTESIAN_POINT ( 'NONE',  ( -122.5894821100217769, -24.34968618360934300, 0.1864209137778896352 ) ) ;
#76711 = DIRECTION ( 'NONE',  ( -1.000000000000000000, -3.773278334444166432E-23, -8.201307841325785021E-29 ) ) ;
#76712 = CARTESIAN_POINT ( 'NONE',  ( -105.6228709571500559, -24.92579138211018375, 1.929029949965666457 ) ) ;
#76713 = VERTEX_POINT ( 'NONE', #3704 ) ;
#76715 = EDGE_CURVE ( 'NONE', #22708, #35597, #4698, .T. ) ;
#76714 = PLANE ( 'NONE',  #50205 ) ;
#76716 = CARTESIAN_POINT ( 'NONE',  ( -16.19606052442943067, -11.93128464602566474, -1.500000000000002220 ) ) ;
#76717 = AXIS2_PLACEMENT_3D ( 'NONE', #74443, #27280, #11542 ) ;
#76718 = CARTESIAN_POINT ( 'NONE',  ( -8.250207518706217158, 19.40231308534122689, 11.49999999999999645 ) ) ;
#76719 = CARTESIAN_POINT ( 'NONE',  ( -64.62287095715005592, -24.66019654487198665, 8.947790411086131712 ) ) ;
#76720 = CARTESIAN_POINT ( 'NONE',  ( 18.18892703665305177, -12.56521834855340281, -1.500000000000002220 ) ) ;
#76721 = EDGE_CURVE ( 'NONE', #29240, #34994, #18017, .T. ) ;
#76722 = CARTESIAN_POINT ( 'NONE',  ( 20.52540449432101610, 0.9483640940595650104, -1.500000000000002220 ) ) ;
#76723 = CARTESIAN_POINT ( 'NONE',  ( -61.24303164512834030, -25.04307381209219230, 7.563174986197129357 ) ) ;
#76724 = CARTESIAN_POINT ( 'NONE',  ( 14.92699176545193041, 5.063793094955937768, -27.26229911407734008 ) ) ;
#76725 = EDGE_LOOP ( 'NONE', ( #3895, #28102, #34675, #57702 ) ) ;
#76726 = CARTESIAN_POINT ( 'NONE',  ( -7.326923076923074873, -6.376774720514427841, 21.75000000000001066 ) ) ;
#76727 = ORIENTED_EDGE ( 'NONE', *, *, #19298, .F. ) ;
#76728 = CARTESIAN_POINT ( 'NONE',  ( -96.62287095715005592, -29.50247984919015209, -1.443849546365050029 ) ) ;
#76729 = CARTESIAN_POINT ( 'NONE',  ( -67.62287095715008434, -23.47596703998600276, 11.44779298504227505 ) ) ;
#76730 = ORIENTED_EDGE ( 'NONE', *, *, #59876, .T. ) ;
#76731 = ORIENTED_EDGE ( 'NONE', *, *, #86808, .F. ) ;
#76732 = VERTEX_POINT ( 'NONE', #50379 ) ;
#76733 = CARTESIAN_POINT ( 'NONE',  ( -51.70072539166533687, -25.26311289191998455, 3.987152081390995306 ) ) ;
#76734 = DIRECTION ( 'NONE',  ( 1.000000000000000000, 3.773278334444167608E-23, 8.201307833595939069E-29 ) ) ;
#76735 = DIRECTION ( 'NONE',  ( -3.773278334453079618E-23, 0.9999999999976377785, 2.173523156925979552E-06 ) ) ;
#76736 = CARTESIAN_POINT ( 'NONE',  ( 10.61356161029474521, 17.70173163822984819, -1.500000000000002220 ) ) ;
#76737 = CARTESIAN_POINT ( 'NONE',  ( 4.348677445931066643, 21.19853102677161871, 11.49999999999999645 ) ) ;
#76738 = ORIENTED_EDGE ( 'NONE', *, *, #81393, .F. ) ;
#76739 = CARTESIAN_POINT ( 'NONE',  ( -80.35919894935767616, -25.29542306156489673, 4.505481338088394239 ) ) ;
#76740 = CARTESIAN_POINT ( 'NONE',  ( 3.769940963823357638, -5.876774720514402972, 18.16074422543206879 ) ) ;
#76741 = CARTESIAN_POINT ( 'NONE',  ( -18.94483701893047467, 11.91932228829616669, 11.49999999999998934 ) ) ;
#76742 = B_SPLINE_CURVE_WITH_KNOTS ( 'NONE', 3,
 ( #83314, #51383, #4710, #35663, #82324, #43774, #59495, #29526 ),
 .UNSPECIFIED., .F., .F.,
 ( 4, 2, 2, 4 ),
 ( -0.001224554619866350400, -0.0002241820295893703040, 0.0007761905606876097919, 0.002776935741241571068 ),
 .UNSPECIFIED. ) ;
#76743 = CARTESIAN_POINT ( 'NONE',  ( -80.37464638460068045, -25.12205811127329014, 7.098502408654610463 ) ) ;
#76744 = CARTESIAN_POINT ( 'NONE',  ( -84.54750306560438844, -24.34968618360934300, 0.1864209137778835013 ) ) ;
#76745 = ORIENTED_EDGE ( 'NONE', *, *, #95384, .T. ) ;
#76746 = CARTESIAN_POINT ( 'NONE',  ( -60.62287095715004881, -24.99156045073392463, 7.747789690856161648 ) ) ;
#76747 = CARTESIAN_POINT ( 'NONE',  ( -49.54715521573665171, -24.15620529776627379, 10.23563542870661003 ) ) ;
#76748 = CARTESIAN_POINT ( 'NONE',  ( -115.5228709571500474, -24.91544648472620338, 1.928969306349230584 ) ) ;
#76749 = CARTESIAN_POINT ( 'NONE',  ( -20.86263692406621928, 1.606387762444034362, 11.49999999999998934 ) ) ;
#76750 = EDGE_LOOP ( 'NONE', ( #88418, #95232, #89615, #8279 ) ) ;
#76751 = ADVANCED_FACE ( 'NONE', ( #58003 ), #28518, .F. ) ;
#76753 = ORIENTED_EDGE ( 'NONE', *, *, #90090, .T. ) ;
#76752 = CARTESIAN_POINT ( 'NONE',  ( -86.59885310783221257, -23.73766607897671221, -1.055555164236432697 ) ) ;
#76754 = ORIENTED_EDGE ( 'NONE', *, *, #44863, .F. ) ;
#76755 = VECTOR ( 'NONE', #4582, 1000.000000000000114 ) ;
#76756 = CARTESIAN_POINT ( 'NONE',  ( -109.5222136401132502, -23.48786465467241769, 11.44779295918253759 ) ) ;
#76757 = CARTESIAN_POINT ( 'NONE',  ( -14.54676392617323266, -15.37779485849079464, -1.500000000000002220 ) ) ;
#76758 = EDGE_LOOP ( 'NONE', ( #78731, #100329, #22793, #40439 ) ) ;
#76759 = CARTESIAN_POINT ( 'NONE',  ( -117.5222355478601060, -23.48783264082477729, -1.443836473390081254 ) ) ;
#76760 = CARTESIAN_POINT ( 'NONE',  ( -42.62287095715004881, -29.50250243563736774, 8.947779886222148704 ) ) ;
#76761 = CARTESIAN_POINT ( 'NONE',  ( -21.76810506448615712, 0.6044244127108716613, 11.49999999999998934 ) ) ;
#76762 = CARTESIAN_POINT ( 'NONE',  ( -7.617563585130437076, -6.376774720514411854, 19.95084900476494383 ) ) ;
#76763 = CARTESIAN_POINT ( 'NONE',  ( 5.356969261897235768, -0.3587747205143965168, -28.55262118024313978 ) ) ;
#76764 = CARTESIAN_POINT ( 'NONE',  ( 31.55236408230781819, -0.6647747205144264315, 19.84760796525321780 ) ) ;
#76765 = CARTESIAN_POINT ( 'NONE',  ( -9.857415191643349672, 19.42730305858377449, -1.500000000000002220 ) ) ;
#76766 = CARTESIAN_POINT ( 'NONE',  ( -71.70689869863497279, -25.24674333672842508, 6.146638408343236826 ) ) ;
#76767 = ORIENTED_EDGE ( 'NONE', *, *, #29059, .F. ) ;
#76768 = CARTESIAN_POINT ( 'NONE',  ( 11.04644962722740864, -4.132774720514426292, -26.87113206189456704 ) ) ;
#76769 = CARTESIAN_POINT ( 'NONE',  ( -117.5228709571500758, -24.64898659630368272, 1.056161002820833028 ) ) ;
#76770 = DIRECTION ( 'NONE',  ( 0.000000000000000000, -1.000000000000000000, 0.000000000000000000 ) ) ;
#76771 = VERTEX_POINT ( 'NONE', #18909 ) ;
#76772 = EDGE_CURVE ( 'NONE', #91650, #84010, #53069, .T. ) ;
#76773 = ORIENTED_EDGE ( 'NONE', *, *, #52181, .T. ) ;
#76774 = ORIENTED_EDGE ( 'NONE', *, *, #66550, .T. ) ;
#76775 = CARTESIAN_POINT ( 'NONE',  ( 5.202077965628057576, 2.038091937962834166, 2.869745073849996442E-16 ) ) ;
#76776 = CARTESIAN_POINT ( 'NONE',  ( 18.66760434907605060, -10.05535386721697222, 11.49999999999998934 ) ) ;
#76777 = DIRECTION ( 'NONE',  ( -0.000000000000000000, 1.000000000000000000, -0.000000000000000000 ) ) ;
#76778 = CARTESIAN_POINT ( 'NONE',  ( -95.62287095715005592, -24.99156045073393173, 7.747789690856161648 ) ) ;
#76779 = DIRECTION ( 'NONE',  ( -0.06975647374412546897, -0.9975640502598241977, 0.000000000000000000 ) ) ;
#76780 = CARTESIAN_POINT ( 'NONE',  ( -27.61845239340658154, 5.965225279485594001, -10.37513603161905351 ) ) ;
#76781 = CARTESIAN_POINT ( 'NONE',  ( -18.22047185089115828, 6.579378235550767506, -1.500000000000002220 ) ) ;
#76782 = B_SPLINE_CURVE_WITH_KNOTS ( 'NONE', 3,
 ( #41847, #80392, #57073, #40825 ),
 .UNSPECIFIED., .F., .F.,
 ( 4, 4 ),
 ( 0.000000000000000000, 9.999999999997510880E-05 ),
 .UNSPECIFIED. ) ;
#76783 = CARTESIAN_POINT ( 'NONE',  ( -70.29579152553412769, -25.31157247813958122, 5.315013286592739306 ) ) ;
#76784 = VERTEX_POINT ( 'NONE', #11306 ) ;
#76785 = CARTESIAN_POINT ( 'NONE',  ( -11.39837868854680814, -15.77482985264681403, 11.49999999999999645 ) ) ;
#76786 = CARTESIAN_POINT ( 'NONE',  ( -42.52287095715006870, -23.95044443724991368, 10.65354141964649415 ) ) ;
#76787 = EDGE_CURVE ( 'NONE', #5690, #63070, #73704, .T. ) ;
#76788 = EDGE_CURVE ( 'NONE', #62952, #42367, #37133, .T. ) ;
#76789 = FACE_OUTER_BOUND ( 'NONE', #67291, .T. ) ;
#76790 = ORIENTED_EDGE ( 'NONE', *, *, #41680, .F. ) ;
#76791 = AXIS2_PLACEMENT_3D ( 'NONE', #19451, #27582, #67154 ) ;
#76792 = CARTESIAN_POINT ( 'NONE',  ( 3.183477995988301945, -6.376774720514404748, 18.35601591497023577 ) ) ;
#76793 = LINE ( 'NONE', #191, #4272 ) ;
#76794 = CARTESIAN_POINT ( 'NONE',  ( -91.62287095715002749, -23.95044443724991368, 10.65354141964649592 ) ) ;
#76795 = CARTESIAN_POINT ( 'NONE',  ( -101.3738023147422638, -25.26303730729093999, 3.986250639247583827 ) ) ;
#76796 = CARTESIAN_POINT ( 'NONE',  ( 19.40334540789412188, 3.064012487144803565, -1.500000000000002220 ) ) ;
#76797 = AXIS2_PLACEMENT_3D ( 'NONE', #10868, #19964, #41833 ) ;
#76798 = CARTESIAN_POINT ( 'NONE',  ( -41.44897309030830712, -25.27805984287601504, 4.366647756403065017 ) ) ;
#76799 = EDGE_LOOP ( 'NONE', ( #74366, #48261, #792, #56333 ) ) ;
#76800 = CARTESIAN_POINT ( 'NONE',  ( 5.689979955356517571, -20.79666814084963278, -1.500000000000002220 ) ) ;
#76801 = CARTESIAN_POINT ( 'NONE',  ( -33.57506839788266007, -24.66019654487198665, 8.947790411086133489 ) ) ;
#76802 = CARTESIAN_POINT ( 'NONE',  ( -74.22287095715006444, -23.47593901973090169, -1.443836447538997536 ) ) ;
#76803 = CARTESIAN_POINT ( 'NONE',  ( -80.52287095715006160, -25.00158670708909625, 2.256160236439166411 ) ) ;
#76804 = CARTESIAN_POINT ( 'NONE',  ( -1.973530150111237003, 22.95712487800313539, -1.500000000000002220 ) ) ;
#76805 = EDGE_CURVE ( 'NONE', #31023, #54552, #82802, .T. ) ;
#76806 = EDGE_CURVE ( 'NONE', #24519, #33217, #77296, .T. ) ;
#76807 = DATE_AND_TIME ( #16414, #19766 ) ;
#76808 = LINE ( 'NONE', #46380, #79096 ) ;
#76809 = LINE ( 'NONE', #7308, #37709 ) ;
#76810 = CARTESIAN_POINT ( 'NONE',  ( 5.087728227403598424, 19.53446797131710611, 11.49999999999999645 ) ) ;
#76811 = CARTESIAN_POINT ( 'NONE',  ( -121.6234957283108145, -24.66019654487200441, 8.947790411086119278 ) ) ;
#76812 = CARTESIAN_POINT ( 'NONE',  ( -101.7020366304713832, -25.16380645952672168, 6.919780044220484427 ) ) ;
#76813 = CARTESIAN_POINT ( 'NONE',  ( -110.4629859055347936, -25.10921374666837735, 2.835693975498917663 ) ) ;
#76814 = LINE ( 'NONE', #84444, #95884 ) ;
#76815 = CARTESIAN_POINT ( 'NONE',  ( -110.9796143976588070, -25.18425627932603916, 3.502226522025594591 ) ) ;
#76816 = CARTESIAN_POINT ( 'NONE',  ( 19.48829924427396421, 3.997931079995220127, 11.49999999999998934 ) ) ;
#76817 = EDGE_CURVE ( 'NONE', #86369, #55468, #11902, .T. ) ;
#76818 = CARTESIAN_POINT ( 'NONE',  ( -15.87499999999997868, 0.000000000000000000, 0.000000000000000000 ) ) ;
#76819 = CARTESIAN_POINT ( 'NONE',  ( 18.78060722631472501, -6.265068672152646734, -1.500000000000002220 ) ) ;
#76820 = CARTESIAN_POINT ( 'NONE',  ( -24.97666371003640151, -5.965225279485592225, -15.72894043976419098 ) ) ;
#76821 = ADVANCED_FACE ( 'NONE', ( #5683 ), #46718, .T. ) ;
#76822 = CARTESIAN_POINT ( 'NONE',  ( -39.73251464975087544, -25.10925631031845384, 3.010156874704200902 ) ) ;
#76823 = DIRECTION ( 'NONE',  ( -0.7512896232465891000, 0.000000000000000000, -0.6599726524652352877 ) ) ;
#76824 = CARTESIAN_POINT ( 'NONE',  ( -14.15296684469643118, 15.14645709676483420, 11.49999999999999645 ) ) ;
#76825 = LINE ( 'NONE', #74842, #87240 ) ;
#76826 = CARTESIAN_POINT ( 'NONE',  ( -50.26765004257320868, -25.31439277774918395, 5.200244519690546241 ) ) ;
#76827 = CARTESIAN_POINT ( 'NONE',  ( -18.45961786539058380, -13.25243217869837231, 11.49999999999999645 ) ) ;
#76828 = ORIENTED_EDGE ( 'NONE', *, *, #17885, .F. ) ;
#76829 = CARTESIAN_POINT ( 'NONE',  ( -0.005606649364735081555, -5.876774720514410077, 19.25713806424188235 ) ) ;
#76830 = B_SPLINE_CURVE_WITH_KNOTS ( 'NONE', 3,
 ( #44853, #14376, #76274, #46337 ),
 .UNSPECIFIED., .F., .F.,
 ( 4, 4 ),
 ( 1.387778780781445676E-17, 0.0001000000000000028508 ),
 .UNSPECIFIED. ) ;
#76831 = PLANE ( 'NONE',  #7907 ) ;
#76832 = CARTESIAN_POINT ( 'NONE',  ( -19.98115086844608612, 2.773124471107000666, 11.49999999999998934 ) ) ;
#76833 = DIRECTION ( 'NONE',  ( 0.8788171126619707119, -0.4771587602595985800, 0.000000000000000000 ) ) ;
#76834 = DIRECTION ( 'NONE',  ( 0.000000000000000000, 0.000000000000000000, 1.000000000000000000 ) ) ;
#76835 = ORIENTED_EDGE ( 'NONE', *, *, #77591, .T. ) ;
#76836 = VERTEX_POINT ( 'NONE', #76181 ) ;
#76837 = CARTESIAN_POINT ( 'NONE',  ( -73.52287095715007581, -24.65952944569304606, 1.056160979905697239 ) ) ;
#76838 = CARTESIAN_POINT ( 'NONE',  ( -13.69284064830502423, 18.33895024417757469, -1.500000000000002220 ) ) ;
#76839 = CARTESIAN_POINT ( 'NONE',  ( -50.97853604095990221, -25.18439684119721278, 3.451784566745564664 ) ) ;
#76840 = CARTESIAN_POINT ( 'NONE',  ( -6.031157642910047301, -20.80930661755759203, -1.500000000000002220 ) ) ;
#76841 = CARTESIAN_POINT ( 'NONE',  ( -90.62287095715004170, -29.50250243563736774, 8.947779886222139822 ) ) ;
#76842 = CARTESIAN_POINT ( 'NONE',  ( 11.56983764158150052, -5.965225279485572685, 28.29037853177889517 ) ) ;
#76843 = CARTESIAN_POINT ( 'NONE',  ( -0.7727808018759799724, -20.89725122839497828, 11.49999999999999645 ) ) ;
#76844 = ORIENTED_EDGE ( 'NONE', *, *, #96170, .F. ) ;
#76845 = CARTESIAN_POINT ( 'NONE',  ( -124.6256202920364586, -23.73766607897671577, -1.055555164236449572 ) ) ;
#76846 = CARTESIAN_POINT ( 'NONE',  ( -18.24146354680218707, 12.35505607031776165, 11.49999999999998934 ) ) ;
#76847 = VECTOR ( 'NONE', #14186, 1000.000000000000114 ) ;
#76848 = DIRECTION ( 'NONE',  ( 0.000000000000000000, -1.000000000000000000, 0.000000000000000000 ) ) ;
#76849 = CARTESIAN_POINT ( 'NONE',  ( -40.43756433397305727, -25.29087034402937206, 2.832404424902956297 ) ) ;
#76851 = ORIENTED_EDGE ( 'NONE', *, *, #37851, .F. ) ;
#76850 = ADVANCED_FACE ( 'NONE', ( #91409 ), #21887, .T. ) ;
#76852 = CARTESIAN_POINT ( 'NONE',  ( 30.93860345374796594, 2.297196155479665158, 24.67598410064776715 ) ) ;
#76854 = ADVANCED_FACE ( 'NONE', ( #51873 ), #77470, .T. ) ;
#76853 = FACE_OUTER_BOUND ( 'NONE', #78117, .T. ) ;
#76855 = VERTEX_POINT ( 'NONE', #47256 ) ;
#76856 = CARTESIAN_POINT ( 'NONE',  ( -72.58424668660525469, -24.51419770103156281, 9.386484678747185839 ) ) ;
#76857 = VERTEX_POINT ( 'NONE', #62997 ) ;
#76858 = VERTEX_POINT ( 'NONE', #33031 ) ;
#76859 = CARTESIAN_POINT ( 'NONE',  ( -71.58081214425558869, -24.66019654487199730, 8.947790411086113949 ) ) ;
#76860 = DIRECTION ( 'NONE',  ( -3.773278334453079030E-23, 0.9999999999976377785, 2.173523156925979128E-06 ) ) ;
#76861 = CARTESIAN_POINT ( 'NONE',  ( -4.289200894924355190, -6.376774720514413630, 19.85590024959437017 ) ) ;
#76862 = CARTESIAN_POINT ( 'NONE',  ( -11.47117155886032158, -16.94740806926979815, -1.500000000000002220 ) ) ;
#76863 = AXIS2_PLACEMENT_3D ( 'NONE', #3907, #58678, #66311 ) ;
#76864 = VERTEX_POINT ( 'NONE', #46755 ) ;
#76865 = CARTESIAN_POINT ( 'NONE',  ( -3.004714864173751998, -6.376774720514411854, 19.63296556618507083 ) ) ;
#76866 = CARTESIAN_POINT ( 'NONE',  ( -10.40290173325841216, 5.356774720514425603, 27.45402280011861862 ) ) ;
#76867 = DIRECTION ( 'NONE',  ( 0.1478094111296165969, -0.9890158633619159367, 0.000000000000000000 ) ) ;
#76868 = CARTESIAN_POINT ( 'NONE',  ( 10.93216147639808611, 19.43004700418156361, -1.500000000000002220 ) ) ;
#76869 = CARTESIAN_POINT ( 'NONE',  ( -4.930333147521421822, -6.376774720514410077, 19.46306892155547530 ) ) ;
#76870 = CARTESIAN_POINT ( 'NONE',  ( -28.32169924589829080, 5.965225279485592225, -8.244178532169447848 ) ) ;
#76871 = VERTEX_POINT ( 'NONE', #17807 ) ;
#76872 = DIRECTION ( 'NONE',  ( 0.000000000000000000, -1.000000000000000000, 0.000000000000000000 ) ) ;
#76873 = CARTESIAN_POINT ( 'NONE',  ( -29.21927636257191807, -24.63645895185818802, 7.471892006582644186 ) ) ;
#76874 = CARTESIAN_POINT ( 'NONE',  ( -18.54028579900546703, -9.471972883075929772, -1.500000000000002220 ) ) ;
#76875 = VERTEX_POINT ( 'NONE', #25413 ) ;
#76877 = VERTEX_POINT ( 'NONE', #63501 ) ;
#76876 = CARTESIAN_POINT ( 'NONE',  ( -28.47875734969025885, 5.965225279485572685, -0.08597719988136941216 ) ) ;
#76878 = EDGE_CURVE ( 'NONE', #77258, #88353, #8694, .T. ) ;
#76879 = LINE ( 'NONE', #15991, #98922 ) ;
#76880 = VERTEX_POINT ( 'NONE', #16796 ) ;
#76881 = ORIENTED_EDGE ( 'NONE', *, *, #41768, .T. ) ;
#76882 = PLANE ( 'NONE',  #43005 ) ;
#76883 = CARTESIAN_POINT ( 'NONE',  ( -80.62287095715005592, -24.99156045073393173, 7.747789690856161648 ) ) ;
#76884 = DIRECTION ( 'NONE',  ( -0.000000000000000000, 1.000000000000000000, -0.000000000000000000 ) ) ;
#76885 = EDGE_CURVE ( 'NONE', #79998, #59480, #13146, .T. ) ;
#76886 = CARTESIAN_POINT ( 'NONE',  ( -40.62287095715004170, -25.00182538069145011, 7.747789668545099317 ) ) ;
#76887 = B_SPLINE_CURVE_WITH_KNOTS ( 'NONE', 3,
 ( #87615, #49063, #18098, #79991, #10479, #31781 ),
 .UNSPECIFIED., .F., .F.,
 ( 4, 2, 4 ),
 ( 1.570755371633993761E-05, 0.001396183895866089271, 0.002776660238015838614 ),
 .UNSPECIFIED. ) ;
#76888 = CARTESIAN_POINT ( 'NONE',  ( -109.4786293639607493, -25.16483953145740671, 3.092510198109223118 ) ) ;
#76889 = DIRECTION ( 'NONE',  ( -1.000000000000000000, 0.000000000000000000, 0.000000000000000000 ) ) ;
#76891 = ORIENTED_EDGE ( 'NONE', *, *, #94325, .T. ) ;
#76890 = CARTESIAN_POINT ( 'NONE',  ( -2.513997614918375589, -22.02279109229760223, 11.49999999999999645 ) ) ;
#76892 = CARTESIAN_POINT ( 'NONE',  ( 22.02124265030973760, 5.356774720514425603, 19.55402280011862004 ) ) ;
#76893 = ORIENTED_EDGE ( 'NONE', *, *, #31061, .F. ) ;
#76894 = CARTESIAN_POINT ( 'NONE',  ( 14.74224262856723833, 17.19160420931263999, -1.500000000000002220 ) ) ;
#76895 = EDGE_CURVE ( 'NONE', #29229, #74171, #71717, .T. ) ;
#76896 = EDGE_CURVE ( 'NONE', #79893, #3121, #50737, .T. ) ;
#76897 = ADVANCED_FACE ( 'NONE', ( #92909 ), #79695, .F. ) ;
#76899 = ORIENTED_EDGE ( 'NONE', *, *, #44272, .F. ) ;
#76898 = CARTESIAN_POINT ( 'NONE',  ( -92.52287095715006160, -24.65952944569304606, 1.056160979905700570 ) ) ;
#76900 = ORIENTED_EDGE ( 'NONE', *, *, #31509, .T. ) ;
#76901 = EDGE_CURVE ( 'NONE', #20703, #91990, #23386, .T. ) ;
#76902 = AXIS2_PLACEMENT_3D ( 'NONE', #61616, #87429, #57506 ) ;
#76903 = DIRECTION ( 'NONE',  ( 7.904402583950632871E-14, 0.000000000000000000, -1.000000000000000000 ) ) ;
#76904 = B_SPLINE_CURVE_WITH_KNOTS ( 'NONE', 3,
 ( #57093, #48970, #8896, #3312, #55084, #32729 ),
 .UNSPECIFIED., .F., .F.,
 ( 4, 2, 4 ),
 ( 0.000000000000000000, 0.001380901958385389412, 0.002761803916770778824 ),
 .UNSPECIFIED. ) ;
#76905 = B_SPLINE_CURVE_WITH_KNOTS ( 'NONE', 3,
 ( #43462, #57690, #49580, #89131, #35839, #11997, #74396, #57203, #80513, #10498, #4400, #97239, #35348, #96735, #19604, #80011, #50565, #66810 ),
 .UNSPECIFIED., .F., .F.,
 ( 4, 2, 2, 2, 2, 2, 2, 2, 4 ),
 ( 0.000000000000000000, 0.0002684257652534861004, 0.0005368515305069722007, 0.0008052772957604583011, 0.001073703061013944401, 0.001342128826267430502, 0.001610554591520916602, 0.001878980356774402703, 0.002147406122027888803 ),
 .UNSPECIFIED. ) ;
#76906 = CARTESIAN_POINT ( 'NONE',  ( -13.04681709000290013, -15.30929823114697541, 11.49999999999998934 ) ) ;
#76907 = B_SPLINE_SURFACE_WITH_KNOTS ( 'NONE', 3, 3, ( 
 ( #19600, #56699, #81014, #87630 ),
 ( #18114, #80007, #10495, #41968 ),
 ( #41455, #72413, #33836, #42470 ),
 ( #64824, #88632, #18601, #49577 ),
 ( #96243, #26727, #57687, #19101 ),
 ( #73409, #3903, #65811, #96731 ),
 ( #5877, #98720, #29715, #36838 ) ),
 .UNSPECIFIED., .F., .F., .F.,
 ( 4, 3, 4 ),
 ( 4, 4 ),
 ( 0.7945040050992234759, 0.8970133687736496775, 0.9995227324480758790 ),
 ( 0.2595599550269429012, 0.2606925096813342280 ),
 .UNSPECIFIED. ) ;
#76908 = CARTESIAN_POINT ( 'NONE',  ( -88.58953762381671027, -23.48783264082479150, -1.443836473390063935 ) ) ;
#76909 = VERTEX_POINT ( 'NONE', #569 ) ;
#76910 = FACE_OUTER_BOUND ( 'NONE', #65180, .T. ) ;
#76911 = CARTESIAN_POINT ( 'NONE',  ( 16.92800457317958518, -14.60656088873787262, -1.500000000000002220 ) ) ;
#76912 = EDGE_CURVE ( 'NONE', #8243, #36724, #40925, .T. ) ;
#76913 = EDGE_CURVE ( 'NONE', #20097, #25992, #14403, .T. ) ;
#76914 = VERTEX_POINT ( 'NONE', #26916 ) ;
#76915 = ORIENTED_EDGE ( 'NONE', *, *, #10129, .T. ) ;
#76916 = CARTESIAN_POINT ( 'NONE',  ( -101.3540785649959304, -25.16257400088798235, 6.680569373907164099 ) ) ;
#76917 = PLANE ( 'NONE',  #26458 ) ;
#76918 = CARTESIAN_POINT ( 'NONE',  ( 8.160000000000000142, 8.793627758918228565, -2.994553991265763049 ) ) ;
#76919 = CARTESIAN_POINT ( 'NONE',  ( -68.52287095715006160, -24.66019654487199730, 8.947790411086124607 ) ) ;
#76920 = DIRECTION ( 'NONE',  ( -1.000000000000000000, 0.000000000000000000, 0.000000000000000000 ) ) ;
#76921 = CARTESIAN_POINT ( 'NONE',  ( 12.76379665850700640, 14.79237594083867080, 11.49999999999998934 ) ) ;
#76922 = CARTESIAN_POINT ( 'NONE',  ( -33.55620429048341435, -24.64898659630528144, 1.056161002820815931 ) ) ;
#76923 = CARTESIAN_POINT ( 'NONE',  ( -2.231587876719630437, -21.34735720706076378, -1.500000000000002220 ) ) ;
#76924 = DIRECTION ( 'NONE',  ( 0.4009304992412300872, 0.000000000000000000, 0.9161084732596779245 ) ) ;
#76925 = DIRECTION ( 'NONE',  ( 0.000000000000000000, 0.000000000000000000, -1.000000000000000000 ) ) ;
#76926 = LINE ( 'NONE', #8435, #32827 ) ;
#76928 = VECTOR ( 'NONE', #30293, 1000.000000000000114 ) ;
#76927 = CARTESIAN_POINT ( 'NONE',  ( 17.70901601935662839, 14.43836031950349152, -1.500000000000002220 ) ) ;
#76929 = EDGE_CURVE ( 'NONE', #24851, #1763, #63617, .T. ) ;
#76930 = EDGE_CURVE ( 'NONE', #27962, #17829, #26419, .T. ) ;
#76931 = PERSON_AND_ORGANIZATION ( #70597, #27821 ) ;
#76932 = CARTESIAN_POINT ( 'NONE',  ( -96.55782220809594207, -23.73791477778912196, 11.05961554403170410 ) ) ;
#76933 = CARTESIAN_POINT ( 'NONE',  ( -2.794793911895765870, -5.876774720514418071, 20.33046051580616265 ) ) ;
#76934 = CARTESIAN_POINT ( 'NONE',  ( 8.743921044546416610, -18.04861246754477477, 11.49999999999999645 ) ) ;
#76935 = CARTESIAN_POINT ( 'NONE',  ( -80.06557898417501917, -25.26612378837472761, 4.529242823862608347 ) ) ;
#76936 = DIRECTION ( 'NONE',  ( 0.000000000000000000, -3.056206645085457922E-15, -1.000000000000000000 ) ) ;
#76937 = CARTESIAN_POINT ( 'NONE',  ( 4.782775879418006859, -5.876774720514407413, 18.83817099474236656 ) ) ;
#76938 = PLANE ( 'NONE',  #27803 ) ;
#76939 = ORIENTED_EDGE ( 'NONE', *, *, #9336, .F. ) ;
#76940 = CARTESIAN_POINT ( 'NONE',  ( -109.5228709571500616, -24.33832256527048088, 0.1851278514138657294 ) ) ;
#76941 = DIRECTION ( 'NONE',  ( 8.503546450866693616E-15, 0.000000000000000000, 1.000000000000000000 ) ) ;
#76942 = EDGE_CURVE ( 'NONE', #92857, #48435, #62004, .T. ) ;
#76943 = AXIS2_PLACEMENT_3D ( 'NONE', #73537, #28858, #19728 ) ;
#76944 = CARTESIAN_POINT ( 'NONE',  ( 6.244050601037331560, 20.82503750550150912, -1.500000000000002220 ) ) ;
#76945 = CARTESIAN_POINT ( 'NONE',  ( -117.6228709571500559, -23.48783264082479505, -1.443836473390058384 ) ) ;
#76946 = CARTESIAN_POINT ( 'NONE',  ( 18.24213732562919787, -7.162457363581539838, -1.500000000000002220 ) ) ;
#76947 = CARTESIAN_POINT ( 'NONE',  ( -29.62287095715004881, -29.50248528299834305, 1.056150588822498460 ) ) ;
#76948 = ADVANCED_FACE ( 'NONE', ( #20280 ), #57886, .T. ) ;
#76949 = B_SPLINE_CURVE_WITH_KNOTS ( 'NONE', 3,
 ( #2741, #35184, #49924, #81353 ),
 .UNSPECIFIED., .F., .F.,
 ( 4, 4 ),
 ( 0.3189916387590558400, 0.3199923857998208110 ),
 .UNSPECIFIED. ) ;
#76950 = EDGE_CURVE ( 'NONE', #32855, #40153, #82191, .T. ) ;
#76951 = FACE_OUTER_BOUND ( 'NONE', #87228, .T. ) ;
#76952 = DATE_AND_TIME ( #46031, #97710 ) ;
#76953 = CARTESIAN_POINT ( 'NONE',  ( -91.58852088267255454, -24.35071581493543391, 9.817618358456023486 ) ) ;
#76954 = CARTESIAN_POINT ( 'NONE',  ( 2.787364042957740651, -5.876774720514424288, 21.14548745790758488 ) ) ;
#76955 = CARTESIAN_POINT ( 'NONE',  ( 19.18951349294833264, 7.196795126939715459, 11.49999999999999645 ) ) ;
#76956 = CARTESIAN_POINT ( 'NONE',  ( -39.11368603858827697, -25.31200071491427650, 4.685369829760536398 ) ) ;
#76957 = CARTESIAN_POINT ( 'NONE',  ( -120.5579443694568909, -23.48783264082477018, -1.443836473390085695 ) ) ;
#76958 = EDGE_CURVE ( 'NONE', #19118, #28096, #73724, .T. ) ;
#76959 = ORIENTED_EDGE ( 'NONE', *, *, #11779, .F. ) ;
#76960 =( NAMED_UNIT ( * ) SI_UNIT ( $, .STERADIAN. ) SOLID_ANGLE_UNIT ( ) );
#76961 = CARTESIAN_POINT ( 'NONE',  ( -109.5228709571500616, -29.50248528299804818, 1.056150453629043584 ) ) ;
#76962 = CARTESIAN_POINT ( 'NONE',  ( -13.57581083383196940, -5.876774720514426953, 20.21213203435597094 ) ) ;
#76963 = CARTESIAN_POINT ( 'NONE',  ( -125.5547320878391275, -24.63419186844610920, 9.035850630976920428 ) ) ;
#76964 = CARTESIAN_POINT ( 'NONE',  ( 29.64064043116815128, -5.965225279485572685, 28.71191112024341408 ) ) ;
#76965 = CARTESIAN_POINT ( 'NONE',  ( -110.5228709571500616, -23.48786465467242479, 11.44779295918253936 ) ) ;
#76966 = PLANE ( 'NONE',  #30162 ) ;
#76967 = CARTESIAN_POINT ( 'NONE',  ( -18.41700849636773540, 13.91914711744011157, 11.49999999999999645 ) ) ;
#76968 = CARTESIAN_POINT ( 'NONE',  ( -16.48365427610503886, -15.78576583860491489, -1.500000000000002220 ) ) ;
#76969 = DIRECTION ( 'NONE',  ( -7.150924204855701834E-40, -2.173523156925979975E-06, 0.9999999999976378895 ) ) ;
#76970 = CARTESIAN_POINT ( 'NONE',  ( 0.3910256410256383042, -6.376774720514408301, 19.19230769230768985 ) ) ;
#76971 = CARTESIAN_POINT ( 'NONE',  ( -85.52287095715004739, -24.99156044556120193, 7.747789690856173195 ) ) ;
#76972 = AXIS2_PLACEMENT_3D ( 'NONE', #19927, #18930, #80843 ) ;
#76973 = CARTESIAN_POINT ( 'NONE',  ( -12.73782554413503654, -18.45060914899308457, 11.49999999999999645 ) ) ;
#76974 = VERTEX_POINT ( 'NONE', #43641 ) ;
#76975 = CARTESIAN_POINT ( 'NONE',  ( -11.64875734969026233, -5.965225279485572685, 31.02402280011862246 ) ) ;
#76976 = CARTESIAN_POINT ( 'NONE',  ( -43.66333338684359688, -23.48783264082478084, -1.443836473390076369 ) ) ;
#76977 = CARTESIAN_POINT ( 'NONE',  ( -19.93956527825925917, 9.129326121205059152, -1.500000000000002220 ) ) ;
#76978 = LINE ( 'NONE', #61289, #65674 ) ;
#76979 = DIRECTION ( 'NONE',  ( -3.773278334453079618E-23, 0.9999999999976377785, 2.173523156925978705E-06 ) ) ;
#76980 = CARTESIAN_POINT ( 'NONE',  ( -104.5480626255145040, -24.65952944569304606, 1.056160979905702346 ) ) ;
#76981 = LINE ( 'NONE', #100306, #41134 ) ;
#76982 = CARTESIAN_POINT ( 'NONE',  ( -103.5228709571500758, -24.65952944569304606, 1.056160979905702346 ) ) ;
#76983 = ORIENTED_EDGE ( 'NONE', *, *, #8238, .T. ) ;
#76984 = CARTESIAN_POINT ( 'NONE',  ( -20.02755620033356010, -4.236777897013602079, -1.500000000000002220 ) ) ;
#76985 = EDGE_LOOP ( 'NONE', ( #14839, #7233, #98763, #89657 ) ) ;
#76986 = B_SPLINE_CURVE_WITH_KNOTS ( 'NONE', 3,
 ( #59920, #81242, #80750, #19338, #42210, #59405, #35076, #19825, #35578, #66554, #97947, #4627 ),
 .UNSPECIFIED., .F., .F.,
 ( 4, 2, 2, 2, 2, 4 ),
 ( 0.000000000000000000, 0.0001492647388655131511, 0.0002985294777310263021, 0.0005970589554620495685, 0.0008955884331930726722, 0.001194117910924095884 ),
 .UNSPECIFIED. ) ;
#76987 = VERTEX_POINT ( 'NONE', #35035 ) ;
#76988 = ORIENTED_EDGE ( 'NONE', *, *, #30426, .T. ) ;
#76989 = ORIENTED_EDGE ( 'NONE', *, *, #634, .F. ) ;
#76990 = CARTESIAN_POINT ( 'NONE',  ( -22.28253579152010033, 6.022996098971622914, 11.49999999999998934 ) ) ;
#76991 = CARTESIAN_POINT ( 'NONE',  ( -82.52287095715006160, -24.64898659630367916, 1.056161002820826145 ) ) ;
#76992 = CARTESIAN_POINT ( 'NONE',  ( -14.66855384320708033, -14.05595220846724835, -1.500000000000002220 ) ) ;
#76993 = ORIENTED_EDGE ( 'NONE', *, *, #45664, .F. ) ;
#76994 = CARTESIAN_POINT ( 'NONE',  ( -26.07725539581784346, -24.96266517532310303, 5.848370260082334404 ) ) ;
#76995 = CARTESIAN_POINT ( 'NONE',  ( -83.52287095715006160, -29.50250786944525672, 11.44777988621623521 ) ) ;
#76996 = CARTESIAN_POINT ( 'NONE',  ( -101.2401810617817262, -25.17942323519604386, 6.818125126578213013 ) ) ;
#76997 = DIRECTION ( 'NONE',  ( 0.000000000000000000, -2.173523156925980399E-06, 0.9999999999976378895 ) ) ;
#76999 = ORIENTED_EDGE ( 'NONE', *, *, #23879, .F. ) ;
#76998 = CARTESIAN_POINT ( 'NONE',  ( -19.34459864454321831, 9.218434461607088792, 11.49999999999999645 ) ) ;
#77000 = CARTESIAN_POINT ( 'NONE',  ( 33.12653832968937451, -0.3587747205144265483, -7.315055336576590683 ) ) ;
#77001 = CARTESIAN_POINT ( 'NONE',  ( -61.54846442012016894, -24.15620529776627734, 10.23563542870660825 ) ) ;
#77002 = EDGE_LOOP ( 'NONE', ( #53234, #38636, #49107, #70273 ) ) ;
#77003 = CARTESIAN_POINT ( 'NONE',  ( 20.68991284688621946, 0.5745778482356619365, 11.49999999999998934 ) ) ;
#77004 = VECTOR ( 'NONE', #53173, 1000.000000000000000 ) ;
#77005 = VERTEX_POINT ( 'NONE', #74579 ) ;
#77007 = EDGE_LOOP ( 'NONE', ( #92134, #77733, #18980, #52891 ) ) ;
#77006 = CARTESIAN_POINT ( 'NONE',  ( -123.6228709571500417, -23.73907113216991149, -1.053371485793226592 ) ) ;
#77008 = EDGE_CURVE ( 'NONE', #84073, #71576, #58377, .T. ) ;
#77009 = LINE ( 'NONE', #1917, #35727 ) ;
#77010 = ORIENTED_EDGE ( 'NONE', *, *, #65787, .F. ) ;
#77011 = ORIENTED_EDGE ( 'NONE', *, *, #38222, .T. ) ;
#77012 = EDGE_CURVE ( 'NONE', #71187, #69320, #45872, .T. ) ;
#77013 = CARTESIAN_POINT ( 'NONE',  ( -55.52287095715004739, -24.14406661686757261, 10.28769366194082302 ) ) ;
#77014 = DIRECTION ( 'NONE',  ( 0.000000000000000000, 0.9999999999976377785, 2.173523156925979128E-06 ) ) ;
#77015 = CARTESIAN_POINT ( 'NONE',  ( -65.57704652348438401, -25.00158670708910691, 2.256160236439222366 ) ) ;
#77016 = CARTESIAN_POINT ( 'NONE',  ( 15.04091035147580335, -15.99806323810862274, 11.49999999999999645 ) ) ;
#77017 = VECTOR ( 'NONE', #83769, 1000.000000000000000 ) ;
#77018 = EDGE_CURVE ( 'NONE', #20503, #15484, #76043, .T. ) ;
#77019 = CARTESIAN_POINT ( 'NONE',  ( -89.51458554710613669, -23.96169478059713498, 10.65365249895717703 ) ) ;
#77020 = CARTESIAN_POINT ( 'NONE',  ( -3.649967738973055376, -22.27025559232234642, 11.49999999999998934 ) ) ;
#77021 = EDGE_CURVE ( 'NONE', #41820, #64103, #41654, .T. ) ;
#77022 = AXIS2_PLACEMENT_3D ( 'NONE', #17474, #84983, #7355 ) ;
#77023 = CARTESIAN_POINT ( 'NONE',  ( -20.92093621315066443, -1.481899440790641842, 11.49999999999998934 ) ) ;
#77024 = CARTESIAN_POINT ( 'NONE',  ( -111.5562042904833930, -24.64898659630529565, 1.056161002820831918 ) ) ;
#77025 = EDGE_CURVE ( 'NONE', #12105, #42138, #11677, .T. ) ;
#77026 = CARTESIAN_POINT ( 'NONE',  ( 6.509931258083027750, -6.376774720514417183, 20.09204137875607188 ) ) ;
#77027 = ORIENTED_EDGE ( 'NONE', *, *, #10382, .F. ) ;
#77028 = ORIENTED_EDGE ( 'NONE', *, *, #81807, .T. ) ;
#77029 = EDGE_CURVE ( 'NONE', #24683, #88649, #34033, .T. ) ;
#77030 = VERTEX_POINT ( 'NONE', #42659 ) ;
#77031 = CARTESIAN_POINT ( 'NONE',  ( -59.62287095715004170, -24.50321055353805377, 9.387540953477532923 ) ) ;
#77032 = CARTESIAN_POINT ( 'NONE',  ( 18.54456287915894563, -10.88813254144886322, -1.500000000000002220 ) ) ;
#77033 = CARTESIAN_POINT ( 'NONE',  ( 8.971512145086503409, -1.000000000000001110, -3.746884140868835367 ) ) ;
#77034 = ORIENTED_EDGE ( 'NONE', *, *, #70573, .F. ) ;
#77035 = CARTESIAN_POINT ( 'NONE',  ( 1.943494986365726485, -21.02143711168614004, 11.49999999999998934 ) ) ;
#77036 = CARTESIAN_POINT ( 'NONE',  ( -24.90875734969025501, -5.965225279485572685, 26.43402280011862615 ) ) ;
#77037 = CARTESIAN_POINT ( 'NONE',  ( -61.66538019323460418, -25.14083923594472125, 2.947789366366679875 ) ) ;
#77038 = FACE_OUTER_BOUND ( 'NONE', #67047, .T. ) ;
#77039 = DIRECTION ( 'NONE',  ( -3.773278334453079030E-23, 0.9999999999976377785, 2.173523156925979128E-06 ) ) ;
#77040 = DIRECTION ( 'NONE',  ( -1.000000000000000000, -0.000000000000000000, -0.000000000000000000 ) ) ;
#77041 = CARTESIAN_POINT ( 'NONE',  ( -5.843409716339609261, -21.38298466452703650, -1.500000000000002220 ) ) ;
#77042 = CARTESIAN_POINT ( 'NONE',  ( -81.51308774969011495, -23.96169478059713143, 10.65365249895718591 ) ) ;
#77043 = EDGE_CURVE ( 'NONE', #89884, #49235, #19785, .T. ) ;
#77044 = ORIENTED_EDGE ( 'NONE', *, *, #83004, .F. ) ;
#77045 = CARTESIAN_POINT ( 'NONE',  ( -51.15602047325173629, -25.24860005136912733, 4.998863007599903874 ) ) ;
#77046 = CARTESIAN_POINT ( 'NONE',  ( -0.6703829557040269504, 4.102177322343282917, 3.549999999999996714 ) ) ;
#77047 = PLANE ( 'NONE',  #71206 ) ;
#77048 = FACE_OUTER_BOUND ( 'NONE', #88167, .T. ) ;
#77049 = ADVANCED_FACE ( 'NONE', ( #81703 ), #65009, .T. ) ;
#77050 = CARTESIAN_POINT ( 'NONE',  ( 8.422564666779264186, -17.53554878399664574, -1.500000000000002220 ) ) ;
#77051 = VECTOR ( 'NONE', #66779, 1000.000000000000114 ) ;
#77052 = CARTESIAN_POINT ( 'NONE',  ( -21.27170209485220198, -2.091907790468015005, 11.49999999999998934 ) ) ;
#77053 = CARTESIAN_POINT ( 'NONE',  ( -62.58763761694054040, -24.34968618360933945, 0.1864209137778799485 ) ) ;
#77054 = CARTESIAN_POINT ( 'NONE',  ( 13.57581083383197296, -6.376774720514426953, 19.78786796564403616 ) ) ;
#77055 = CARTESIAN_POINT ( 'NONE',  ( -110.9353407762807393, -25.05712135967895549, 7.447789548357303779 ) ) ;
#77056 = CARTESIAN_POINT ( 'NONE',  ( -100.4839344043725333, -25.27359974982199020, 3.295731817984544509 ) ) ;
#77057 = CARTESIAN_POINT ( 'NONE',  ( -10.65177407370799045, -20.06881281718593613, -1.500000000000002220 ) ) ;
#77058 = CARTESIAN_POINT ( 'NONE',  ( -98.55771462834329100, -23.73766607897669800, -1.055555164236454013 ) ) ;
#77059 = LINE ( 'NONE', #39008, #57329 ) ;
#77060 = CARTESIAN_POINT ( 'NONE',  ( -19.19514693104756375, 4.742496307885142315, 11.49999999999999645 ) ) ;
#77061 = CARTESIAN_POINT ( 'NONE',  ( -115.6228709571500559, -23.47596703998600631, 11.44779298504227860 ) ) ;
#77062 = ORIENTED_EDGE ( 'NONE', *, *, #51370, .F. ) ;
#77063 = CARTESIAN_POINT ( 'NONE',  ( -60.52287095715006160, -25.00158670708908915, 2.256160236439166411 ) ) ;
#77064 = CARTESIAN_POINT ( 'NONE',  ( -80.52287095715006160, -23.84081130425359163, 10.88220057483156644 ) ) ;
#77065 = CARTESIAN_POINT ( 'NONE',  ( -68.52287095715001897, -24.34917612406836795, 0.1852690917426542405 ) ) ;
#77066 = CARTESIAN_POINT ( 'NONE',  ( 21.13687465659472409, 4.681744431724916389, -1.500000000000002220 ) ) ;
#77067 = CARTESIAN_POINT ( 'NONE',  ( 6.650000000000004796, 0.000000000000000000, 18.35000000000000142 ) ) ;
#77068 = CARTESIAN_POINT ( 'NONE',  ( -19.08929872761019908, -3.557156390981079053, -1.500000000000002220 ) ) ;
#77069 = CARTESIAN_POINT ( 'NONE',  ( -80.52287095715006160, -23.85229601348996908, 10.88205029486208986 ) ) ;
#77070 = CARTESIAN_POINT ( 'NONE',  ( -8.160000000000000142, -9.652339641703484574, -1.621096496867199033 ) ) ;
#77071 = EDGE_CURVE ( 'NONE', #94542, #16286, #66377, .T. ) ;
#77072 = CARTESIAN_POINT ( 'NONE',  ( 9.833179757865110560, 17.22857952739193266, -1.500000000000002220 ) ) ;
#77073 = EDGE_LOOP ( 'NONE', ( #83525, #50320 ) ) ;
#77074 = CARTESIAN_POINT ( 'NONE',  ( 0.7445296356392017145, -20.29553345556499622, 11.49999999999999645 ) ) ;
#77075 = CARTESIAN_POINT ( 'NONE',  ( -80.53951533976572819, -24.83618233451450408, 1.606449574219532384 ) ) ;
#77076 = EDGE_CURVE ( 'NONE', #55189, #46432, #39563, .T. ) ;
#77077 = AXIS2_PLACEMENT_3D ( 'NONE', #33822, #65307, #11480 ) ;
#77078 = CARTESIAN_POINT ( 'NONE',  ( 33.47959399259596580, -3.475369878553063341, -12.33463419434873032 ) ) ;
#77079 = B_SPLINE_CURVE_WITH_KNOTS ( 'NONE', 3,
 ( #86718, #92825, #31941, #23307, #85724, #17208, #54292, #39048 ),
 .UNSPECIFIED., .F., .F.,
 ( 4, 2, 2, 4 ),
 ( 6.384118678605199737E-06, 0.002007151183507247146, 0.003007534715921569932, 0.004007918248335893587 ),
 .UNSPECIFIED. ) ;
#77080 = ORIENTED_EDGE ( 'NONE', *, *, #38645, .T. ) ;
#77081 = CARTESIAN_POINT ( 'NONE',  ( -0.08079981110223319329, -22.00398294951504496, 0.01136689895587368430 ) ) ;
#77082 = CARTESIAN_POINT ( 'NONE',  ( -92.52287095715009002, -23.72747288104470087, -1.053458166803225460 ) ) ;
#77083 = LINE ( 'NONE', #30420, #72699 ) ;
#77084 = CIRCLE ( 'NONE', #69050, 18.50000000000000355 ) ;
#77085 = CARTESIAN_POINT ( 'NONE',  ( -40.62644180606930888, -24.92592662359561118, 8.075495903017996469 ) ) ;
#77086 = VECTOR ( 'NONE', #15414, 1000.000000000000000 ) ;
#77087 = CARTESIAN_POINT ( 'NONE',  ( -0.7827064370038755436, -5.876774720514410077, 19.55912026249540148 ) ) ;
#77088 = CARTESIAN_POINT ( 'NONE',  ( -19.91332876899582160, 2.521106391696132931, 11.49999999999998934 ) ) ;
#77089 = AXIS2_PLACEMENT_3D ( 'NONE', #72213, #16910, #79805 ) ;
#77090 = CARTESIAN_POINT ( 'NONE',  ( -85.52287095715013265, -24.91544648472627088, 1.928969306349433310 ) ) ;
#77091 = VERTEX_POINT ( 'NONE', #90308 ) ;
#77092 = CARTESIAN_POINT ( 'NONE',  ( -130.5728709571500588, -23.56000036390797092, -1.497999999999531040 ) ) ;
#77093 = VECTOR ( 'NONE', #81755, 1000.000000000000000 ) ;
#77094 = CARTESIAN_POINT ( 'NONE',  ( -4.124250913864588419, 22.51598698906299845, 11.49999999999999645 ) ) ;
#77095 = CARTESIAN_POINT ( 'NONE',  ( -5.793434319722853054, -21.96748078227757617, -1.500000000000002220 ) ) ;
#77096 = VERTEX_POINT ( 'NONE', #76071 ) ;
#77097 = LINE ( 'NONE', #78588, #79391 ) ;
#77098 = CARTESIAN_POINT ( 'NONE',  ( -57.62287095715004881, -29.50248528299804818, 1.056150453629034924 ) ) ;
#77099 = CARTESIAN_POINT ( 'NONE',  ( 14.76093561896379214, -3.316774720514426456, -26.55548769130089681 ) ) ;
#77100 = CARTESIAN_POINT ( 'NONE',  ( -73.58953762381672448, -23.48783264082478084, -1.443836473390067487 ) ) ;
#77101 = DIRECTION ( 'NONE',  ( 0.000000000000000000, 1.000000000000000000, -0.000000000000000000 ) ) ;
#77102 = PLANE ( 'NONE',  #61518 ) ;
#77103 = EDGE_LOOP ( 'NONE', ( #23125, #44222, #40315, #7272 ) ) ;
#77104 = CARTESIAN_POINT ( 'NONE',  ( -5.548086588741434788, -19.59138962566686004, -1.500000000000002220 ) ) ;
#77105 = ORIENTED_EDGE ( 'NONE', *, *, #27648, .T. ) ;
#77106 = CARTESIAN_POINT ( 'NONE',  ( 8.272623322502495213, 21.45567517505680044, -1.500000000000002220 ) ) ;
#77107 = CARTESIAN_POINT ( 'NONE',  ( -54.52206316579233203, -23.48786465467240703, 11.44779295918255180 ) ) ;
#77108 = ORIENTED_EDGE ( 'NONE', *, *, #40256, .F. ) ;
#77109 = CARTESIAN_POINT ( 'NONE',  ( -108.5535921372889163, -24.15620529776629510, 10.23563542870659404 ) ) ;
#77110 = CARTESIAN_POINT ( 'NONE',  ( 2.903846153846159517, -6.376774720514415407, 19.99999999999999289 ) ) ;
#77111 = CARTESIAN_POINT ( 'NONE',  ( -40.62287095715006302, -23.84047902841600930, -0.8780736468305813114 ) ) ;
#77113 = ORIENTED_EDGE ( 'NONE', *, *, #23179, .T. ) ;
#77112 = CARTESIAN_POINT ( 'NONE',  ( 6.411417644607832145, 20.24884965431308714, 11.49999999999999645 ) ) ;
#77114 = EDGE_LOOP ( 'NONE', ( #9866, #53449, #95509, #92838 ) ) ;
#77115 = CARTESIAN_POINT ( 'NONE',  ( 4.265775719338400052, 21.77767432286298543, 11.49999999999998934 ) ) ;
#77116 = B_SPLINE_CURVE_WITH_KNOTS ( 'NONE', 3,
 ( #80993, #74860, #51551, #73388 ),
 .UNSPECIFIED., .F., .F.,
 ( 4, 4 ),
 ( 0.000000000000000000, 9.999999999998206125E-05 ),
 .UNSPECIFIED. ) ;
#77117 = CARTESIAN_POINT ( 'NONE',  ( -20.24099117049231467, 3.958469829285517161, 11.49999999999998934 ) ) ;
#77118 = ORIENTED_EDGE ( 'NONE', *, *, #83283, .F. ) ;
#77119 = ORIENTED_EDGE ( 'NONE', *, *, #77466, .T. ) ;
#77120 = EDGE_CURVE ( 'NONE', #21700, #89515, #42107, .T. ) ;
#77121 = CARTESIAN_POINT ( 'NONE',  ( -108.9610644980590450, -25.31627158989577353, 4.357072244912905568 ) ) ;
#77122 = CARTESIAN_POINT ( 'NONE',  ( -7.347880794884120722E-16, -4.056774720514426669, -6.000000000000000888 ) ) ;
#77123 = VERTEX_POINT ( 'NONE', #38017 ) ;
#77124 = EDGE_CURVE ( 'NONE', #86083, #5378, #68475, .T. ) ;
#77125 = CARTESIAN_POINT ( 'NONE',  ( -91.54879471971332805, -24.34968618360934300, 0.1864209137778843617 ) ) ;
#77126 = ORIENTED_EDGE ( 'NONE', *, *, #52858, .T. ) ;
#77127 = CARTESIAN_POINT ( 'NONE',  ( -121.5895376238167387, -23.47596703998600631, 11.44779298504227683 ) ) ;
#77128 = DIRECTION ( 'NONE',  ( 0.000000000000000000, 0.000000000000000000, 1.000000000000000000 ) ) ;
#77129 = CARTESIAN_POINT ( 'NONE',  ( 15.20108283357335921, -14.20388156210760577, -1.500000000000002220 ) ) ;
#77130 = CARTESIAN_POINT ( 'NONE',  ( -21.42251255223715134, 3.917230396363152067, 11.49999999999999645 ) ) ;
#77131 = EDGE_CURVE ( 'NONE', #71104, #37448, #57172, .T. ) ;
#77132 = CARTESIAN_POINT ( 'NONE',  ( 25.08009522652915635, -5.127174019380943193, -9.013305873660419465 ) ) ;
#77133 = CARTESIAN_POINT ( 'NONE',  ( -99.10821524085508827, -25.16307519314475982, 6.860273405324268658 ) ) ;
#77134 = CARTESIAN_POINT ( 'NONE',  ( -1.649324495273077451, -22.40575143947253167, 11.49999999999998934 ) ) ;
#77135 = EDGE_CURVE ( 'NONE', #1913, #16500, #28399, .T. ) ;
#77136 = VECTOR ( 'NONE', #80463, 1000.000000000000114 ) ;
#77137 = FACE_OUTER_BOUND ( 'NONE', #45431, .T. ) ;
#77138 = EDGE_LOOP ( 'NONE', ( #778, #25874, #8448, #67361 ) ) ;
#77139 = CARTESIAN_POINT ( 'NONE',  ( -50.52287095715008292, -24.92604778743017491, 8.074972756849357225 ) ) ;
#77140 = DIRECTION ( 'NONE',  ( -0.9701425001453318764, 0.2425356250363331356, 0.000000000000000000 ) ) ;
#77141 = EDGE_CURVE ( 'NONE', #98958, #56064, #15173, .T. ) ;
#77142 = EDGE_LOOP ( 'NONE', ( #69774, #8385, #6756, #2548 ) ) ;
#77143 = EDGE_CURVE ( 'NONE', #29097, #87273, #98907, .T. ) ;
#77144 = EDGE_LOOP ( 'NONE', ( #85136, #36919 ) ) ;
#77145 = EDGE_LOOP ( 'NONE', ( #39292, #95126, #80924 ) ) ;
#77146 = VECTOR ( 'NONE', #43442, 1000.000000000000114 ) ;
#77147 = CARTESIAN_POINT ( 'NONE',  ( -13.85510387911049079, -16.26762222697724880, -1.500000000000002220 ) ) ;
#77148 = EDGE_LOOP ( 'NONE', ( #78390, #66600, #91251, #48963 ) ) ;
#77149 = CARTESIAN_POINT ( 'NONE',  ( -5.295558097854481616, 20.35707381486366785, -1.500000000000002220 ) ) ;
#77150 = CARTESIAN_POINT ( 'NONE',  ( -30.44149352667901809, -24.26500045891999946, 0.04395666736089841320 ) ) ;
#77151 = LINE ( 'NONE', #24379, #98740 ) ;
#77152 = AXIS2_PLACEMENT_3D ( 'NONE', #44767, #84307, #75691 ) ;
#77153 = CARTESIAN_POINT ( 'NONE',  ( -37.62287095715005592, -29.50248528299804818, 1.056150453629031594 ) ) ;
#77154 = CARTESIAN_POINT ( 'NONE',  ( 4.628415685485613551, -21.52068878818806752, -1.500000000000002220 ) ) ;
#77155 = CARTESIAN_POINT ( 'NONE',  ( 16.36243866176394945, 0.000000000000000000, 0.000000000000000000 ) ) ;
#77156 = VERTEX_POINT ( 'NONE', #45144 ) ;
#77157 = LINE ( 'NONE', #61960, #3287 ) ;
#77158 = VECTOR ( 'NONE', #96535, 1000.000000000000114 ) ;
#77159 = CARTESIAN_POINT ( 'NONE',  ( -107.5895376238167529, -23.47593901973091235, -1.443836447538999312 ) ) ;
#77160 = VECTOR ( 'NONE', #17583, 1000.000000000000114 ) ;
#77161 = CARTESIAN_POINT ( 'NONE',  ( 31.62500054620284473, -6.365374413700245704, 26.93529845007237711 ) ) ;
#77162 = LINE ( 'NONE', #7665, #45712 ) ;
#77163 = DIRECTION ( 'NONE',  ( 0.000000000000000000, 0.000000000000000000, -1.000000000000000000 ) ) ;
#77164 = CARTESIAN_POINT ( 'NONE',  ( 17.95810460983813783, 11.44545274529666479, 11.49999999999998934 ) ) ;
#77165 = DIRECTION ( 'NONE',  ( 1.420947339892994047E-14, 0.000000000000000000, -1.000000000000000000 ) ) ;
#77166 = CARTESIAN_POINT ( 'NONE',  ( -107.6297665980143137, -23.96169478059713853, 10.65365249895717348 ) ) ;
#77167 = LINE ( 'NONE', #15778, #84 ) ;
#77168 = DIRECTION ( 'NONE',  ( -0.9913618264504691080, 4.164321980682960499E-15, 0.1311553622875927805 ) ) ;
#77169 = CARTESIAN_POINT ( 'NONE',  ( 14.28312119630281174, -17.39864199977734671, -1.500000000000002220 ) ) ;
#77170 = CARTESIAN_POINT ( 'NONE',  ( -108.8785801883210951, -25.06174035403189038, 7.474877196992075312 ) ) ;
#77171 = VERTEX_POINT ( 'NONE', #59874 ) ;
#77172 = CARTESIAN_POINT ( 'NONE',  ( 30.53060340732035982, -1.477225279485574028, 19.84760796525321780 ) ) ;
#77173 = CARTESIAN_POINT ( 'NONE',  ( 0.6594449095415070294, 19.62168050102039629, 11.49999999999999645 ) ) ;
#77174 = DIRECTION ( 'NONE',  ( 0.000000000000000000, -1.000000000000000000, 0.000000000000000000 ) ) ;
#77175 = CARTESIAN_POINT ( 'NONE',  ( -100.6228709571500701, -24.82576562982393042, 8.398263435472967942 ) ) ;
#77176 = ORIENTED_EDGE ( 'NONE', *, *, #1107, .F. ) ;
#77177 = CARTESIAN_POINT ( 'NONE',  ( -68.93918693012690824, -25.24795196732124936, 6.184868460502651821 ) ) ;
#77178 = DIRECTION ( 'NONE',  ( -3.773278334453079030E-23, 0.9999999999976377785, 2.173523156925979128E-06 ) ) ;
#77179 = CARTESIAN_POINT ( 'NONE',  ( -91.96414918007445749, -25.30572777988224331, 5.920366768842380445 ) ) ;
#77180 = AXIS2_PLACEMENT_3D ( 'NONE', #6896, #54576, #85512 ) ;
#77181 = CARTESIAN_POINT ( 'NONE',  ( 7.891737972721761807, -18.10977644326358771, -1.500000000000002220 ) ) ;
#77182 = VERTEX_POINT ( 'NONE', #59365 ) ;
#77183 = CARTESIAN_POINT ( 'NONE',  ( -120.5228709571501184, -24.92604778743018556, 8.074972756849353672 ) ) ;
#77184 = CARTESIAN_POINT ( 'NONE',  ( -70.62287095715005592, -25.00158670708909270, 2.256160236439166855 ) ) ;
#77185 = EDGE_CURVE ( 'NONE', #26377, #52082, #51756, .T. ) ;
#77186 = APPROVAL_ROLE ( '' ) ;
#77187 = EDGE_CURVE ( 'NONE', #28708, #23124, #63864, .T. ) ;
#77188 = ORIENTED_EDGE ( 'NONE', *, *, #65059, .T. ) ;
#77189 = CARTESIAN_POINT ( 'NONE',  ( -109.6228709571500417, -23.48786465467242124, 11.44779295918253936 ) ) ;
#77190 = DIRECTION ( 'NONE',  ( 0.000000000000000000, 0.000000000000000000, 1.000000000000000000 ) ) ;
#77191 = CARTESIAN_POINT ( 'NONE',  ( -90.52287095715006160, -23.48786465467241769, 11.44779295918254292 ) ) ;
#77192 = CARTESIAN_POINT ( 'NONE',  ( -99.65618967412262919, -25.03145138608062226, 7.377943801491970710 ) ) ;
#77193 = CARTESIAN_POINT ( 'NONE',  ( -1.304987980769231948, -5.876774720514413630, 19.76512419871795245 ) ) ;
#77194 = B_SPLINE_CURVE_WITH_KNOTS ( 'NONE', 3,
 ( #65422, #49188, #88236, #50667, #27328, #11592 ),
 .UNSPECIFIED., .F., .F.,
 ( 4, 2, 4 ),
 ( 6.384118695050191095E-06, 0.001386860460836595839, 0.002767336802978141459 ),
 .UNSPECIFIED. ) ;
#77195 = CARTESIAN_POINT ( 'NONE',  ( -56.52287095715006870, -24.65952944569304606, 1.056160979905695463 ) ) ;
#77196 = CARTESIAN_POINT ( 'NONE',  ( 19.86680303116296287, 2.261939200664708327, 11.49999999999998934 ) ) ;
#77197 = CARTESIAN_POINT ( 'NONE',  ( -127.6228709571500559, -24.50216790748099882, 0.6166512839513782485 ) ) ;
#77198 = CARTESIAN_POINT ( 'NONE',  ( -51.37986311123607663, -25.31231099970419862, 4.713062901810517680 ) ) ;
#77199 = ORIENTED_EDGE ( 'NONE', *, *, #23551, .T. ) ;
#77200 = AXIS2_PLACEMENT_3D ( 'NONE', #12181, #81709, #4594 ) ;
#77201 = CARTESIAN_POINT ( 'NONE',  ( 14.98985047787450320, 3.577630190450212577, -26.76169638709854226 ) ) ;
#77202 = CARTESIAN_POINT ( 'NONE',  ( -73.62287095715007013, -23.47596703998600276, 11.44779298504227860 ) ) ;
#77203 = CARTESIAN_POINT ( 'NONE',  ( -35.57451790842697648, -23.48783264082477729, -1.443836473390077479 ) ) ;
#77204 = CARTESIAN_POINT ( 'NONE',  ( -28.62287095715005947, -24.36053554431182988, 9.387565063642748342 ) ) ;
#77205 = B_SPLINE_CURVE_WITH_KNOTS ( 'NONE', 3,
 ( #1678, #32617, #69178, #30612, #61587, #92507, #22978, #33622, #64604, #26515, #57479, #4177, #11280, #34129, #79284, #40732, #9778, #56976, #10787, #3189, #50354, #71691 ),
 .UNSPECIFIED., .F., .F.,
 ( 4, 2, 2, 2, 2, 2, 2, 2, 2, 2, 4 ),
 ( 2.109901731184535120E-07, 0.0007177669497569155819, 0.001435322909340712699, 0.001794100889132610064, 0.002152878868924507430, 0.002870434828508297825, 0.003587990788092088653, 0.003946768767883982766, 0.004305546747675877313, 0.005023102707259665539, 0.005740658666843454633 ),
 .UNSPECIFIED. ) ;
#77206 = DIRECTION ( 'NONE',  ( -3.773278334444166432E-23, 1.000000000000000000, 0.000000000000000000 ) ) ;
#77207 = CARTESIAN_POINT ( 'NONE',  ( -83.51756576996206149, -23.73766607897670511, -1.055555164236456900 ) ) ;
#77208 = VECTOR ( 'NONE', #40144, 1000.000000000000114 ) ;
#77209 = CARTESIAN_POINT ( 'NONE',  ( -47.62287095715004881, -29.50248528299804818, 1.056150453629033370 ) ) ;
#77211 = VECTOR ( 'NONE', #10767, 1000.000000000000000 ) ;
#77210 = CARTESIAN_POINT ( 'NONE',  ( 5.402409956206937203, -5.876774720514423400, 21.18719775722114917 ) ) ;
#77212 = ORIENTED_EDGE ( 'NONE', *, *, #90788, .F. ) ;
#77213 = AXIS2_PLACEMENT_3D ( 'NONE', #92501, #31604, #77760 ) ;
#77214 = CARTESIAN_POINT ( 'NONE',  ( -15.67655817637044890, 12.86142704545212290, -1.500000000000002220 ) ) ;
#77215 = CARTESIAN_POINT ( 'NONE',  ( 10.34999999999998010, 22.00000000000000000, 2.100000000000000089 ) ) ;
#77216 = AXIS2_PLACEMENT_3D ( 'NONE', #65899, #89710, #2989 ) ;
#77217 = CARTESIAN_POINT ( 'NONE',  ( -90.52287095715004739, -24.14321612903117753, -0.2833117244520893530 ) ) ;
#77218 = ORIENTED_EDGE ( 'NONE', *, *, #86319, .F. ) ;
#77219 = FACE_OUTER_BOUND ( 'NONE', #45203, .T. ) ;
#77220 = CARTESIAN_POINT ( 'NONE',  ( 19.93115673323400117, -2.579441489355707606, -1.500000000000002220 ) ) ;
#77221 = CARTESIAN_POINT ( 'NONE',  ( 20.77832821955112408, -3.674247523096572099, 11.49999999999999645 ) ) ;
#77222 = CARTESIAN_POINT ( 'NONE',  ( -15.83042281971428977, -15.45127431894796466, -1.500000000000002220 ) ) ;
#77223 = CARTESIAN_POINT ( 'NONE',  ( -4.863915844574979275, 19.94883092034378791, -1.500000000000002220 ) ) ;
#77224 = DIRECTION ( 'NONE',  ( -3.469446951953611033E-15, -1.000000000000000000, 0.000000000000000000 ) ) ;
#77225 = CARTESIAN_POINT ( 'NONE',  ( -15.82668884360736961, 1.684774720514424118, 42.07822029717483758 ) ) ;
#77226 = EDGE_LOOP ( 'NONE', ( #17707, #50253, #24219, #64712 ) ) ;
#77227 = FACE_OUTER_BOUND ( 'NONE', #21332, .T. ) ;
#77228 = ORIENTED_EDGE ( 'NONE', *, *, #90946, .F. ) ;
#77229 = CARTESIAN_POINT ( 'NONE',  ( -6.636054160061366503, -6.376774720514411854, 19.15289935703627933 ) ) ;
#77230 = CARTESIAN_POINT ( 'NONE',  ( -85.62287095715007013, -24.92604778743018201, 8.074972756849359001 ) ) ;
#77231 = ORIENTED_EDGE ( 'NONE', *, *, #62439, .F. ) ;
#77233 = VERTEX_POINT ( 'NONE', #44140 ) ;
#77232 = EDGE_CURVE ( 'NONE', #66603, #81403, #50532, .T. ) ;
#77234 = EDGE_LOOP ( 'NONE', ( #890, #49369, #83141, #230 ) ) ;
#77235 = CARTESIAN_POINT ( 'NONE',  ( -19.69812919673063689, -5.965225279485592225, -22.00173861453435720 ) ) ;
#77236 = CARTESIAN_POINT ( 'NONE',  ( -63.62287095715004881, -24.65952944569303895, 1.056160979905696129 ) ) ;
#77237 = CARTESIAN_POINT ( 'NONE',  ( -68.49730927663665625, -24.51419770103157347, 9.386484678747180510 ) ) ;
#77238 = CARTESIAN_POINT ( 'NONE',  ( -16.38011734009650411, 12.53836025512309149, -1.500000000000002220 ) ) ;
#77239 = CARTESIAN_POINT ( 'NONE',  ( -21.09935167195790839, -4.734744157926700225, 11.49999999999999645 ) ) ;
#77240 = ORIENTED_EDGE ( 'NONE', *, *, #27811, .T. ) ;
#77241 = ADVANCED_FACE ( 'NONE', ( #99892 ), #100124, .T. ) ;
#77242 = B_SPLINE_CURVE_WITH_KNOTS ( 'NONE', 3,
 ( #16963, #40311, #98323, #28830, #39302, #13590 ),
 .UNSPECIFIED., .F., .F.,
 ( 4, 2, 4 ),
 ( 2.661873927568507014E-05, 0.002253574034153483369, 0.004480529329031281843 ),
 .UNSPECIFIED. ) ;
#77243 = PLANE ( 'NONE',  #30439 ) ;
#77244 = CIRCLE ( 'NONE', #38448, 11.85241003308275864 ) ;
#77245 = CARTESIAN_POINT ( 'NONE',  ( -57.62287095715004881, -23.47596703998600276, 11.44779298504227683 ) ) ;
#77246 = CARTESIAN_POINT ( 'NONE',  ( -16.90645664988545249, 14.66980924573920397, 11.49999999999998934 ) ) ;
#77247 = EDGE_CURVE ( 'NONE', #37557, #24356, #26272, .T. ) ;
#77248 = CARTESIAN_POINT ( 'NONE',  ( -47.54065078942323197, -24.35071581493542325, 9.817618358456030592 ) ) ;
#77249 = DIRECTION ( 'NONE',  ( -0.000000000000000000, -1.000000000000000000, -0.000000000000000000 ) ) ;
#77250 = ORIENTED_EDGE ( 'NONE', *, *, #3009, .T. ) ;
#77251 = CARTESIAN_POINT ( 'NONE',  ( -58.62287095715006302, -24.65952944569304250, 1.056160979905695463 ) ) ;
#77252 = CARTESIAN_POINT ( 'NONE',  ( -49.54102043467515415, -24.35071581493542325, 9.817618358456035921 ) ) ;
#77253 = EDGE_CURVE ( 'NONE', #6116, #5085, #16678, .T. ) ;
#77254 = CARTESIAN_POINT ( 'NONE',  ( -62.62287095715004881, -29.50248528299804818, 1.056150453629034924 ) ) ;
#77255 = CIRCLE ( 'NONE', #33537, 3.549999999999999378 ) ;
#77256 = CARTESIAN_POINT ( 'NONE',  ( -20.67734376658059858, -3.193854526364364954, -1.500000000000002220 ) ) ;
#77257 = EDGE_CURVE ( 'NONE', #24519, #99951, #62366, .T. ) ;
#77258 = VERTEX_POINT ( 'NONE', #17683 ) ;
#77259 = CARTESIAN_POINT ( 'NONE',  ( -86.58837541417300088, -24.34968618360933945, 0.1864209137778916059 ) ) ;
#77260 = VERTEX_POINT ( 'NONE', #23788 ) ;
#77261 = CARTESIAN_POINT ( 'NONE',  ( -109.5571236054648523, -23.73791477778912551, 11.05961554403169878 ) ) ;
#77262 = CARTESIAN_POINT ( 'NONE',  ( -17.67215177357914513, -11.65580189297658897, -1.500000000000002220 ) ) ;
#77263 = ORIENTED_EDGE ( 'NONE', *, *, #76680, .F. ) ;
#77264 = CARTESIAN_POINT ( 'NONE',  ( -50.52963312974734578, -24.83618233451449697, 1.606449574219540599 ) ) ;
#77265 = FACE_OUTER_BOUND ( 'NONE', #89826, .T. ) ;
#77266 = CARTESIAN_POINT ( 'NONE',  ( 14.98227958311676744, 15.82868232077399462, -1.500000000000002220 ) ) ;
#77267 = PLANE ( 'NONE',  #51388 ) ;
#77268 = PLANE ( 'NONE',  #87438 ) ;
#77269 = CARTESIAN_POINT ( 'NONE',  ( -80.41333690452883332, -25.13350261022028675, 7.099562396224023963 ) ) ;
#77270 = CARTESIAN_POINT ( 'NONE',  ( 3.267597511969735802, 21.59432767039258394, -1.500000000000002220 ) ) ;
#77271 = CARTESIAN_POINT ( 'NONE',  ( -71.27229073968156570, -25.31639491978751622, 4.988759705255076504 ) ) ;
#77272 = ORIENTED_EDGE ( 'NONE', *, *, #12776, .F. ) ;
#77273 = EDGE_CURVE ( 'NONE', #46259, #43349, #86692, .T. ) ;
#77274 = CARTESIAN_POINT ( 'NONE',  ( 7.344278919687202922, -5.876774720514417183, 20.19896341048075783 ) ) ;
#77275 = CARTESIAN_POINT ( 'NONE',  ( 8.160000000000000142, -10.65233964170348635, -1.621096496867198589 ) ) ;
#77276 = CARTESIAN_POINT ( 'NONE',  ( 32.54161589056530346, -4.044086941844335925, -1.517980283019001453 ) ) ;
#77277 = ORIENTED_EDGE ( 'NONE', *, *, #34815, .F. ) ;
#77278 = VECTOR ( 'NONE', #60233, 1000.000000000000114 ) ;
#77279 = ORIENTED_EDGE ( 'NONE', *, *, #34131, .T. ) ;
#77280 = EDGE_LOOP ( 'NONE', ( #72386, #41346, #59571, #72696 ) ) ;
#77281 = CARTESIAN_POINT ( 'NONE',  ( -63.62287095715003460, -23.48783264082478084, -1.443836473390069042 ) ) ;
#77282 = CARTESIAN_POINT ( 'NONE',  ( 20.83148622972472808, -3.941400823363257366, 11.49999999999998934 ) ) ;
#77283 = CARTESIAN_POINT ( 'NONE',  ( -94.62287095715005592, -24.65952944569304606, 1.056160979905700348 ) ) ;
#77284 = CARTESIAN_POINT ( 'NONE',  ( -79.02216967728209340, -25.27791743151245996, 6.505900957663475204 ) ) ;
#77285 = CARTESIAN_POINT ( 'NONE',  ( -60.52287095715006160, -24.99156044556119838, 7.747789690856173195 ) ) ;
#77286 = AXIS2_PLACEMENT_3D ( 'NONE', #60668, #44941, #45442 ) ;
#77287 = CARTESIAN_POINT ( 'NONE',  ( 5.635247460261607166, -5.876774720514424288, 21.53093896358932469 ) ) ;
#77288 = CARTESIAN_POINT ( 'NONE',  ( 11.20917403917954225, 15.81763734437701885, 11.49999999999998934 ) ) ;
#77289 = CARTESIAN_POINT ( 'NONE',  ( -69.35003614255256821, -25.26766161569622682, 6.083062509053539735 ) ) ;
#77290 = EDGE_LOOP ( 'NONE', ( #48805, #75404, #72286, #86962 ) ) ;
#77291 = CIRCLE ( 'NONE', #51387, 129.7684398600581517 ) ;
#77292 = CARTESIAN_POINT ( 'NONE',  ( -9.780116039169133302, 16.78644576961053048, 11.49999999999999645 ) ) ;
#77293 = LINE ( 'NONE', #7796, #56895 ) ;
#77294 = AXIS2_PLACEMENT_3D ( 'NONE', #93619, #16495, #8897 ) ;
#77295 = CARTESIAN_POINT ( 'NONE',  ( -103.5228709571500758, -24.64965694238408034, 8.947790433994194714 ) ) ;
#77296 = B_SPLINE_CURVE_WITH_KNOTS ( 'NONE', 3,
 ( #91913, #69593, #30518, #7683 ),
 .UNSPECIFIED., .F., .F.,
 ( 4, 4 ),
 ( 0.000000000000000000, 9.999999999998897304E-05 ),
 .UNSPECIFIED. ) ;
#77297 = ORIENTED_EDGE ( 'NONE', *, *, #80364, .F. ) ;
#77298 = CARTESIAN_POINT ( 'NONE',  ( 2.936453026386435017, -6.376774720514406525, 18.60215244312560401 ) ) ;
#77299 = LINE ( 'NONE', #61108, #99849 ) ;
#77300 = CARTESIAN_POINT ( 'NONE',  ( -91.62287095715004170, -23.47596703998600631, 11.44779298504227860 ) ) ;
#77301 = EDGE_CURVE ( 'NONE', #87827, #29179, #54259, .T. ) ;
#77302 = CARTESIAN_POINT ( 'NONE',  ( -93.51252845903317734, -24.15620529776628800, 10.23563542870659582 ) ) ;
#77303 = CARTESIAN_POINT ( 'NONE',  ( -15.96901387740391343, -11.39031854172415947, 11.49999999999998934 ) ) ;
#77304 = CARTESIAN_POINT ( 'NONE',  ( -117.6228709571500701, -24.66019654487199730, 8.947790411086121054 ) ) ;
#77305 = ORIENTED_EDGE ( 'NONE', *, *, #12334, .T. ) ;
#77306 = CARTESIAN_POINT ( 'NONE',  ( 11.83326311654409935, 18.06170320929925310, -1.500000000000002220 ) ) ;
#77307 = CARTESIAN_POINT ( 'NONE',  ( -120.5228709571500616, -24.99132157543167310, 2.256160258750667502 ) ) ;
#77309 = B_SPLINE_CURVE_WITH_KNOTS ( 'NONE', 3,
 ( #41687, #96953, #35063, #9720, #80229, #72633, #48799, #89348, #3125, #26944, #33062, #34063, #65039, #73128, #42687, #25942 ),
 .UNSPECIFIED., .F., .F.,
 ( 4, 2, 2, 2, 2, 2, 2, 4 ),
 ( 2.602085213965210642E-18, 0.0002042144920037962993, 0.0004084289840075899965, 0.0006126434760113836937, 0.0008168579680151773909, 0.001225286952022764785, 0.001429501444026539184, 0.001633715936030313799 ),
 .UNSPECIFIED. ) ;
#77308 = DIRECTION ( 'NONE',  ( 1.000000000000000000, 0.000000000000000000, 0.000000000000000000 ) ) ;
#77310 = DIRECTION ( 'NONE',  ( -0.000000000000000000, 1.000000000000000000, -0.000000000000000000 ) ) ;
#77311 = CARTESIAN_POINT ( 'NONE',  ( 7.103900956763240515, -21.94381868531750968, -1.500000000000002220 ) ) ;
#77312 = EDGE_CURVE ( 'NONE', #61929, #27949, #13456, .T. ) ;
#77313 = APPROVAL_DATE_TIME ( #31647, #71746 ) ;
#77314 = PLANE ( 'NONE',  #35378 ) ;
#77315 = DIRECTION ( 'NONE',  ( 0.09824042138329625029, 2.980407940728111021E-17, -0.9951627101165079203 ) ) ;
#77316 = CARTESIAN_POINT ( 'NONE',  ( -121.5550104420377409, -24.15620529776628800, 10.23563542870660115 ) ) ;
#77317 = CARTESIAN_POINT ( 'NONE',  ( -104.5228709571500758, -23.47596703998600631, 11.44779298504228215 ) ) ;
#77318 = CARTESIAN_POINT ( 'NONE',  ( -111.3477393431454487, -25.29823902580309891, 3.253010139271965251 ) ) ;
#77319 = CARTESIAN_POINT ( 'NONE',  ( -129.6235277210520564, -24.51314013834316796, 0.6176544820404222813 ) ) ;
#77320 = CARTESIAN_POINT ( 'NONE',  ( -99.32787325113280019, -25.31566036122295671, 4.639922477934026901 ) ) ;
#77321 = CARTESIAN_POINT ( 'NONE',  ( 19.23997954701083657, -5.074110557352235595, 11.49999999999998934 ) ) ;
#77322 = CARTESIAN_POINT ( 'NONE',  ( -41.52287095715005449, -23.48783264083359867, -1.443836473376375329 ) ) ;
#77323 = CARTESIAN_POINT ( 'NONE',  ( -8.418173371947181849, -17.93405594323863284, -1.500000000000002220 ) ) ;
#77324 = AXIS2_PLACEMENT_3D ( 'NONE', #58961, #82285, #5163 ) ;
#77325 = CARTESIAN_POINT ( 'NONE',  ( -0.3982818654701407723, -5.876774720514410966, 19.46306892155547530 ) ) ;
#77326 = CARTESIAN_POINT ( 'NONE',  ( -108.5895376238167245, -24.64898659630368627, 1.056161002820390493 ) ) ;
#77327 = FACE_OUTER_BOUND ( 'NONE', #91224, .T. ) ;
#77328 = CARTESIAN_POINT ( 'NONE',  ( 20.74337371777590278, 0.4424840333690017724, 11.49999999999999645 ) ) ;
#77329 = VECTOR ( 'NONE', #18534, 1000.000000000000114 ) ;
#77330 = FACE_OUTER_BOUND ( 'NONE', #33871, .T. ) ;
#77331 = APPROVAL ( #59624, 'UNSPECIFIED' ) ;
#77332 = CARTESIAN_POINT ( 'NONE',  ( -106.5895376238167387, -24.66019654487199730, 8.947790411086117501 ) ) ;
#77333 = CARTESIAN_POINT ( 'NONE',  ( 22.70222466501550329, 0.2752559529566028229, 11.49999999999999645 ) ) ;
#77334 = EDGE_LOOP ( 'NONE', ( #35188, #94560, #35923, #89867 ) ) ;
#77335 = B_SPLINE_SURFACE_WITH_KNOTS ( 'NONE', 3, 3, ( 
 ( #93328, #15209, #22802, #14704 ),
 ( #30934, #76595, #69998, #1502 ),
 ( #45670, #485, #69506, #78590 ),
 ( #91830, #61405, #9100, #53788 ),
 ( #71012, #995, #99924, #92828 ),
 ( #46169, #61902, #23310, #62398 ),
 ( #7098, #38047, #16710, #69000 ) ),
 .UNSPECIFIED., .F., .F., .F.,
 ( 4, 3, 4 ),
 ( 4, 4 ),
 ( 0.7945040050992244751, 0.8970133687736505657, 0.9995227324480766562 ),
 ( 0.9197277128001624114, 0.9211650446997299291 ),
 .UNSPECIFIED. ) ;
#77336 = DIRECTION ( 'NONE',  ( -3.773278334444166432E-23, 1.000000000000000000, 0.000000000000000000 ) ) ;
#77337 = CARTESIAN_POINT ( 'NONE',  ( -106.6228709571500985, -24.33832256527048798, 0.1851278514138634534 ) ) ;
#77338 = ORIENTED_EDGE ( 'NONE', *, *, #8788, .T. ) ;
#77339 = CARTESIAN_POINT ( 'NONE',  ( -16.67386609800740516, 11.36076560755915033, -1.500000000000002220 ) ) ;
#77340 = LINE ( 'NONE', #100164, #53273 ) ;
#77341 = CARTESIAN_POINT ( 'NONE',  ( -95.62287095715009855, -24.82558206586144323, 1.605769216559443935 ) ) ;
#77342 = VERTEX_POINT ( 'NONE', #63888 ) ;
#77343 = AXIS2_PLACEMENT_3D ( 'NONE', #88817, #49765, #11184 ) ;
#77344 = EDGE_LOOP ( 'NONE', ( #52552, #13875, #97464, #34198 ) ) ;
#77345 = PLANE ( 'NONE',  #35507 ) ;
#77346 = CARTESIAN_POINT ( 'NONE',  ( 12.20170062390598709, -19.39347807479101249, -1.500000000000002220 ) ) ;
#77347 = CARTESIAN_POINT ( 'NONE',  ( -51.28182533633388829, -25.18439771871680577, 3.855515987445083503 ) ) ;
#77348 = CARTESIAN_POINT ( 'NONE',  ( 17.85095790706337127, 12.24325521369631176, -1.500000000000002220 ) ) ;
#77349 = CARTESIAN_POINT ( 'NONE',  ( -123.5905688118583470, -23.96119346886881019, -0.6495511937832022520 ) ) ;
#77350 = CARTESIAN_POINT ( 'NONE',  ( -3.961239394588834895, 20.55660451852329018, 11.49999999999999645 ) ) ;
#77351 = ORIENTED_EDGE ( 'NONE', *, *, #26642, .T. ) ;
#77352 = CARTESIAN_POINT ( 'NONE',  ( -68.94044447473358161, -25.31612700224413004, 6.138838773723374942 ) ) ;
#77353 = CARTESIAN_POINT ( 'NONE',  ( -15.57331531552114612, -15.56871402003811333, -1.500000000000002220 ) ) ;
#77354 = VECTOR ( 'NONE', #24717, 1000.000000000000114 ) ;
#77355 = CARTESIAN_POINT ( 'NONE',  ( -127.4728709571500360, -25.21113200442379565, 5.000950862978372768 ) ) ;
#77356 = CARTESIAN_POINT ( 'NONE',  ( -30.47287095715007155, -25.10123602413552035, 7.248486769786293138 ) ) ;
#77357 = ORIENTED_EDGE ( 'NONE', *, *, #53700, .F. ) ;
#77358 = CARTESIAN_POINT ( 'NONE',  ( 4.039061187531148178, -6.376774720514401196, 18.18637930035166761 ) ) ;
#77359 = DIRECTION ( 'NONE',  ( -0.000000000000000000, 1.000000000000000000, -0.000000000000000000 ) ) ;
#77360 = ORIENTED_EDGE ( 'NONE', *, *, #29880, .T. ) ;
#77361 = CARTESIAN_POINT ( 'NONE',  ( -72.50700632870835705, -24.15620529776627734, 10.23563542870660825 ) ) ;
#77362 = ORIENTED_EDGE ( 'NONE', *, *, #46869, .T. ) ;
#77363 = VECTOR ( 'NONE', #55477, 1000.000000000000000 ) ;
#77364 = VERTEX_POINT ( 'NONE', #38517 ) ;
#77365 = ADVANCED_FACE ( 'NONE', ( #93804 ), #24297, .F. ) ;
#77366 = CARTESIAN_POINT ( 'NONE',  ( -32.55620429048340014, -24.64898659630528854, 1.056161002820822592 ) ) ;
#77367 = CARTESIAN_POINT ( 'NONE',  ( -74.52287095715007581, -29.50247984919015209, -1.443849546365055359 ) ) ;
#77368 = CARTESIAN_POINT ( 'NONE',  ( -4.635780534842457001, -6.376774720514410077, 19.53657742262743113 ) ) ;
#77369 = CARTESIAN_POINT ( 'NONE',  ( 19.38413035786728145, -6.671778716439519030, -1.500000000000002220 ) ) ;
#77370 = VERTEX_POINT ( 'NONE', #86194 ) ;
#77371 = CARTESIAN_POINT ( 'NONE',  ( -71.62287095715005592, -23.73934037231757443, 11.05740245334328975 ) ) ;
#77372 = CARTESIAN_POINT ( 'NONE',  ( -33.62287095715006302, -23.73934037231755667, 11.05740245334329508 ) ) ;
#77373 = PLANE ( 'NONE',  #33786 ) ;
#77374 = CARTESIAN_POINT ( 'NONE',  ( -19.83904684311861644, 10.14288308415042827, -1.500000000000002220 ) ) ;
#77375 = CARTESIAN_POINT ( 'NONE',  ( -4.141025641025641413, -6.376774720514420736, 20.67377804487180271 ) ) ;
#77376 = CARTESIAN_POINT ( 'NONE',  ( -101.5228709571500758, -24.64898659630368627, 1.056161002820829697 ) ) ;
#77377 = ORIENTED_EDGE ( 'NONE', *, *, #88684, .F. ) ;
#77378 = FACE_BOUND ( 'NONE', #70418, .T. ) ;
#77379 = CARTESIAN_POINT ( 'NONE',  ( -39.52287095715006870, -24.66019654487198665, 8.947790411086131712 ) ) ;
#77380 = EDGE_CURVE ( 'NONE', #1020, #39331, #94803, .T. ) ;
#77381 = CARTESIAN_POINT ( 'NONE',  ( -20.82185584224439978, -0.2524610531272265534, -1.500000000000002220 ) ) ;
#77382 = EDGE_CURVE ( 'NONE', #2549, #3403, #27792, .T. ) ;
#77383 = ORIENTED_EDGE ( 'NONE', *, *, #77992, .F. ) ;
#77385 = ORIENTED_EDGE ( 'NONE', *, *, #20213, .F. ) ;
#77384 = CARTESIAN_POINT ( 'NONE',  ( -42.52287095715005449, -23.48786465467240347, 11.44779295918255180 ) ) ;
#77386 = CARTESIAN_POINT ( 'NONE',  ( -50.85935151307011637, -25.12217849056909813, 7.039179954492152724 ) ) ;
#77387 = CARTESIAN_POINT ( 'NONE',  ( 12.86141378215833342, 16.59024694808438127, -1.500000000000002220 ) ) ;
#77388 = ORIENTED_EDGE ( 'NONE', *, *, #49612, .F. ) ;
#77389 = CARTESIAN_POINT ( 'NONE',  ( 31.25756411700558601, -5.804570343751186634, -1.813502816810933949 ) ) ;
#77390 = CARTESIAN_POINT ( 'NONE',  ( -55.62287095715004170, -24.14406661707768720, 10.28769366152059561 ) ) ;
#77391 = CARTESIAN_POINT ( 'NONE',  ( 10.22011794244940752, -3.316774720515020203, -27.02313658111319938 ) ) ;
#77392 = B_SPLINE_CURVE_WITH_KNOTS ( 'NONE', 3,
 ( #51283, #18823, #43671, #34568, #82223, #56916 ),
 .UNSPECIFIED., .F., .F.,
 ( 4, 2, 4 ),
 ( 0.000000000000000000, 0.001380764517854766700, 0.002761529035709533401 ),
 .UNSPECIFIED. ) ;
#77393 = LINE ( 'NONE', #23104, #89047 ) ;
#77394 = CARTESIAN_POINT ( 'NONE',  ( -92.59430328945671818, -23.96169478059713498, 10.65365249895717881 ) ) ;
#77395 = PLANE ( 'NONE',  #87015 ) ;
#77397 = ORIENTED_EDGE ( 'NONE', *, *, #11905, .F. ) ;
#77396 = CARTESIAN_POINT ( 'NONE',  ( -14.87450875942801254, -16.50811611944624602, 11.49999999999999645 ) ) ;
#77398 = EDGE_CURVE ( 'NONE', #4386, #91196, #83228, .T. ) ;
#77399 = CARTESIAN_POINT ( 'NONE',  ( -37.62287095715005592, -23.48786465467240347, 11.44779295918255180 ) ) ;
#77400 = EDGE_LOOP ( 'NONE', ( #97722, #18396, #18003, #55451 ) ) ;
#77401 = CARTESIAN_POINT ( 'NONE',  ( -17.75566480456612695, 14.03706703302619374, -1.500000000000002220 ) ) ;
#77403 = ORIENTED_EDGE ( 'NONE', *, *, #65518, .T. ) ;
#77402 = CARTESIAN_POINT ( 'NONE',  ( -111.5228709571500758, -23.96177878511310055, 10.65340807706329507 ) ) ;
#77404 = ORIENTED_EDGE ( 'NONE', *, *, #92933, .T. ) ;
#77405 = PLANE ( 'NONE',  #49914 ) ;
#77406 = B_SPLINE_CURVE_WITH_KNOTS ( 'NONE', 3,
 ( #192, #62604, #31134, #54484, #15906, #77794 ),
 .UNSPECIFIED., .F., .F.,
 ( 4, 2, 4 ),
 ( 0.000000000000000000, 0.001380764517854763881, 0.002761529035709527763 ),
 .UNSPECIFIED. ) ;
#77407 = CARTESIAN_POINT ( 'NONE',  ( -17.50950832565593984, 9.922426906265528146, -1.500000000000002220 ) ) ;
#77408 = LINE ( 'NONE', #54109, #50602 ) ;
#77409 = ORIENTED_EDGE ( 'NONE', *, *, #87332, .T. ) ;
#77410 = DIRECTION ( 'NONE',  ( -0.000000000000000000, -1.000000000000000000, -0.000000000000000000 ) ) ;
#77411 = CARTESIAN_POINT ( 'NONE',  ( -20.55042600948665310, 8.738301046694649798, -1.500000000000002220 ) ) ;
#77412 = EDGE_CURVE ( 'NONE', #60463, #7274, #95803, .T. ) ;
#77413 = ORIENTED_EDGE ( 'NONE', *, *, #83082, .F. ) ;
#77414 = ORIENTED_EDGE ( 'NONE', *, *, #32898, .T. ) ;
#77415 = FACE_OUTER_BOUND ( 'NONE', #13219, .T. ) ;
#77416 = CARTESIAN_POINT ( 'NONE',  ( -94.58428862232342738, -24.66019654487199730, 8.947790411086121054 ) ) ;
#77417 = LINE ( 'NONE', #54606, #16657 ) ;
#77418 = CARTESIAN_POINT ( 'NONE',  ( -62.52287095715006160, -23.47593901973090169, -1.443836447538997092 ) ) ;
#77419 = AXIS2_PLACEMENT_3D ( 'NONE', #95180, #72853, #88574 ) ;
#77420 = CARTESIAN_POINT ( 'NONE',  ( -30.64427850938830389, -23.47593901973090169, -1.443836447538998646 ) ) ;
#77421 = CARTESIAN_POINT ( 'NONE',  ( 11.58774116221665729, 15.72987433093905096, 11.49999999999998934 ) ) ;
#77422 = FACE_OUTER_BOUND ( 'NONE', #25314, .T. ) ;
#77423 = CARTESIAN_POINT ( 'NONE',  ( 10.13398631766115443, 18.95262098133242290, -1.500000000000002220 ) ) ;
#77424 = CARTESIAN_POINT ( 'NONE',  ( -128.5559270644360481, -23.96119346886882084, -0.6495511937831803806 ) ) ;
#77425 = CARTESIAN_POINT ( 'NONE',  ( -54.62287095715006302, -24.50321055353805377, 9.387540953477531147 ) ) ;
#77426 = DIRECTION ( 'NONE',  ( 1.000000000000000000, -2.209838822900391329E-16, 0.000000000000000000 ) ) ;
#77427 = DIRECTION ( 'NONE',  ( 0.000000000000000000, -0.000000000000000000, -1.000000000000000000 ) ) ;
#77428 = CARTESIAN_POINT ( 'NONE',  ( 22.56601425305882813, -3.627385684441148506, -1.500000000000002220 ) ) ;
#77429 = VECTOR ( 'NONE', #19851, 1000.000000000000000 ) ;
#77430 = EDGE_CURVE ( 'NONE', #17712, #47723, #34912, .T. ) ;
#77431 = COORDINATED_UNIVERSAL_TIME_OFFSET ( 0, 0, .AHEAD. ) ;
#77432 = DIRECTION ( 'NONE',  ( 3.773278334444166432E-23, -1.000000000000000000, 0.000000000000000000 ) ) ;
#77433 = CARTESIAN_POINT ( 'NONE',  ( -2.786875287040666560, -5.876774720514418071, 20.09505574050193388 ) ) ;
#77434 = CARTESIAN_POINT ( 'NONE',  ( -9.072532997253766496, -17.89392090870456542, 11.49999999999999645 ) ) ;
#77435 = CARTESIAN_POINT ( 'NONE',  ( -5.366453405989235925, -2.000000000000005329, 19.19609335255483629 ) ) ;
#77436 = FACE_OUTER_BOUND ( 'NONE', #28205, .T. ) ;
#77437 = AXIS2_PLACEMENT_3D ( 'NONE', #38617, #55362, #86293 ) ;
#77438 = DIRECTION ( 'NONE',  ( 0.7512896232465891000, 0.000000000000000000, 0.6599726524652351767 ) ) ;
#77439 = CARTESIAN_POINT ( 'NONE',  ( -39.58953762381673158, -23.47596703998600276, 11.44779298504227505 ) ) ;
#77440 = ORIENTED_EDGE ( 'NONE', *, *, #70156, .T. ) ;
#77441 = CARTESIAN_POINT ( 'NONE',  ( -22.05275734969026047, -5.965225279485572685, 30.51402280011862089 ) ) ;
#77442 = CARTESIAN_POINT ( 'NONE',  ( -109.1326033789950145, -25.21121287918716902, 3.488800947434629762 ) ) ;
#77443 = CARTESIAN_POINT ( 'NONE',  ( -21.53672441135761773, -2.854535511010750870, -1.500000000000002220 ) ) ;
#77444 = PLANE ( 'NONE',  #35077 ) ;
#77445 = CARTESIAN_POINT ( 'NONE',  ( -19.13235715846047214, 4.354950445902704637, -1.500000000000002220 ) ) ;
#77446 = DIRECTION ( 'NONE',  ( 1.000000000000000000, 0.000000000000000000, 0.000000000000000000 ) ) ;
#77447 = AXIS2_PLACEMENT_3D ( 'NONE', #39264, #39761, #23523 ) ;
#77448 = CARTESIAN_POINT ( 'NONE',  ( -109.8661607933284472, -25.27925885274750328, 5.216081408360091487 ) ) ;
#77449 = SECURITY_CLASSIFICATION_LEVEL ( 'unclassified' ) ;
#77450 = B_SPLINE_CURVE_WITH_KNOTS ( 'NONE', 3,
 ( #82963, #84468, #54037, #62146, #14449, #77341, #14949, #93070 ),
 .UNSPECIFIED., .F., .F.,
 ( 4, 2, 2, 4 ),
 ( 0.000000000000000000, 0.002001098010032682350, 0.003001647015049025043, 0.004002196020065368169 ),
 .UNSPECIFIED. ) ;
#77451 = PLANE ( 'NONE',  #41896 ) ;
#77452 = CARTESIAN_POINT ( 'NONE',  ( -47.52287095715009713, -23.95044443724992789, 10.65354141964649415 ) ) ;
#77453 = CARTESIAN_POINT ( 'NONE',  ( -19.39287000742378453, 6.875061630626206011, 11.49999999999999645 ) ) ;
#77454 = CARTESIAN_POINT ( 'NONE',  ( -39.04496671189667723, -25.29399908399037145, 4.275509040138983252 ) ) ;
#77455 = CARTESIAN_POINT ( 'NONE',  ( -47.62287095715004170, -24.65952944569304250, 1.056160979905693686 ) ) ;
#77456 = EDGE_CURVE ( 'NONE', #44339, #38457, #45854, .T. ) ;
#77457 = EDGE_LOOP ( 'NONE', ( #50751, #38835, #3137, #67945 ) ) ;
#77458 = CARTESIAN_POINT ( 'NONE',  ( -99.52764846858842418, -25.26387293761020914, 3.999772272046739907 ) ) ;
#77459 = CARTESIAN_POINT ( 'NONE',  ( 1.095236984349686971, 8.494825072090639750, -1.700000000000008837 ) ) ;
#77460 = CARTESIAN_POINT ( 'NONE',  ( -74.52287095715007581, -24.50321055353805377, 9.387540953477508054 ) ) ;
#77461 = CARTESIAN_POINT ( 'NONE',  ( -69.55620429048336462, -24.64965694238574656, 8.947790433994198267 ) ) ;
#77462 = ADVANCED_FACE ( 'NONE', ( #79581 ), #8651, .T. ) ;
#77463 = CARTESIAN_POINT ( 'NONE',  ( -28.98875734969026396, -5.965225279485572685, 0.1180228001186258285 ) ) ;
#77464 = CARTESIAN_POINT ( 'NONE',  ( -32.52287095715006160, -23.47596703998600631, 11.44779298504229459 ) ) ;
#77465 = EDGE_CURVE ( 'NONE', #20674, #80, #65885, .T. ) ;
#77466 = EDGE_CURVE ( 'NONE', #22711, #32453, #10567, .T. ) ;
#77467 = CARTESIAN_POINT ( 'NONE',  ( -23.06710473063640165, 0.7821689226722955413, 11.49999999999999645 ) ) ;
#77468 = CARTESIAN_POINT ( 'NONE',  ( 18.64237364862239943, 13.12531859369229359, 11.49999999999998934 ) ) ;
#77469 = CARTESIAN_POINT ( 'NONE',  ( -74.55412977414610509, -23.96119346886879953, -0.6495511937832119109 ) ) ;
#77470 = B_SPLINE_SURFACE_WITH_KNOTS ( 'NONE', 3, 3, ( 
 ( #94421, #54371, #85813, #41152 ),
 ( #24904, #23904, #94924, #93916 ),
 ( #15789, #32525, #70589, #79194 ),
 ( #64007, #62483, #2097, #1080 ),
 ( #61983, #31518, #55375, #86310 ),
 ( #2591, #9182, #16293, #71098 ),
 ( #39633, #24408, #39130, #40143 ) ),
 .UNSPECIFIED., .F., .F., .F.,
 ( 4, 3, 4 ),
 ( 4, 4 ),
 ( 0.0004766839783844487510, 0.1029713700210909688, 0.2054660560637974753 ),
 ( 0.3095727472661086721, 0.3107283081189128326 ),
 .UNSPECIFIED. ) ;
#77471 = CARTESIAN_POINT ( 'NONE',  ( -67.52287095715003318, -23.73907113216989728, -1.053371485793251905 ) ) ;
#77472 = CARTESIAN_POINT ( 'NONE',  ( -104.5228709571500758, -24.66019654487200441, 8.947790411086113949 ) ) ;
#77473 = EDGE_CURVE ( 'NONE', #14898, #63088, #58256, .T. ) ;
#77474 = CARTESIAN_POINT ( 'NONE',  ( 20.43785579724129420, 9.289222182981756504, 11.49999999999999645 ) ) ;
#77475 = EDGE_LOOP ( 'NONE', ( #3746, #31038, #33138, #58557, #76416, #22885, #19749, #25489, #72327 ) ) ;
#77476 = CARTESIAN_POINT ( 'NONE',  ( 8.676776695296466002, 18.57322330470350735, 2.100000000000000089 ) ) ;
#77477 = CARTESIAN_POINT ( 'NONE',  ( -70.62287095715005592, -25.00182538069145011, 7.747789668545097541 ) ) ;
#77478 = CARTESIAN_POINT ( 'NONE',  ( -17.33335002049248530, 13.43749923854009509, 11.49999999999998934 ) ) ;
#77479 = FACE_OUTER_BOUND ( 'NONE', #76511, .T. ) ;
#77480 = CARTESIAN_POINT ( 'NONE',  ( -87.59165135172374050, -24.15620529776628445, 10.23563542870660292 ) ) ;
#77481 = FACE_OUTER_BOUND ( 'NONE', #77114, .T. ) ;
#77482 = CARTESIAN_POINT ( 'NONE',  ( -129.6228709571500417, -29.50248528299804818, 1.056150453629047137 ) ) ;
#77483 = DIRECTION ( 'NONE',  ( -0.000000000000000000, 1.000000000000000000, -0.000000000000000000 ) ) ;
#77484 = ORIENTED_EDGE ( 'NONE', *, *, #51535, .F. ) ;
#77485 = CARTESIAN_POINT ( 'NONE',  ( -20.46784169311667867, 0.4426517378232717737, -1.500000000000002220 ) ) ;
#77486 = ORIENTED_EDGE ( 'NONE', *, *, #31146, .T. ) ;
#77487 = VERTEX_POINT ( 'NONE', #19669 ) ;
#77488 = EDGE_LOOP ( 'NONE', ( #11640, #32459, #63710, #59833 ) ) ;
#77489 = EDGE_LOOP ( 'NONE', ( #46922, #5767, #37602, #86272 ) ) ;
#77490 = EDGE_CURVE ( 'NONE', #7016, #57758, #55395, .T. ) ;
#77491 = CARTESIAN_POINT ( 'NONE',  ( -14.75821945985506645, 17.75411527500383002, 11.49999999999998934 ) ) ;
#77492 = DIRECTION ( 'NONE',  ( 3.773278334444166432E-23, -1.000000000000000000, 0.000000000000000000 ) ) ;
#77493 = CARTESIAN_POINT ( 'NONE',  ( 9.679018533540549640, -17.85022214266596308, -1.500000000000002220 ) ) ;
#77494 = EDGE_LOOP ( 'NONE', ( #85483, #17799, #93109, #4631, #4553 ) ) ;
#77495 = CARTESIAN_POINT ( 'NONE',  ( 29.70264281947218876, 3.584400861594816856, 28.19233905662918005 ) ) ;
#77496 = AXIS2_PLACEMENT_3D ( 'NONE', #68859, #29794, #84074 ) ;
#77497 = CARTESIAN_POINT ( 'NONE',  ( -72.52287095715006160, -24.50216790748204332, 0.6166512839542518387 ) ) ;
#77498 = LINE ( 'NONE', #61308, #62650 ) ;
#77499 = CARTESIAN_POINT ( 'NONE',  ( -99.63766830052645673, -23.48786465467241413, 11.44779295918254292 ) ) ;
#77501 = VERTEX_POINT ( 'NONE', #48657 ) ;
#77500 = CARTESIAN_POINT ( 'NONE',  ( -15.45034113870702441, -14.97902827799142500, 11.49999999999999645 ) ) ;
#77502 = CARTESIAN_POINT ( 'NONE',  ( -75.58062029086705991, -24.92564183028979130, 1.928384488918256645 ) ) ;
#77503 = CARTESIAN_POINT ( 'NONE',  ( -61.55369053405362934, -23.96169478059712787, 10.65365249895718591 ) ) ;
#77504 = VERTEX_POINT ( 'NONE', #59754 ) ;
#77505 = CARTESIAN_POINT ( 'NONE',  ( 17.59156710592704442, 10.99281682905060897, -1.500000000000002220 ) ) ;
#77506 = EDGE_CURVE ( 'NONE', #42081, #50071, #16722, .T. ) ;
#77507 = ORIENTED_EDGE ( 'NONE', *, *, #25163, .F. ) ;
#77509 = VERTEX_POINT ( 'NONE', #98283 ) ;
#77508 = CARTESIAN_POINT ( 'NONE',  ( 15.29947330337542688, 3.316774720514426456, -27.16854002387010070 ) ) ;
#77510 = EDGE_CURVE ( 'NONE', #92435, #31493, #67864, .T. ) ;
#77511 = CARTESIAN_POINT ( 'NONE',  ( 32.60294298177596062, 6.475225279485573360, -11.48871326860665043 ) ) ;
#77512 = CARTESIAN_POINT ( 'NONE',  ( -48.52287095715004028, -24.34917612407046050, 0.1852690917481008004 ) ) ;
#77513 = ORIENTED_EDGE ( 'NONE', *, *, #55997, .F. ) ;
#77514 = ORIENTED_EDGE ( 'NONE', *, *, #87170, .T. ) ;
#77515 = CARTESIAN_POINT ( 'NONE',  ( -1.358974358974355257, -6.376774720514427841, 21.75000000000000711 ) ) ;
#77516 = VECTOR ( 'NONE', #37832, 1000.000000000000000 ) ;
#77517 = CARTESIAN_POINT ( 'NONE',  ( -42.61655362215102372, -23.48786465467240347, 11.44779295918255535 ) ) ;
#77518 = CARTESIAN_POINT ( 'NONE',  ( -65.54247407030995021, -24.52300882791528736, 0.6510814631126250474 ) ) ;
#77519 = CARTESIAN_POINT ( 'NONE',  ( 19.49364837986538745, 10.19379059548657551, 11.49999999999999645 ) ) ;
#77520 = ADVANCED_FACE ( 'NONE', ( #99770 ), #84068, .F. ) ;
#77521 = FACE_BOUND ( 'NONE', #44718, .T. ) ;
#77522 = CARTESIAN_POINT ( 'NONE',  ( -8.633696204196466439, -20.85254729778420923, -1.500000000000002220 ) ) ;
#77523 = CARTESIAN_POINT ( 'NONE',  ( 12.56776941831905070, -16.83212535568997126, -1.500000000000002220 ) ) ;
#77524 = EDGE_CURVE ( 'NONE', #23209, #57615, #20667, .T. ) ;
#77525 = CARTESIAN_POINT ( 'NONE',  ( -127.5228709571500616, -29.50250243563736774, 8.947779886222132717 ) ) ;
#77526 = EDGE_LOOP ( 'NONE', ( #18755, #94913, #19619, #82279 ) ) ;
#77527 = ADVANCED_FACE ( 'NONE', ( #13053 ), #28790, .T. ) ;
#77528 = AXIS2_PLACEMENT_3D ( 'NONE', #2610, #25930, #42181 ) ;
#77529 = ORIENTED_EDGE ( 'NONE', *, *, #43436, .T. ) ;
#77530 = FACE_OUTER_BOUND ( 'NONE', #5288, .T. ) ;
#77531 = CARTESIAN_POINT ( 'NONE',  ( -20.54356019850136050, 6.435454313062578535, -1.500000000000002220 ) ) ;
#77532 = DIRECTION ( 'NONE',  ( 0.000000000000000000, 0.000000000000000000, 1.000000000000000000 ) ) ;
#77533 = ORIENTED_EDGE ( 'NONE', *, *, #18337, .F. ) ;
#77534 = CARTESIAN_POINT ( 'NONE',  ( 1.812468502196824760, -21.08352789287561180, -1.500000000000002220 ) ) ;
#77535 = CARTESIAN_POINT ( 'NONE',  ( -126.6228709571501696, -24.51283580621365132, 0.6167428607019908027 ) ) ;
#77536 = CARTESIAN_POINT ( 'NONE',  ( -60.72641359848758214, -25.29489609436098263, 6.057563354383567855 ) ) ;
#77537 = CARTESIAN_POINT ( 'NONE',  ( -121.5198938983199923, -24.15543982623907127, -0.2315651400026573492 ) ) ;
#77538 = CARTESIAN_POINT ( 'NONE',  ( 15.00000000000000533, 0.000000000000000000, 19.30000000000000071 ) ) ;
#77539 = CARTESIAN_POINT ( 'NONE',  ( -127.5228709571500332, -23.73934037231757443, 11.05740245334327199 ) ) ;
#77540 = CARTESIAN_POINT ( 'NONE',  ( -20.56814720681451902, 8.302189128749821734, -1.500000000000002220 ) ) ;
#77541 = CARTESIAN_POINT ( 'NONE',  ( -71.58416595370849222, -24.51314013834315730, 0.6176544820404130665 ) ) ;
#77542 = ORIENTED_EDGE ( 'NONE', *, *, #51669, .F. ) ;
#77543 = CARTESIAN_POINT ( 'NONE',  ( 14.43441819135927950, -3.316774720514427344, -28.36222020317712378 ) ) ;
#77544 = LINE ( 'NONE', #70454, #70317 ) ;
#77545 = CARTESIAN_POINT ( 'NONE',  ( -126.6242557217197628, -24.15543982623907482, -0.2315651400026573492 ) ) ;
#77546 = DIRECTION ( 'NONE',  ( -1.000000000000000000, -0.000000000000000000, -0.000000000000000000 ) ) ;
#77547 = FACE_OUTER_BOUND ( 'NONE', #40476, .T. ) ;
#77548 = CARTESIAN_POINT ( 'NONE',  ( 19.04819733361787470, -3.913502273677552878, -1.500000000000002220 ) ) ;
#77549 = CARTESIAN_POINT ( 'NONE',  ( -0.4629837013611828866, -21.40787533109759977, -1.500000000000002220 ) ) ;
#77550 = CARTESIAN_POINT ( 'NONE',  ( -62.59277767315021634, -24.15543982623907482, -0.2315651400026649265 ) ) ;
#77551 = CARTESIAN_POINT ( 'NONE',  ( 10.57556460110582286, 0.7139560615726621151, 8.999999999999994671 ) ) ;
#77552 = FACE_OUTER_BOUND ( 'NONE', #42591, .T. ) ;
#77553 = CARTESIAN_POINT ( 'NONE',  ( -38.58953762381673158, -24.65952944569304250, 1.056160979905691022 ) ) ;
#77554 = CARTESIAN_POINT ( 'NONE',  ( -2.919094682108430483, 22.50186656173435296, -1.500000000000002220 ) ) ;
#77555 = B_SPLINE_SURFACE_WITH_KNOTS ( 'NONE', 3, 3, ( 
 ( #81573, #88191, #49636, #89187 ),
 ( #88689, #63875, #80566, #11061 ),
 ( #19159, #41020, #12047, #65873 ),
 ( #42027, #43017, #73960, #27288 ),
 ( #72970, #96792, #34399, #65376 ),
 ( #96297, #32904, #57749, #18172 ),
 ( #95298, #17670, #58243, #94790 ) ),
 .UNSPECIFIED., .F., .F., .F.,
 ( 4, 3, 4 ),
 ( 4, 4 ),
 ( 0.0004766839783814693634, 0.1029713700210893174, 0.2054660560637971700 ),
 ( 0.5296287257475410515, 0.5308858200244782610 ),
 .UNSPECIFIED. ) ;
#77556 = CARTESIAN_POINT ( 'NONE',  ( -63.52287095715006160, -23.48786465467241058, 11.44779295918254824 ) ) ;
#77557 = PLANE ( 'NONE',  #86482 ) ;
#77558 = CARTESIAN_POINT ( 'NONE',  ( 8.615496892348360802, 17.92367856960711947, 11.49999999999999645 ) ) ;
#77559 = CARTESIAN_POINT ( 'NONE',  ( -123.5215655060820410, -23.73791477778912196, 11.05961554403169878 ) ) ;
#77560 = AXIS2_PLACEMENT_3D ( 'NONE', #57244, #10541, #39995 ) ;
#77561 = CARTESIAN_POINT ( 'NONE',  ( -61.64687923781919920, -25.20074463982482982, 3.409327697717700278 ) ) ;
#77562 = B_SPLINE_CURVE_WITH_KNOTS ( 'NONE', 3,
 ( #96128, #27617, #82878, #82387 ),
 .UNSPECIFIED., .F., .F.,
 ( 4, 4 ),
 ( 0.000000000000000000, 9.999999999998897304E-05 ),
 .UNSPECIFIED. ) ;
#77563 = VERTEX_POINT ( 'NONE', #98788 ) ;
#77564 = LINE ( 'NONE', #51374, #85025 ) ;
#77565 = CARTESIAN_POINT ( 'NONE',  ( -6.033988668995577065, -5.876774720514413630, 19.86422795159478483 ) ) ;
#77566 = CARTESIAN_POINT ( 'NONE',  ( -115.5895376238167387, -25.00158670708909625, 2.256160236439167299 ) ) ;
#77567 = CARTESIAN_POINT ( 'NONE',  ( 4.348677445931066643, 21.19853102677161871, 11.49999999999998934 ) ) ;
#77568 = CARTESIAN_POINT ( 'NONE',  ( -124.5228709571500616, -24.64898659630368627, 1.056161002820833028 ) ) ;
#77569 = VECTOR ( 'NONE', #31215, 1000.000000000000000 ) ;
#77570 = CARTESIAN_POINT ( 'NONE',  ( -18.32239908988104204, -6.426282940459683068, -1.500000000000002220 ) ) ;
#77571 = CARTESIAN_POINT ( 'NONE',  ( -55.47780762501948715, -25.00182538069146787, 7.747789668545041586 ) ) ;
#77572 = CARTESIAN_POINT ( 'NONE',  ( -3.387584560642538101, 19.54024307811383210, -1.500000000000002220 ) ) ;
#77573 = VERTEX_POINT ( 'NONE', #91674 ) ;
#77574 = CARTESIAN_POINT ( 'NONE',  ( -16.54958403137900191, 11.88860064210666856, 11.49999999999999645 ) ) ;
#77575 = CARTESIAN_POINT ( 'NONE',  ( -80.63292597169439091, -24.52300882791530157, 0.6510814631126378149 ) ) ;
#77576 = DIRECTION ( 'NONE',  ( 9.426781450619601849E-18, -6.307606751056558338E-17, -1.000000000000000000 ) ) ;
#77577 = EDGE_CURVE ( 'NONE', #14489, #93507, #14208, .T. ) ;
#77578 = ORIENTED_EDGE ( 'NONE', *, *, #80369, .T. ) ;
#77579 = CARTESIAN_POINT ( 'NONE',  ( -78.95130178854248015, -25.24824198256244401, 6.186328973465725412 ) ) ;
#77580 = LINE ( 'NONE', #92316, #20159 ) ;
#77581 = CARTESIAN_POINT ( 'NONE',  ( -96.62287095715007013, -23.72773821059535848, 11.05748984161097503 ) ) ;
#77582 = VECTOR ( 'NONE', #27314, 1000.000000000000000 ) ;
#77583 = CARTESIAN_POINT ( 'NONE',  ( -11.64875734969026233, 0.3587747205144265483, 30.51402280011862089 ) ) ;
#77584 = CARTESIAN_POINT ( 'NONE',  ( -127.6228709571500559, -23.72773821059535848, 11.05748984161097503 ) ) ;
#77585 = CARTESIAN_POINT ( 'NONE',  ( 19.44710440357065551, 5.058846670610233076, -1.500000000000002220 ) ) ;
#77586 = DIRECTION ( 'NONE',  ( -0.09824042138329623641, -0.9951627101165078093, -3.504396110891626425E-15 ) ) ;
#77587 = ORIENTED_EDGE ( 'NONE', *, *, #55865, .F. ) ;
#77588 = EDGE_CURVE ( 'NONE', #96640, #12730, #78369, .T. ) ;
#77589 = CARTESIAN_POINT ( 'NONE',  ( -129.5895376238167387, -23.47593901973091235, -1.443836447538995760 ) ) ;
#77590 = EDGE_CURVE ( 'NONE', #67166, #40197, #20170, .T. ) ;
#77591 = EDGE_CURVE ( 'NONE', #35025, #31553, #27536, .T. ) ;
#77592 = CARTESIAN_POINT ( 'NONE',  ( -22.79553223295561892, 1.966428799096173075, 11.49999999999999645 ) ) ;
#77593 = CARTESIAN_POINT ( 'NONE',  ( -14.94938274637043207, -17.11189489004485864, -1.500000000000002220 ) ) ;
#77594 = ORIENTED_EDGE ( 'NONE', *, *, #92901, .T. ) ;
#77595 = CARTESIAN_POINT ( 'NONE',  ( -81.11505102485448049, -25.26845562246343846, 3.692626550805397478 ) ) ;
#77596 = CARTESIAN_POINT ( 'NONE',  ( -28.52287095715005805, -24.49893655963190042, 1.056161680022248195 ) ) ;
#77597 = CARTESIAN_POINT ( 'NONE',  ( -39.86131625157400293, -25.21721466608290640, 3.456295588647256611 ) ) ;
#77598 = EDGE_CURVE ( 'NONE', #33368, #1165, #6952, .T. ) ;
#77599 = CARTESIAN_POINT ( 'NONE',  ( -30.57287095715005165, -24.99054282775755098, 7.805183119964042682 ) ) ;
#77600 = CARTESIAN_POINT ( 'NONE',  ( -55.62287095715004881, -25.00158670708909625, 2.256160236439165967 ) ) ;
#77601 = CLOSED_SHELL ( 'NONE', ( #48213, #23166, #28225, #30506, #57841, #86485, #56552, #7050, #81895, #80534, #30560, #78275, #50275, #39693, #43596, #1947, #71652, #61465, #44224, #42356, #51152, #14603, #37216, #48891, #15198, #23887, #3578, #67441, #85732, #23994, #95151, #41698, #16830, #1349, #3889, #95592, #100322, #42217, #73257, #17071, #29551, #69597, #19413, #46796, #44038, #3639, #16368, #46629, #17067, #40058, #89931, #10051, #90548, #76122, #69950, #15419, #27320, #11841, #12768, #61145, #10492, #53822, #33396, #70475, #89133, #62602, #84945, #50046, #18280, #25188, #7037, #12462, #4859, #33487, #9936, #20981, #18832, #57045, #66556, #95458, #56079, #79482, #65327, #37457, #60141, #2136, #40506, #59348, #12382, #67326, #92332, #70729, #12656, #18157, #11686, #86361, #36259, #40994, #84309, #83440, #82094, #10713, #55653, #35499, #35383, #21685, #1899, #98168, #88852, #91845, #32536, #16615, #36166, #99792, #58499, #61138, #82216, #50656, #56429, #78180, #85101, #39359, #58043, #88440, #64690, #8198, #74981, #85064, #51539, #57422, #92037, #23046, #88275, #31544, #17329, #87379, #99480, #70180, #99170, #96043, #43881, #61466, #50364, #32365, #98657, #86424, #78266, #90208, #96736, #61638, #52243, #42388, #19591, #65384, #18283, #36068, #94903, #24076, #48711, #4254, #4918, #76358, #67444, #45326, #35134, #62852, #29297, #11690, #14821, #66457, #15539, #99695, #50475, #38196, #84347, #85169, #32811, #43151, #43024, #70862, #18273, #30902, #59660, #72428, #42341, #41297, #77527, #53315, #50919, #11282, #35691, #11521, #92030, #22967, #25327, #43370, #26802, #74400, #98357, #86611, #31816, #93068, #18290, #66587, #55858, #38574, #43517, #54823, #7404, #64943, #74406, #99261, #20105, #76821, #60176, #72501, #90650, #75121, #22835, #61316, #9712, #88164, #1153, #79602, #25185, #25388, #3291, #49287, #41970, #49469, #34444, #16477, #57489, #90122, #21728, #11969, #44047, #80568, #42149, #72130, #98806, #55977, #3214, #57884, #26035, #10837, #58994, #90339, #35358, #36277, #30046, #45237, #29380, #39356, #83196, #76850, #97778, #6347, #75185, #16188, #12459, #22362, #44240, #14614, #60905, #59431, #92409, #97555, #13703, #19161, #91692, #79726, #81200, #62861, #86538, #95153, #52183, #11692, #58402, #73952, #55664, #92152, #87058, #63015, #52636, #7349, #100372, #90035, #46395, #27159, #70070, #53711, #66427, #57533, #21677, #92850, #67119, #37162, #4024, #20410, #72061, #78988, #11764, #56448, #14712, #36338, #70184, #10254, #62907, #99919, #45537, #81103, #90454, #61701, #36826, #73375, #14335, #61463, #86666, #68176, #18072, #29186, #26118, #90129, #93630, #29061, #83455, #36720, #81520, #79992, #33227, #85801, #16209, #3192, #52019, #70039, #4128, #20718, #53919, #68264, #38351, #87500, #85536, #47255, #81979, #5084, #53, #58533, #13212, #36996, #45366, #93662, #50359, #90215, #43034, #49702, #93322, #93928, #68789, #67514, #91161, #30761, #9122, #65530, #59305, #5028, #8296, #94282, #70990, #60129, #79909, #41067, #46982, #85040, #75874, #68785, #69827, #32227, #38092, #17521, #52660, #4794, #80014, #36520, #6953, #5584, #61469, #19280, #87705, #70093, #80423, #4596, #65449, #47164, #51075, #80341, #43836, #7798, #86205, #14153, #47875, #40982, #30521, #27443, #82952, #46109, #79036, #61990, #46687, #32800, #24795, #31588, #24792, #28251, #14724, #37120, #860, #77049, #40845, #95321, #96222, #84217, #74548, #7199, #22927, #68335, #92046, #3538, #71306, #6145, #87287, #34652, #26683, #86570, #60571, #56221, #80612, #65114, #10366, #35516, #89520, #63027, #29269, #33164, #25535, #13537, #69119, #94569, #55596, #55392, #10642, #71425, #73438, #2719, #24244, #54135, #600, #62642, #7391, #17833, #34795, #90664, #93352, #54255, #46171, #94349, #16310, #47951, #31963, #19082, #9321, #34010, #22918, #38561, #37287, #54708, #69256, #58969, #95071, #61384, #20109, #76495, #551, #11398, #61951, #2975, #50232, #42639, #46479, #72624, #60742, #32598, #32254, #25784, #32468, #19020, #62147, #58778, #8629, #50377, #57160, #32244, #96136, #40030, #66709, #66703, #35466, #91283, #12101, #81380, #67606, #38003, #41524, #94332, #86710, #84418, #20217, #56346, #71550, #80234, #78413, #18405, #54205, #64558, #75996, #28632, #65765, #39790, #85770, #43944, #63801, #80582, #54985, #42238, #77, #57001, #1004, #7720, #66956, #37410, #97685, #94687, #39072, #75597, #47634, #15660, #69145, #44539, #82204, #62141, #53244, #24138, #13778, #81965, #15053, #90160, #42849, #67645, #34511, #60502, #24171, #65513, #16234, #73099, #90412, #6297, #41372, #81596, #55285, #94946, #38996, #82084, #70029, #39154, #62764, #72745, #77365, #82247, #60593, #22962, #11844, #33165, #87457, #19775, #69310, #45207, #7156, #33380, #64826, #4829, #83107, #13204, #31020, #7614, #47505, #99925, #21788, #7147, #12594, #66121, #46023, #28698, #21816, #33424, #6265, #26304, #78263, #24220, #55223, #35836, #69710, #68700, #3786, #76118, #61644, #67568, #61139, #7611, #18468, #47433, #68215, #966, #85042, #87132, #87695, #43599, #29680, #38205, #13898, #61253, #50388, #54035, #78913, #96694, #4013, #100138, #76854, #86784, #45999, #7212, #48121, #85039, #97450, #1235, #63730, #48078, #95648, #73249, #26687, #100370, #89332, #18036, #50595, #19219, #37151, #23683, #40959, #85289, #67432, #58629, #62546, #83445, #11566, #96158, #29845, #85793, #46123, #60617, #18162, #73831, #21046, #62627, #98453, #66271, #22409, #51855, #5689, #732, #25273, #2842, #12977, #66973, #63368, #17092, #29378, #46626, #79253, #74850, #47020, #53328, #95438, #62391, #1496, #70777, #6962, #36141, #86338, #19855, #70151, #36766, #10512, #64996, #87820, #81207, #68808, #33805, #15623, #27135, #5662, #15566, #22386, #71726, #60628, #33842, #70716, #9022, #31856, #44849, #28138, #31407, #66781, #5268, #80939, #2129, #65630, #8679, #89977, #75026, #2382, #86184, #27195, #28485, #42683, #33399, #69618, #59748, #27036, #45877, #26931, #99306, #2999, #41893, #39858, #32190, #2623, #63178, #68623, #99915, #74968, #88749, #42233, #87600, #39853, #13774, #41250, #24713, #98345, #81016, #71851, #59690, #23765, #33874, #99363, #64117, #65868, #19895, #66884, #42275, #3173, #38080, #79681, #90349, #76285, #67314, #96215, #4968, #38331, #55959, #68499, #59563, #13669, #7277, #52470, #40180, #61595, #39108, #34435, #45001, #73503, #22613, #55105, #14082, #4207, #25412, #59555, #26926, #30327, #41013, #84595, #5967, #6131, #76450, #67115, #82812, #57679, #94166, #93166, #19758, #7727, #65335, #71610, #99836, #53809, #33505, #63347, #3734, #2313, #62138, #81057, #99247, #36135, #99203, #76191, #91068, #78406, #47767, #55881, #71, #25459, #41078, #74934, #39043, #98904, #96890, #94800, #8192, #37196, #10718, #99482, #36400, #97781, #13667, #81640, #41787, #74444, #87489, #5327, #77866, #93294, #3735, #64289, #39244, #67323, #8449, #42472, #69884, #93505, #43533, #5470, #97094, #66462, #39868, #26771, #98949, #80021, #48298, #51620, #81968, #74185, #96561, #77834, #53306, #57792, #98576, #65193, #66642, #43620, #97156, #69113, #40981, #11780, #31337, #96290, #39487, #29791, #14146, #77819, #79088, #51334, #161, #76751, #10836, #85216, #11642, #16794, #9885, #40381, #91575, #25937, #5116, #21295, #15505, #30125, #34876, #50840, #19910, #97533, #8600, #42722, #75116, #41662, #96008, #40737, #14965, #66403, #47179, #57920, #75876, #82697, #40512, #95200, #80126, #62962, #85324, #2139, #46402, #81003, #85859, #37084, #25218, #26178, #24118, #58405, #46607, #45671, #23506, #64176, #46861, #611, #99587, #90900, #79340, #2521, #17021, #86798, #55963, #70612, #42169, #3568, #40290, #56726, #25348, #58223, #39128, #37980, #36065, #50769, #61484, #69517, #18586, #3854, #30784, #52716, #70299, #4922, #47290, #32472, #95576, #1478, #96178, #61354, #36714, #51097, #25538, #96394, #97530, #5448, #25848, #49607, #50476, #50922, #70279, #11173, #83311, #36959, #92254, #52775, #61067, #59299, #69586, #61386, #81378, #87580, #5667, #46827, #17018, #95454, #72419, #3350, #91730, #89670, #11083, #45342, #63796, #87295, #89852, #56585, #54017, #29143, #67565, #15290, #56104, #84585, #12327, #10156, #74057, #78830, #1120, #29534, #26688, #29721, #84251, #36189, #79587, #15800, #96862, #19833, #12379, #64124, #34793, #91606, #39727, #96402, #53333, #2004, #75520, #95273, #14355, #90594, #76948, #28726, #42838, #54327, #13151, #57715, #85278, #29540, #58336, #86309, #82533, #91444, #24789, #6539, #90722, #11304, #57813, #15047, #38313, #81191, #72824, #14363, #68610, #852, #6700, #5038, #36025, #20157, #98227, #27045, #81306, #93742, #6159, #82560, #78840, #32418, #70881, #39224, #41456, #42909, #35395, #52404, #30768, #54288, #57741, #94046, #30079, #33680, #83669, #57744, #90507, #49364, #1570, #47282, #98672, #25144, #97980, #46566, #89429, #35873, #92360, #33332, #58292, #43707, #96405, #1732, #86986, #4239, #91137, #72179, #68442, #31203, #69383, #23404, #16559, #80129, #11168, #9858, #99294, #47704, #23493, #48779, #39063, #29945, #80732, #77462, #65261, #58606, #18902, #47559, #4219, #7267, #25277, #58039, #87689, #53909, #51040, #18709, #16202, #31542, #98339, #17397, #88646, #21153, #97998, #96091, #74511, #14928, #35472, #8122, #89207, #69387, #76897, #98602, #66021, #36296, #89791, #69705, #71108, #73871, #55791, #35084, #52067, #54947, #75073, #61714 ) ) ;
#77602 = DIRECTION ( 'NONE',  ( 0.000000000000000000, -0.000000000000000000, -1.000000000000000000 ) ) ;
#77603 = VERTEX_POINT ( 'NONE', #82079 ) ;
#77604 = CARTESIAN_POINT ( 'NONE',  ( 2.554409723529738052, 20.22502395925995700, -1.500000000000002220 ) ) ;
#77605 = ORIENTED_EDGE ( 'NONE', *, *, #16471, .T. ) ;
#77606 = EDGE_CURVE ( 'NONE', #53605, #7384, #36147, .T. ) ;
#77607 = CARTESIAN_POINT ( 'NONE',  ( -16.20615075098634961, 16.30094363606528418, 11.49999999999998934 ) ) ;
#77608 = CARTESIAN_POINT ( 'NONE',  ( -103.5562042904834072, -23.48783264082478794, -1.443836473390061492 ) ) ;
#77609 = VERTEX_POINT ( 'NONE', #68356 ) ;
#77610 = DIRECTION ( 'NONE',  ( -1.000000000000000000, -3.773278334444166432E-23, -8.201307841325785021E-29 ) ) ;
#77611 = LINE ( 'NONE', #56697, #68019 ) ;
#77612 = EDGE_CURVE ( 'NONE', #5568, #39979, #51796, .T. ) ;
#77613 = CARTESIAN_POINT ( 'NONE',  ( -51.56793223790934633, -23.48786465467241058, 11.44779295918254824 ) ) ;
#77615 = VERTEX_POINT ( 'NONE', #6947 ) ;
#77614 = CARTESIAN_POINT ( 'NONE',  ( 16.11712757473013014, 13.99349609535929773, 11.49999999999999645 ) ) ;
#77616 = ORIENTED_EDGE ( 'NONE', *, *, #74432, .T. ) ;
#77617 = CARTESIAN_POINT ( 'NONE',  ( 13.49617185221842952, 17.62045156095830123, 11.49999999999998934 ) ) ;
#77618 = CARTESIAN_POINT ( 'NONE',  ( 14.23986175545555355, -14.96101607593195304, -1.500000000000002220 ) ) ;
#77619 = ADVANCED_FACE ( 'NONE', ( #5451 ), #23151, .T. ) ;
#77620 = ORIENTED_EDGE ( 'NONE', *, *, #95586, .F. ) ;
#77621 = ORIENTED_EDGE ( 'NONE', *, *, #55709, .F. ) ;
#77622 = CARTESIAN_POINT ( 'NONE',  ( -109.8650282762807393, -25.31627469272110531, 5.784627927385296964 ) ) ;
#77623 = CARTESIAN_POINT ( 'NONE',  ( -95.63007649029256640, -24.52399227489127398, 9.353111116836521077 ) ) ;
#77624 = EDGE_LOOP ( 'NONE', ( #82782, #74643, #38935, #66725, #34418 ) ) ;
#77625 = VECTOR ( 'NONE', #91091, 1000.000000000000227 ) ;
#77626 = CARTESIAN_POINT ( 'NONE',  ( -91.56188552897437205, -23.48783264082477018, -1.443836473390090802 ) ) ;
#77627 = VECTOR ( 'NONE', #48424, 1000.000000000000227 ) ;
#77628 = ORIENTED_EDGE ( 'NONE', *, *, #29816, .T. ) ;
#77629 = CARTESIAN_POINT ( 'NONE',  ( -58.63231504519726656, -24.35071581493543036, 9.817618358456028815 ) ) ;
#77630 = CARTESIAN_POINT ( 'NONE',  ( -44.52287095715006870, -24.33832256527048088, 0.1851278514138559594 ) ) ;
#77631 = CARTESIAN_POINT ( 'NONE',  ( -2.100290975465340271, -20.70549805216813510, -1.500000000000002220 ) ) ;
#77632 = CARTESIAN_POINT ( 'NONE',  ( -17.45706314325883213, 13.02611496694466275, 11.49999999999999645 ) ) ;
#77633 = EDGE_CURVE ( 'NONE', #57780, #94513, #35971, .T. ) ;
#77634 = DIRECTION ( 'NONE',  ( 1.000000000000000000, 3.773278334444166432E-23, 8.201307841325785021E-29 ) ) ;
#77635 = PLANE ( 'NONE',  #20728 ) ;
#77636 = CARTESIAN_POINT ( 'NONE',  ( 8.471766090126642723, -20.80389698432254519, -1.500000000000002220 ) ) ;
#77637 = VECTOR ( 'NONE', #76258, 1000.000000000000114 ) ;
#77638 = EDGE_CURVE ( 'NONE', #18516, #4528, #69942, .T. ) ;
#77639 = CARTESIAN_POINT ( 'NONE',  ( -44.58953762381671737, -24.64898659630528854, 1.056161002820819927 ) ) ;
#77640 = CARTESIAN_POINT ( 'NONE',  ( -50.52287095715006160, -23.85229601348995843, 10.88205029486208453 ) ) ;
#77641 = LINE ( 'NONE', #24367, #66995 ) ;
#77642 = AXIS2_PLACEMENT_3D ( 'NONE', #76604, #22813, #82731 ) ;
#77643 = ORIENTED_EDGE ( 'NONE', *, *, #85452, .F. ) ;
#77644 = AXIS2_PLACEMENT_3D ( 'NONE', #22311, #39054, #99441 ) ;
#77645 = ORIENTED_EDGE ( 'NONE', *, *, #66406, .F. ) ;
#77646 = EDGE_CURVE ( 'NONE', #39432, #81122, #54140, .T. ) ;
#77647 = ORIENTED_EDGE ( 'NONE', *, *, #30509, .F. ) ;
#77648 = CARTESIAN_POINT ( 'NONE',  ( -6.196366259867160942, 20.41550611124569059, -1.500000000000002220 ) ) ;
#77649 = ORIENTED_EDGE ( 'NONE', *, *, #82823, .T. ) ;
#77650 = CARTESIAN_POINT ( 'NONE',  ( -14.29351441246084065, -15.47709782942846424, 11.49999999999998934 ) ) ;
#77651 = CARTESIAN_POINT ( 'NONE',  ( 11.22434917415779054, 4.132774715458839232, -26.87660878605755599 ) ) ;
#77652 = CARTESIAN_POINT ( 'NONE',  ( -6.132916590032589710, 18.96384228413732842, -1.500000000000002220 ) ) ;
#77653 = CARTESIAN_POINT ( 'NONE',  ( -114.5895376238167245, -23.48786465467241769, 11.44779295918253936 ) ) ;
#77654 = CARTESIAN_POINT ( 'NONE',  ( -49.54749379695226708, -25.08548750068662869, 7.358461225295097385 ) ) ;
#77655 = CARTESIAN_POINT ( 'NONE',  ( -17.28599015371049674, 13.57978550619682956, -1.500000000000002220 ) ) ;
#77656 = CARTESIAN_POINT ( 'NONE',  ( -76.55620429048340725, -24.65952944569304606, 1.056160979905700126 ) ) ;
#77657 = ORIENTED_EDGE ( 'NONE', *, *, #20612, .F. ) ;
#77658 = DIRECTION ( 'NONE',  ( 0.000000000000000000, 0.9999999999976377785, 2.173523156925979975E-06 ) ) ;
#77659 = CARTESIAN_POINT ( 'NONE',  ( -54.55620429048340014, -23.47596703998600276, 11.44779298504227505 ) ) ;
#77660 = CARTESIAN_POINT ( 'NONE',  ( 20.84756458399398937, 0.1950554047328266483, 11.49999999999999645 ) ) ;
#77661 = CARTESIAN_POINT ( 'NONE',  ( 29.67519708478274865, -5.974976214603829661, 27.68766025429119537 ) ) ;
#77662 = CARTESIAN_POINT ( 'NONE',  ( -122.5228709571500616, -29.50248528299804818, 1.056150453629045360 ) ) ;
#77663 = CARTESIAN_POINT ( 'NONE',  ( -20.38992493328631284, -24.51868705080920563, 5.002395802403317049 ) ) ;
#77664 = CARTESIAN_POINT ( 'NONE',  ( 17.02398533174402218, 12.79255474601471043, -1.500000000000002220 ) ) ;
#77665 = CARTESIAN_POINT ( 'NONE',  ( -98.56083136990402238, -23.48786465467241769, 11.44779295918254469 ) ) ;
#77666 = CARTESIAN_POINT ( 'NONE',  ( 21.57151214508649772, 3.625915217019311583E-15, -1.699999999999999956 ) ) ;
#77667 = LINE ( 'NONE', #39117, #89189 ) ;
#77668 = CARTESIAN_POINT ( 'NONE',  ( -5.576843645946834016, -5.876774720514418959, 20.41272575174755133 ) ) ;
#77669 = CARTESIAN_POINT ( 'NONE',  ( -1.726696889551340153, 22.42386595106472669, -1.500000000000002220 ) ) ;
#77670 = DIRECTION ( 'NONE',  ( 1.000000000000000000, 0.000000000000000000, 0.000000000000000000 ) ) ;
#77671 = EDGE_LOOP ( 'NONE', ( #50300, #57496, #46327, #53113 ) ) ;
#77672 = DIRECTION ( 'NONE',  ( 0.000000000000000000, 0.000000000000000000, -1.000000000000000000 ) ) ;
#77673 = CARTESIAN_POINT ( 'NONE',  ( -5.193715590271882121, 18.98282465337476665, 11.49999999999999645 ) ) ;
#77674 = CARTESIAN_POINT ( 'NONE',  ( -68.62287095715002749, -23.94994826722515668, -0.6494450866351699769 ) ) ;
#77675 = FACE_OUTER_BOUND ( 'NONE', #71036, .T. ) ;
#77676 = ORIENTED_EDGE ( 'NONE', *, *, #14474, .F. ) ;
#77677 = CARTESIAN_POINT ( 'NONE',  ( -5.366453405989236813, 0.000000000000000000, 21.89999999999999858 ) ) ;
#77678 = CARTESIAN_POINT ( 'NONE',  ( -84.62287095715005592, -23.47593901973091235, -1.443836447539004642 ) ) ;
#77679 = CARTESIAN_POINT ( 'NONE',  ( -88.87267940187761894, -25.12049752546737835, 2.832404795212227100 ) ) ;
#77680 = CARTESIAN_POINT ( 'NONE',  ( -70.35718658181241381, -25.12219144531794157, 7.100646793647915622 ) ) ;
#77681 = CARTESIAN_POINT ( 'NONE',  ( 10.86211995951333620, 16.47970581058804740, -1.500000000000002220 ) ) ;
#77682 = ORIENTED_EDGE ( 'NONE', *, *, #30278, .T. ) ;
#77683 = CARTESIAN_POINT ( 'NONE',  ( 9.002841642506252740, 6.376774720514426065, -25.01329513651794656 ) ) ;
#77684 = VECTOR ( 'NONE', #97285, 1000.000000000000000 ) ;
#77685 = APPROVAL_ROLE ( '' ) ;
#77686 = ORIENTED_EDGE ( 'NONE', *, *, #97466, .F. ) ;
#77687 = DIRECTION ( 'NONE',  ( 0.000000000000000000, 0.9999999999976377785, 2.173523156925979128E-06 ) ) ;
#77688 = CARTESIAN_POINT ( 'NONE',  ( -67.62287095715005592, -23.48783264082478794, -1.443836473390067265 ) ) ;
#77689 = DIRECTION ( 'NONE',  ( 1.000000000000000000, -0.000000000000000000, -0.000000000000000000 ) ) ;
#77690 = CARTESIAN_POINT ( 'NONE',  ( -99.00488046896290939, -25.26638346776037736, 6.667019968706677346 ) ) ;
#77691 = CARTESIAN_POINT ( 'NONE',  ( 5.541369867593821219, -6.376774720514426065, 21.42815349816763160 ) ) ;
#77692 = EDGE_CURVE ( 'NONE', #48998, #6520, #72731, .T. ) ;
#77693 = PLANE ( 'NONE',  #95954 ) ;
#77694 = EDGE_CURVE ( 'NONE', #75484, #21744, #93171, .T. ) ;
#77695 = CARTESIAN_POINT ( 'NONE',  ( -30.30597055170165888, -23.44955593248640824, -1.443836447538997314 ) ) ;
#77696 = CARTESIAN_POINT ( 'NONE',  ( -18.86779840422491716, -6.689013621249945807, -1.500000000000002220 ) ) ;
#77697 = EDGE_CURVE ( 'NONE', #99971, #47988, #58825, .T. ) ;
#77698 = CARTESIAN_POINT ( 'NONE',  ( -99.21726371882367346, -25.27533020790543361, 3.564824879032668203 ) ) ;
#77699 = DIRECTION ( 'NONE',  ( -0.8264557562326033668, -6.845827386180409975E-16, -0.5630016722799281448 ) ) ;
#77700 = VERTEX_POINT ( 'NONE', #23660 ) ;
#77701 = VECTOR ( 'NONE', #85520, 1000.000000000000000 ) ;
#77702 = EDGE_CURVE ( 'NONE', #65722, #73093, #8113, .T. ) ;
#77703 = VECTOR ( 'NONE', #30575, 1000.000000000000114 ) ;
#77704 = CARTESIAN_POINT ( 'NONE',  ( -79.62649533826925108, -24.51419770103157347, 9.386484678747176957 ) ) ;
#77705 = CARTESIAN_POINT ( 'NONE',  ( -109.5745106736623029, -25.29012798628001946, 3.630693211477457716 ) ) ;
#77706 = CARTESIAN_POINT ( 'NONE',  ( -34.62287095715005592, -23.48786465467240347, 11.44779295918255535 ) ) ;
#77707 = CARTESIAN_POINT ( 'NONE',  ( -92.52287095715006160, -23.48783264083452593, -1.443836473374927820 ) ) ;
#77708 = VECTOR ( 'NONE', #25070, 1000.000000000000000 ) ;
#77709 = CARTESIAN_POINT ( 'NONE',  ( -116.6623340026854692, -25.38352273315421925, 4.245316684715564115 ) ) ;
#77710 = CARTESIAN_POINT ( 'NONE',  ( -54.62287095715005592, -24.65952944569304606, 1.056160979905694131 ) ) ;
#77711 = AXIS2_PLACEMENT_3D ( 'NONE', #39716, #17893, #1169 ) ;
#77712 = CARTESIAN_POINT ( 'NONE',  ( -3.071531057816138333, -5.876774720514414518, 19.86545874326175110 ) ) ;
#77713 = EDGE_CURVE ( 'NONE', #94877, #25496, #18432, .T. ) ;
#77714 = CARTESIAN_POINT ( 'NONE',  ( 5.326923076923078426, -5.876774720514419847, 20.76772836538461320 ) ) ;
#77715 = VERTEX_POINT ( 'NONE', #53642 ) ;
#77716 = CARTESIAN_POINT ( 'NONE',  ( 17.44645523915803764, -10.38078700900905993, -1.500000000000002220 ) ) ;
#77717 = CARTESIAN_POINT ( 'NONE',  ( 31.63608488009066733, 3.316774720514426456, 27.34773273846990804 ) ) ;
#77718 = CARTESIAN_POINT ( 'NONE',  ( -39.56136241089613748, -25.30385213834873781, 5.536731319770037629 ) ) ;
#77719 = ORIENTED_EDGE ( 'NONE', *, *, #78191, .T. ) ;
#77720 = CARTESIAN_POINT ( 'NONE',  ( -83.55620429048339304, -23.48786465467241058, 11.44779295918254469 ) ) ;
#77721 = CARTESIAN_POINT ( 'NONE',  ( 1.236116150138429903, -20.07036509671028668, -1.500000000000002220 ) ) ;
#77722 = CARTESIAN_POINT ( 'NONE',  ( 17.90021246794804810, -11.17811638239879279, 11.49999999999999645 ) ) ;
#77723 = CARTESIAN_POINT ( 'NONE',  ( -21.04927197579530329, -6.814310187297170529, 11.49999999999998934 ) ) ;
#77724 = CARTESIAN_POINT ( 'NONE',  ( 7.506095096478735407, 19.11734572241606145, -1.500000000000002220 ) ) ;
#77725 = LINE ( 'NONE', #77225, #95614 ) ;
#77726 = EDGE_LOOP ( 'NONE', ( #47488, #77867, #35150, #12851 ) ) ;
#77727 = CARTESIAN_POINT ( 'NONE',  ( -88.58953762381671027, -23.47596703998600631, 11.44779298504227683 ) ) ;
#77728 = ORIENTED_EDGE ( 'NONE', *, *, #98783, .F. ) ;
#77729 = CARTESIAN_POINT ( 'NONE',  ( -88.62287095715004170, -24.64965695001469115, 8.947790433994180503 ) ) ;
#77730 = CARTESIAN_POINT ( 'NONE',  ( -80.55620429048339304, -23.47593901973091235, -1.443836447539004642 ) ) ;
#77731 = EDGE_LOOP ( 'NONE', ( #5198, #55181, #67288, #98981 ) ) ;
#77732 = ORIENTED_EDGE ( 'NONE', *, *, #3194, .T. ) ;
#77733 = ORIENTED_EDGE ( 'NONE', *, *, #59058, .T. ) ;
#77734 = LINE ( 'NONE', #16350, #76178 ) ;
#77735 = CARTESIAN_POINT ( 'NONE',  ( -50.29668966358368465, -25.03348023436011260, 7.560224540057909337 ) ) ;
#77736 = CARTESIAN_POINT ( 'NONE',  ( -68.58780896930441884, -24.35071581493542681, 9.817618358456032368 ) ) ;
#77737 = CARTESIAN_POINT ( 'NONE',  ( 17.27521350410721368, -11.31798593588896829, -1.500000000000002220 ) ) ;
#77738 = CARTESIAN_POINT ( 'NONE',  ( -18.67883320684159543, -10.89015303950203517, 11.49999999999999645 ) ) ;
#77739 = EDGE_LOOP ( 'NONE', ( #21852, #34455, #11129, #16236 ) ) ;
#77740 = DIRECTION ( 'NONE',  ( 1.232047923278981953E-16, -1.000000000000000000, 0.000000000000000000 ) ) ;
#77741 = CARTESIAN_POINT ( 'NONE',  ( -96.52287095715006160, -24.64965694238575011, 8.947790433994194714 ) ) ;
#77742 = CARTESIAN_POINT ( 'NONE',  ( -3.695635658436464244, 22.08213133993951161, 11.49999999999998934 ) ) ;
#77743 = EDGE_CURVE ( 'NONE', #99569, #44562, #46941, .T. ) ;
#77744 = CARTESIAN_POINT ( 'NONE',  ( -67.52287095715006160, -23.47596703998600631, 11.44779298504228748 ) ) ;
#77745 = LINE ( 'NONE', #62055, #56260 ) ;
#77746 = VERTEX_POINT ( 'NONE', #10319 ) ;
#77747 = CARTESIAN_POINT ( 'NONE',  ( -100.3670236477657056, -25.31212503800871971, 4.712017573479897692 ) ) ;
#77748 = CARTESIAN_POINT ( 'NONE',  ( -35.60239790912048363, -24.15602025860895452, 10.28564288303536856 ) ) ;
#77749 = CARTESIAN_POINT ( 'NONE',  ( -17.98194200498208062, 10.70670730041394947, -1.500000000000002220 ) ) ;
#77750 = ORIENTED_EDGE ( 'NONE', *, *, #35399, .T. ) ;
#77752 = ADVANCED_FACE ( 'NONE', ( #30786 ), #92673, .T. ) ;
#77751 = VECTOR ( 'NONE', #5749, 1000.000000000000000 ) ;
#77753 = DIRECTION ( 'NONE',  ( 0.000000000000000000, -2.173523156925979552E-06, 0.9999999999976378895 ) ) ;
#77754 = VERTEX_POINT ( 'NONE', #7439 ) ;
#77755 = LINE ( 'NONE', #15367, #95749 ) ;
#77756 = CARTESIAN_POINT ( 'NONE',  ( 20.45381123341165619, -5.387677532796200097, -1.500000000000002220 ) ) ;
#77757 = VERTEX_POINT ( 'NONE', #13299 ) ;
#77758 = CARTESIAN_POINT ( 'NONE',  ( -50.57159316625579493, -23.48783264082477018, -1.443836473390096797 ) ) ;
#77759 = CARTESIAN_POINT ( 'NONE',  ( -0.2038501785326352067, 21.78777694363981254, 11.49999999999998934 ) ) ;
#77760 = DIRECTION ( 'NONE',  ( -1.000000000000000000, 0.000000000000000000, 0.000000000000000000 ) ) ;
#77761 = VECTOR ( 'NONE', #11862, 1000.000000000000000 ) ;
#77762 = DIRECTION ( 'NONE',  ( -0.000000000000000000, -1.000000000000000000, -0.000000000000000000 ) ) ;
#77763 = CARTESIAN_POINT ( 'NONE',  ( -75.55620429048340725, -25.00158670708909625, 2.256160236439166855 ) ) ;
#77764 = CARTESIAN_POINT ( 'NONE',  ( -3.523925741820590929, 21.50064390955241578, -1.500000000000002220 ) ) ;
#77765 = CARTESIAN_POINT ( 'NONE',  ( 6.480733632922428988, -6.376774720514426065, 21.47849199606610782 ) ) ;
#77766 = ORIENTED_EDGE ( 'NONE', *, *, #34693, .F. ) ;
#77767 = CARTESIAN_POINT ( 'NONE',  ( 7.275731542451676859, -5.876774720514415407, 20.06332870126568224 ) ) ;
#77768 = LINE ( 'NONE', #30613, #36263 ) ;
#77769 = ORIENTED_EDGE ( 'NONE', *, *, #67020, .F. ) ;
#77770 = AXIS2_PLACEMENT_3D ( 'NONE', #88856, #19321, #50292 ) ;
#77771 = AXIS2_PLACEMENT_3D ( 'NONE', #1757, #32694, #41832 ) ;
#77772 = EDGE_LOOP ( 'NONE', ( #71887, #83005, #17379, #42080 ) ) ;
#77773 = EDGE_LOOP ( 'NONE', ( #28837, #91360, #70159, #81483 ) ) ;
#77774 = CARTESIAN_POINT ( 'NONE',  ( -23.59123376470063960, -5.356774720514425603, 23.50402280011862288 ) ) ;
#77775 = AXIS2_PLACEMENT_3D ( 'NONE', #75724, #19455, #44806 ) ;
#77776 = CARTESIAN_POINT ( 'NONE',  ( -63.55620429048339304, -23.48783264082478084, -1.443836473390068820 ) ) ;
#77777 = CARTESIAN_POINT ( 'NONE',  ( 21.18767802922067034, -0.7184367399587067160, 11.49999999999998934 ) ) ;
#77778 = CARTESIAN_POINT ( 'NONE',  ( -125.5562042904833930, -23.47593901973091235, -1.443836447538995760 ) ) ;
#77779 = CARTESIAN_POINT ( 'NONE',  ( -95.62287095715002749, -24.91570333823099759, 8.075032458375547506 ) ) ;
#77780 = CARTESIAN_POINT ( 'NONE',  ( -81.62287095715005592, -29.50248528299804818, 1.056150453629038477 ) ) ;
#77782 = DIRECTION ( 'NONE',  ( 0.000000000000000000, 0.000000000000000000, -1.000000000000000000 ) ) ;
#77781 = B_SPLINE_CURVE_WITH_KNOTS ( 'NONE', 3,
 ( #62833, #47597, #9519, #93749 ),
 .UNSPECIFIED., .F., .F.,
 ( 4, 4 ),
 ( 0.7893427479188557250, 0.7903434949596209735 ),
 .UNSPECIFIED. ) ;
#77783 = AXIS2_PLACEMENT_3D ( 'NONE', #18407, #2694, #33637 ) ;
#77784 = CARTESIAN_POINT ( 'NONE',  ( 11.20917403917954225, 15.81763734437701885, -1.500000000000002220 ) ) ;
#77785 = CARTESIAN_POINT ( 'NONE',  ( -51.93149462243455616, -25.25905089634592571, 6.174051128686508072 ) ) ;
#77786 = VERTEX_POINT ( 'NONE', #96061 ) ;
#77787 = AXIS2_PLACEMENT_3D ( 'NONE', #43522, #11555, #56764 ) ;
#77788 = CARTESIAN_POINT ( 'NONE',  ( 19.43689267596983683, 0.5339526363925560792, 11.49999999999999645 ) ) ;
#77789 = FACE_OUTER_BOUND ( 'NONE', #68058, .T. ) ;
#77790 = PLANE ( 'NONE',  #65766 ) ;
#77791 = ORIENTED_EDGE ( 'NONE', *, *, #21737, .T. ) ;
#77792 = CARTESIAN_POINT ( 'NONE',  ( 4.885870204371583370, -6.376774720514420736, 20.85936027411790405 ) ) ;
#77793 = DIRECTION ( 'NONE',  ( 0.9975640502598243087, -0.06975647374412546897, -0.000000000000000000 ) ) ;
#77794 = CARTESIAN_POINT ( 'NONE',  ( -64.62287095715005592, -24.64898659630528499, 1.056161002820822592 ) ) ;
#77795 = CARTESIAN_POINT ( 'NONE',  ( -93.62566436713133555, -24.51419770103157703, 9.386484678747164523 ) ) ;
#77796 = CARTESIAN_POINT ( 'NONE',  ( 14.19269941865516671, -13.59168563846684563, 11.49999999999998934 ) ) ;
#77797 = DIRECTION ( 'NONE',  ( 0.000000000000000000, 0.000000000000000000, -1.000000000000000000 ) ) ;
#77798 = ORIENTED_EDGE ( 'NONE', *, *, #29148, .F. ) ;
#77799 = CARTESIAN_POINT ( 'NONE',  ( 20.63042821663210091, 6.393326493806346100, 11.49999999999998934 ) ) ;
#77800 = CARTESIAN_POINT ( 'NONE',  ( 8.971512145086499856, -0.9999999999999991118, 3.746884140868835367 ) ) ;
#77801 = CARTESIAN_POINT ( 'NONE',  ( -9.299999999999991829, 12.00000000000002309, 0.000000000000000000 ) ) ;
#77802 = CARTESIAN_POINT ( 'NONE',  ( -21.75560140871883164, 7.562747417745157463, -1.500000000000002220 ) ) ;
#77803 = PERSON_AND_ORGANIZATION_ROLE ( 'classification_officer' ) ;
#77804 = CARTESIAN_POINT ( 'NONE',  ( -55.92287095715006018, -23.47596703998600631, 11.44779298504227683 ) ) ;
#77805 = DIRECTION ( 'NONE',  ( 1.000000000000000000, 3.773278334444166432E-23, 8.201307841325785021E-29 ) ) ;
#77806 = CARTESIAN_POINT ( 'NONE',  ( -43.62287095715004881, -29.50248528299804818, 1.056150453629031594 ) ) ;
#77807 = CARTESIAN_POINT ( 'NONE',  ( -64.62287095715005592, -23.73934037231756733, 11.05740245334329153 ) ) ;
#77808 = EDGE_CURVE ( 'NONE', #49731, #7781, #57516, .T. ) ;
#77809 = CARTESIAN_POINT ( 'NONE',  ( -111.7736932848194726, -25.10921665464774577, 4.173604445294007093 ) ) ;
#77810 = DIRECTION ( 'NONE',  ( 0.000000000000000000, -0.000000000000000000, -1.000000000000000000 ) ) ;
#77811 = CARTESIAN_POINT ( 'NONE',  ( -99.32787325113280019, -25.26400820985182705, 4.639922590201173591 ) ) ;
#77812 = CARTESIAN_POINT ( 'NONE',  ( 2.793900936927258272, 19.68708943014846469, -1.500000000000002220 ) ) ;
#77813 = B_SPLINE_CURVE_WITH_KNOTS ( 'NONE', 3,
 ( #72245, #96562, #98937, #65155 ),
 .UNSPECIFIED., .F., .F.,
 ( 4, 4 ),
 ( 0.000000000000000000, 9.999999999997510880E-05 ),
 .UNSPECIFIED. ) ;
#77814 = EDGE_CURVE ( 'NONE', #67032, #46870, #23924, .T. ) ;
#77815 = CARTESIAN_POINT ( 'NONE',  ( -72.62287095715005592, -23.47596703998600631, 11.44779298504227860 ) ) ;
#77816 = CARTESIAN_POINT ( 'NONE',  ( 9.833179757865110560, 17.22857952739193266, -1.500000000000002220 ) ) ;
#77817 = CARTESIAN_POINT ( 'NONE',  ( -94.62287095715005592, -24.66019654487199730, 8.947790411086126383 ) ) ;
#77818 = EDGE_CURVE ( 'NONE', #71054, #39828, #66136, .T. ) ;
#77819 = ADVANCED_FACE ( 'NONE', ( #11324 ), #530, .T. ) ;
#77820 = CARTESIAN_POINT ( 'NONE',  ( -108.5228709571500616, -24.64898659630528854, 1.056161002820831474 ) ) ;
#77821 = B_SPLINE_CURVE_WITH_KNOTS ( 'NONE', 3,
 ( #21012, #4807, #51982, #12402, #96645, #27145, #66731, #97153, #82910, #97642, #19518, #83410 ),
 .UNSPECIFIED., .F., .F.,
 ( 4, 2, 2, 2, 2, 4 ),
 ( 0.000000000000000000, 0.0002976555682062342022, 0.0005953111364124684043, 0.0008929667046187024981, 0.001041794488721820792, 0.001190622272824939194 ),
 .UNSPECIFIED. ) ;
#77822 = CARTESIAN_POINT ( 'NONE',  ( 11.98973536156539943, -2.682774720514426559, -26.26140391504922178 ) ) ;
#77823 = CARTESIAN_POINT ( 'NONE',  ( 8.872108392497455753, -18.76566404461018678, 11.49999999999999645 ) ) ;
#77824 = CARTESIAN_POINT ( 'NONE',  ( -7.640476926272304681, -5.876774720514415407, 20.25188360057253689 ) ) ;
#77825 = EDGE_CURVE ( 'NONE', #86594, #60374, #15283, .T. ) ;
#77826 = VECTOR ( 'NONE', #9385, 1000.000000000000114 ) ;
#77827 = CARTESIAN_POINT ( 'NONE',  ( -106.5141348546935802, -24.34968618360934300, 0.1864209137778878034 ) ) ;
#77828 = CARTESIAN_POINT ( 'NONE',  ( 20.43669262517703800, -10.12641136740851699, 11.49999999999999645 ) ) ;
#77829 = ORIENTED_EDGE ( 'NONE', *, *, #58109, .T. ) ;
#77830 = CARTESIAN_POINT ( 'NONE',  ( -69.62363796276726191, -24.65952944569304606, 1.056160979905704567 ) ) ;
#77831 = CARTESIAN_POINT ( 'NONE',  ( -69.55367693329765189, -25.17615986935216199, 6.773585123431198340 ) ) ;
#77832 = VERTEX_POINT ( 'NONE', #3722 ) ;
#77833 = CARTESIAN_POINT ( 'NONE',  ( 19.32837167043147986, -5.866312143582237404, 11.49999999999998934 ) ) ;
#77834 = ADVANCED_FACE ( 'NONE', ( #4711 ), #58015, .F. ) ;
#77835 = CARTESIAN_POINT ( 'NONE',  ( 9.045337356650575700, -0.9026027323331682339, -3.697389739420774646 ) ) ;
#77836 = DIRECTION ( 'NONE',  ( 0.000000000000000000, -1.000000000000000000, 0.000000000000000000 ) ) ;
#77837 = ORIENTED_EDGE ( 'NONE', *, *, #67672, .F. ) ;
#77838 = VERTEX_POINT ( 'NONE', #88948 ) ;
#77839 = DIRECTION ( 'NONE',  ( -0.000000000000000000, -1.000000000000000000, -0.000000000000000000 ) ) ;
#77840 = CARTESIAN_POINT ( 'NONE',  ( -7.509321099650855480, 21.62252279970214985, 11.49999999999998934 ) ) ;
#77841 = FACE_OUTER_BOUND ( 'NONE', #77234, .T. ) ;
#77842 = AXIS2_PLACEMENT_3D ( 'NONE', #88432, #88932, #56994 ) ;
#77843 = CARTESIAN_POINT ( 'NONE',  ( -21.57582672592670292, -1.461774377805347802, -1.500000000000002220 ) ) ;
#77844 = CARTESIAN_POINT ( 'NONE',  ( 282.9764569301858046, -4.540774720514427543, 20.79159422840526616 ) ) ;
#77845 = CARTESIAN_POINT ( 'NONE',  ( -10.06633388967972209, 18.29571535785830960, 11.49999999999999645 ) ) ;
#77846 = EDGE_LOOP ( 'NONE', ( #87321, #72792, #74654, #66345 ) ) ;
#77847 = VECTOR ( 'NONE', #27977, 1000.000000000000114 ) ;
#77848 = CARTESIAN_POINT ( 'NONE',  ( -122.6228709571500417, -24.66019654487199730, 8.947790411086121054 ) ) ;
#77849 = CARTESIAN_POINT ( 'NONE',  ( -107.5228709571501042, -23.47593901973090524, -1.443836447538996426 ) ) ;
#77850 = CARTESIAN_POINT ( 'NONE',  ( -2.093881351098874521, -21.91542971883435698, 11.49999999999998934 ) ) ;
#77852 = DIRECTION ( 'NONE',  ( -0.1736481776669262789, -0.9848077530122087975, 0.000000000000000000 ) ) ;
#77851 = CIRCLE ( 'NONE', #87593, 1.699999999999999289 ) ;
#77853 = CARTESIAN_POINT ( 'NONE',  ( -65.62287095715005592, -23.47596703998600631, 11.44779298504227683 ) ) ;
#77854 = ORIENTED_EDGE ( 'NONE', *, *, #70914, .T. ) ;
#77855 = DIRECTION ( 'NONE',  ( -0.000000000000000000, -1.000000000000000000, -0.000000000000000000 ) ) ;
#77856 = CARTESIAN_POINT ( 'NONE',  ( -85.62287095715005592, -23.47593901973091235, -1.443836447539002865 ) ) ;
#77857 = EDGE_LOOP ( 'NONE', ( #25563, #97138, #52314, #95099 ) ) ;
#77858 = LINE ( 'NONE', #22567, #71290 ) ;
#77859 = B_SPLINE_CURVE_WITH_KNOTS ( 'NONE', 3,
 ( #9434, #34289, #18052, #24652, #57139, #48014 ),
 .UNSPECIFIED., .F., .F.,
 ( 4, 2, 4 ),
 ( 1.570755371633875854E-05, 0.001396183895866086235, 0.002776660238015833410 ),
 .UNSPECIFIED. ) ;
#77860 = ORIENTED_EDGE ( 'NONE', *, *, #81154, .F. ) ;
#77861 = EDGE_LOOP ( 'NONE', ( #66274, #23038, #27642, #87548 ) ) ;
#77862 = CARTESIAN_POINT ( 'NONE',  ( -71.49851612826357439, -24.51419770103159124, 9.386484678747166299 ) ) ;
#77863 = CARTESIAN_POINT ( 'NONE',  ( -101.3783285514244028, -25.10935884294595866, 3.208886314311354848 ) ) ;
#77864 = CARTESIAN_POINT ( 'NONE',  ( -100.5228709571500900, -23.84081130425357387, 10.88220057483161085 ) ) ;
#77865 = CARTESIAN_POINT ( 'NONE',  ( -2.750569593922542300, -20.27526743851804625, -1.500000000000002220 ) ) ;
#77866 = ADVANCED_FACE ( 'NONE', ( #19428 ), #71055, .T. ) ;
#77867 = ORIENTED_EDGE ( 'NONE', *, *, #6016, .F. ) ;
#77868 = CARTESIAN_POINT ( 'NONE',  ( -100.0587518433314784, -25.30258194450249931, 5.273723563230666933 ) ) ;
#77869 = CARTESIAN_POINT ( 'NONE',  ( -44.66287493451820012, -23.48783264082476663, -1.443836473390094799 ) ) ;
#77870 = DIRECTION ( 'NONE',  ( 1.000000000000000000, 0.000000000000000000, 0.000000000000000000 ) ) ;
#77871 = CARTESIAN_POINT ( 'NONE',  ( -22.23078454666273274, -1.437644496696519170, -1.500000000000002220 ) ) ;
#77872 = ADVANCED_FACE ( 'NONE', ( #60509 ), #7188, .T. ) ;
#77873 = CARTESIAN_POINT ( 'NONE',  ( -55.52287095715004028, -24.52323809116984066, 9.355190652339430812 ) ) ;
#77874 = CARTESIAN_POINT ( 'NONE',  ( -1.380763273332680896, -5.876774720514418071, 20.28973052848695602 ) ) ;
#77875 = ORIENTED_EDGE ( 'NONE', *, *, #82922, .T. ) ;
#77876 = CARTESIAN_POINT ( 'NONE',  ( -44.52287095715004739, -23.48783264082477018, -1.443836473390094577 ) ) ;
#77877 = CARTESIAN_POINT ( 'NONE',  ( -118.6228709571500559, -29.50248528299804818, 1.056150453629045360 ) ) ;
#77878 = CARTESIAN_POINT ( 'NONE',  ( 12.46380520747237419, 16.70348211664046900, 11.49999999999998934 ) ) ;
#77879 = EDGE_LOOP ( 'NONE', ( #56657, #68193, #72456, #49951 ) ) ;
#77881 = ORIENTED_EDGE ( 'NONE', *, *, #39916, .F. ) ;
#77880 = DIRECTION ( 'NONE',  ( 0.1827036106964188555, 0.000000000000000000, -0.9831680378442393398 ) ) ;
#77882 = ORIENTED_EDGE ( 'NONE', *, *, #89457, .T. ) ;
#77883 = CARTESIAN_POINT ( 'NONE',  ( -58.52287095715006160, -24.50321055353803601, 9.387540953477515160 ) ) ;
#77884 = CARTESIAN_POINT ( 'NONE',  ( 14.98681507544721292, -14.71779577663021321, -1.500000000000002220 ) ) ;
#77885 = EDGE_CURVE ( 'NONE', #503, #8654, #23737, .T. ) ;
#77886 = ORIENTED_EDGE ( 'NONE', *, *, #84341, .F. ) ;
#77887 = CARTESIAN_POINT ( 'NONE',  ( -90.52287095715006160, -24.99132157543165889, 2.256160258750667502 ) ) ;
#77888 = CARTESIAN_POINT ( 'NONE',  ( -50.38191529551148307, -25.10935757153401937, 2.832404819425170306 ) ) ;
#77889 = LINE ( 'NONE', #22600, #23784 ) ;
#77890 = CARTESIAN_POINT ( 'NONE',  ( -49.52287095715006160, -29.50250243563736774, 8.947779886222146928 ) ) ;
#77891 = PLANE ( 'NONE',  #67581 ) ;
#77892 = FACE_OUTER_BOUND ( 'NONE', #3427, .T. ) ;
#77894 = VERTEX_POINT ( 'NONE', #60996 ) ;
#77893 = CARTESIAN_POINT ( 'NONE',  ( -12.04397493737346991, 18.63154960201688226, 11.49999999999999645 ) ) ;
#77895 = DIRECTION ( 'NONE',  ( -3.773278334453079618E-23, 0.9999999999976377785, 2.173523156925979975E-06 ) ) ;
#77896 = EDGE_CURVE ( 'NONE', #95483, #477, #63655, .T. ) ;
#77897 = CARTESIAN_POINT ( 'NONE',  ( 8.978253834636468866, -6.376774720514426953, 18.51871304725684553 ) ) ;
#77898 = ORIENTED_EDGE ( 'NONE', *, *, #45291, .F. ) ;
#77899 = CARTESIAN_POINT ( 'NONE',  ( -21.51096707683950626, -7.176001652309477841, -1.500000000000002220 ) ) ;
#77901 = VERTEX_POINT ( 'NONE', #22894 ) ;
#77900 = CARTESIAN_POINT ( 'NONE',  ( -111.5228709571499763, -23.73934037231757443, 11.05740245334327909 ) ) ;
#77902 = EDGE_LOOP ( 'NONE', ( #83608, #11279, #52698, #81621 ) ) ;
#77903 = LINE ( 'NONE', #8410, #32059 ) ;
#77904 = AXIS2_PLACEMENT_3D ( 'NONE', #69794, #60199, #6398 ) ;
#77905 = CC_DESIGN_DATE_AND_TIME_ASSIGNMENT ( #75202, #62491, ( #92779 ) ) ;
#77906 = CARTESIAN_POINT ( 'NONE',  ( 13.66866334921533799, -14.80927461459226890, 11.49999999999998934 ) ) ;
#77907 = LINE ( 'NONE', #46984, #2003 ) ;
#77908 = VERTEX_POINT ( 'NONE', #44773 ) ;
#77909 = DIRECTION ( 'NONE',  ( 0.000000000000000000, -2.173523156925979552E-06, 0.9999999999976378895 ) ) ;
#77910 = CARTESIAN_POINT ( 'NONE',  ( 7.974090105135403839, 20.87195307945309963, -1.500000000000002220 ) ) ;
#77911 = ORIENTED_EDGE ( 'NONE', *, *, #1189, .F. ) ;
#77912 = CARTESIAN_POINT ( 'NONE',  ( -104.5118022433312461, -24.51314013834316086, 0.6176544820404171743 ) ) ;
#77913 = CARTESIAN_POINT ( 'NONE',  ( -101.2523990460597503, -25.25341228077052946, 6.807413982353327064 ) ) ;
#77914 = DIRECTION ( 'NONE',  ( -1.000000000000000000, -3.773278334444166432E-23, -8.201307841325785021E-29 ) ) ;
#77915 = LINE ( 'NONE', #53117, #63544 ) ;
#77916 = CARTESIAN_POINT ( 'NONE',  ( -38.62287095715005592, -24.65952944569303895, 1.056160979905692798 ) ) ;
#77917 = CARTESIAN_POINT ( 'NONE',  ( -130.5728709571500588, -24.37807914296826084, 0.3010598746230577771 ) ) ;
#77918 = AXIS2_PLACEMENT_3D ( 'NONE', #54127, #85051, #77427 ) ;
#77919 = CARTESIAN_POINT ( 'NONE',  ( -9.112395119859147741, -17.30902560603237106, 11.49999999999998934 ) ) ;
#77920 = CARTESIAN_POINT ( 'NONE',  ( -32.30247028140506416, 1.684774720514426560, 27.60502002861223048 ) ) ;
#77921 = CARTESIAN_POINT ( 'NONE',  ( 21.44729954461699251, -1.519088741117538000, 11.49999999999998934 ) ) ;
#77922 = CARTESIAN_POINT ( 'NONE',  ( -95.62287095715005592, -23.47596703998600631, 11.44779298504227860 ) ) ;
#77923 = DIRECTION ( 'NONE',  ( 0.000000000000000000, 0.9961946980917452121, -0.08715574274766166307 ) ) ;
#77924 = CARTESIAN_POINT ( 'NONE',  ( -7.641025641025638748, -6.376774720514427841, 21.75000000000001066 ) ) ;
#77925 = CARTESIAN_POINT ( 'NONE',  ( 15.00000000000000533, 2.939152317953647894E-15, -24.00000000000000000 ) ) ;
#77926 = CARTESIAN_POINT ( 'NONE',  ( -22.79553223295561892, 1.966428799096173075, -1.500000000000002220 ) ) ;
#77927 = SECURITY_CLASSIFICATION_LEVEL ( 'unclassified' ) ;
#77928 = CARTESIAN_POINT ( 'NONE',  ( 26.14999174255633463, 4.132774720517320866, -11.56127575336603286 ) ) ;
#77929 = CARTESIAN_POINT ( 'NONE',  ( -53.65126712112351015, -23.73766607897669090, -1.055555164236459564 ) ) ;
#77930 = CARTESIAN_POINT ( 'NONE',  ( -5.935188749463110369, 19.13178230186815298, 11.49999999999999645 ) ) ;
#77931 = CARTESIAN_POINT ( 'NONE',  ( -99.62287095715005592, -23.47593901973091235, -1.443836447539001089 ) ) ;
#77932 = LINE ( 'NONE', #56137, #3111 ) ;
#77933 = CARTESIAN_POINT ( 'NONE',  ( 13.91401389203221406, 5.965225279485572685, 27.75920385068456042 ) ) ;
#77934 = CARTESIAN_POINT ( 'NONE',  ( 1.175186991919851431, 0.3587747205144265483, 28.89597625626659649 ) ) ;
#77935 = ADVANCED_FACE ( 'NONE', ( #38139 ), #44263, .T. ) ;
#77936 = ORIENTED_EDGE ( 'NONE', *, *, #17456, .F. ) ;
#77937 = CARTESIAN_POINT ( 'NONE',  ( -33.62287095715005592, -24.66019654487199020, 8.947790411086138818 ) ) ;
#77938 = CARTESIAN_POINT ( 'NONE',  ( -7.892909027492730267, -20.28523913882780505, 11.49999999999998934 ) ) ;
#77939 = DIRECTION ( 'NONE',  ( -3.773278334444167608E-23, 1.000000000000000000, 0.000000000000000000 ) ) ;
#77940 = CARTESIAN_POINT ( 'NONE',  ( -14.15603575923578283, -13.64839490926926580, -1.500000000000002220 ) ) ;
#77941 = CARTESIAN_POINT ( 'NONE',  ( -38.62287095715005592, -23.48786465467240703, 11.44779295918255180 ) ) ;
#77942 = CARTESIAN_POINT ( 'NONE',  ( -110.0852742341990904, -25.27925937390634914, 5.455857480927421399 ) ) ;
#77943 = DATE_AND_TIME ( #97803, #32900 ) ;
#77944 = EDGE_CURVE ( 'NONE', #73404, #49834, #53386, .T. ) ;
#77945 = CARTESIAN_POINT ( 'NONE',  ( -91.64133805002603594, -23.48786465467241058, 11.44779295918254469 ) ) ;
#77946 = DIRECTION ( 'NONE',  ( 7.109281096390894329E-15, 0.000000000000000000, 1.000000000000000000 ) ) ;
#77947 = CARTESIAN_POINT ( 'NONE',  ( 15.21836549854886123, 13.79734045396011943, 11.49999999999999645 ) ) ;
#77948 = DIRECTION ( 'NONE',  ( -0.000000000000000000, -1.000000000000000000, -0.000000000000000000 ) ) ;
#77949 = EDGE_CURVE ( 'NONE', #68153, #98254, #6197, .T. ) ;
#77950 = CARTESIAN_POINT ( 'NONE',  ( -8.978253834636468866, -5.876774720514426953, 0.000000000000000000 ) ) ;
#77951 = CARTESIAN_POINT ( 'NONE',  ( -22.11960324842224423, 4.537628740662121629, 11.49999999999999645 ) ) ;
#77952 = ORIENTED_EDGE ( 'NONE', *, *, #77273, .F. ) ;
#77953 = CARTESIAN_POINT ( 'NONE',  ( -99.65355524409876864, -25.26387372658618347, 4.362766323930155288 ) ) ;
#77954 = CARTESIAN_POINT ( 'NONE',  ( -27.37821967320581251, -24.79341979850518385, 7.571465340039231329 ) ) ;
#77955 = CARTESIAN_POINT ( 'NONE',  ( -125.5569696030716926, -23.48786465467241769, 11.44779295918253581 ) ) ;
#77956 = CARTESIAN_POINT ( 'NONE',  ( 14.98380649186719538, -3.494980989714896680, -27.33501059067317485 ) ) ;
#77957 = EDGE_CURVE ( 'NONE', #24998, #48069, #86408, .T. ) ;
#77958 = CARTESIAN_POINT ( 'NONE',  ( -26.25023971703978276, -24.93063488596019539, 7.578546381800906673 ) ) ;
#77959 = CARTESIAN_POINT ( 'NONE',  ( 32.70752563734568952, 3.536205085657706082, -3.307643893017725212 ) ) ;
#77960 = ORIENTED_EDGE ( 'NONE', *, *, #86998, .F. ) ;
#77961 = CARTESIAN_POINT ( 'NONE',  ( -18.27982475084466785, -14.08179083545084964, 11.49999999999999645 ) ) ;
#77962 = CARTESIAN_POINT ( 'NONE',  ( 16.42120958226126604, -15.83219868413775622, 11.49999999999998934 ) ) ;
#77963 = CARTESIAN_POINT ( 'NONE',  ( -104.5228709571500758, -23.47593901973090524, -1.443836447538996204 ) ) ;
#77964 = CARTESIAN_POINT ( 'NONE',  ( -5.596556251055551101, -6.376774720514411854, 19.35667676486397681 ) ) ;
#77965 = DIRECTION ( 'NONE',  ( -0.9762960071199348056, -0.2164396139380966033, 6.123031769111886291E-17 ) ) ;
#77966 = CARTESIAN_POINT ( 'NONE',  ( 22.01961411883556252, 4.383451955130949429, 11.49999999999999645 ) ) ;
#77967 = ORIENTED_EDGE ( 'NONE', *, *, #79791, .F. ) ;
#77968 = CARTESIAN_POINT ( 'NONE',  ( 32.53135143123563466, -5.965225279485572685, 6.926385399448451885 ) ) ;
#77969 = CARTESIAN_POINT ( 'NONE',  ( -43.52287095715007581, -23.72773821059536203, 11.05748984161097503 ) ) ;
#77970 = AXIS2_PLACEMENT_3D ( 'NONE', #96046, #2711, #57505 ) ;
#77971 = CARTESIAN_POINT ( 'NONE',  ( 20.73430856240977249, 7.200853762728330665, -1.500000000000002220 ) ) ;
#77972 = B_SPLINE_CURVE_WITH_KNOTS ( 'NONE', 3,
 ( #47481, #69312, #23617, #15016 ),
 .UNSPECIFIED., .F., .F.,
 ( 4, 4 ),
 ( 0.6209434004830697296, 0.6299498317551853743 ),
 .UNSPECIFIED. ) ;
#77973 = CARTESIAN_POINT ( 'NONE',  ( -5.654682302363691626, -6.376774720514411854, 19.41635569784906323 ) ) ;
#77974 = CARTESIAN_POINT ( 'NONE',  ( -34.57050063697510467, -23.48786465467240347, 11.44779295918255535 ) ) ;
#77975 = CARTESIAN_POINT ( 'NONE',  ( -70.62287095715005592, -29.50250243563736774, 8.947779886222143375 ) ) ;
#77976 = ORIENTED_EDGE ( 'NONE', *, *, #67096, .T. ) ;
#77977 = DIRECTION ( 'NONE',  ( -3.773278334453079618E-23, 0.9999999999976377785, 2.173523156925979975E-06 ) ) ;
#77978 = CARTESIAN_POINT ( 'NONE',  ( 30.53060340732036337, -5.330559497947037428, 2.122526108693120861 ) ) ;
#77979 = EDGE_LOOP ( 'NONE', ( #6606, #49234, #46470, #61297 ) ) ;
#77980 = CARTESIAN_POINT ( 'NONE',  ( 13.99439195134931069, 14.96789054323355828, 11.49999999999998934 ) ) ;
#77981 = ORIENTED_EDGE ( 'NONE', *, *, #64252, .T. ) ;
#77982 = EDGE_LOOP ( 'NONE', ( #25616, #71402, #50218, #20687 ) ) ;
#77983 = VERTEX_POINT ( 'NONE', #7697 ) ;
#77984 = ORIENTED_EDGE ( 'NONE', *, *, #776, .T. ) ;
#77985 = B_SPLINE_CURVE_WITH_KNOTS ( 'NONE', 3,
 ( #57984, #65106, #66334, #83015 ),
 .UNSPECIFIED., .F., .F.,
 ( 4, 4 ),
 ( 0.000000000000000000, 1.000000000000000000 ),
 .UNSPECIFIED. ) ;
#77986 = CARTESIAN_POINT ( 'NONE',  ( 5.395019145045520048, -22.42585393411717121, -1.500000000000002220 ) ) ;
#77987 = CARTESIAN_POINT ( 'NONE',  ( -112.5228709571500474, -23.73934037231757443, 11.05740245334328087 ) ) ;
#77988 = CARTESIAN_POINT ( 'NONE',  ( -6.888417027594036846, 19.07602104198033643, -1.500000000000002220 ) ) ;
#77989 = ORIENTED_EDGE ( 'NONE', *, *, #64578, .F. ) ;
#77990 = DIRECTION ( 'NONE',  ( 1.000000000000000000, 3.773278334444167608E-23, 8.201307833595939069E-29 ) ) ;
#77991 = CARTESIAN_POINT ( 'NONE',  ( -92.51515423418101136, -23.96119346886881374, -0.6495511937831873750 ) ) ;
#77992 = EDGE_CURVE ( 'NONE', #27734, #31312, #40648, .T. ) ;
#77994 = DIRECTION ( 'NONE',  ( 1.000000000000000000, 0.000000000000000000, -5.238131417152343399E-15 ) ) ;
#77993 = VECTOR ( 'NONE', #74576, 1000.000000000000000 ) ;
#77995 = CARTESIAN_POINT ( 'NONE',  ( 4.017909867803298063, -6.376774720514402972, 18.55402206357357286 ) ) ;
#77997 = ORIENTED_EDGE ( 'NONE', *, *, #24203, .F. ) ;
#77996 = CARTESIAN_POINT ( 'NONE',  ( -19.15072323977689095, -9.709862252083167888, 11.49999999999999645 ) ) ;
#77998 = CARTESIAN_POINT ( 'NONE',  ( -75.55242436766256731, -24.15503026093913519, -0.2815557561904521444 ) ) ;
#77999 = CARTESIAN_POINT ( 'NONE',  ( 14.70320764097967547, 3.414808732104102518, -28.39448918867740801 ) ) ;
#78000 = APPROVAL_PERSON_ORGANIZATION ( #4460, #29008, #51123 ) ;
#78001 = ORIENTED_EDGE ( 'NONE', *, *, #81891, .T. ) ;
#78002 = CARTESIAN_POINT ( 'NONE',  ( 1.902724757927627408, 20.64897553884969028, -1.500000000000002220 ) ) ;
#78003 = VERTEX_POINT ( 'NONE', #38642 ) ;
#78005 = EDGE_LOOP ( 'NONE', ( #86768, #13843, #74288, #97122 ) ) ;
#78004 = DIRECTION ( 'NONE',  ( 1.000000000000000000, 0.000000000000000000, 1.251281512149627050E-16 ) ) ;
#78006 = EDGE_CURVE ( 'NONE', #42298, #59704, #52864, .T. ) ;
#78007 = CARTESIAN_POINT ( 'NONE',  ( -41.53388201844860106, -24.51419770103157347, 9.386484678747180510 ) ) ;
#78008 = DIRECTION ( 'NONE',  ( -4.335561085774420994E-16, -0.000000000000000000, 1.000000000000000000 ) ) ;
#78009 = VERTEX_POINT ( 'NONE', #9195 ) ;
#78010 = VERTEX_POINT ( 'NONE', #54887 ) ;
#78011 = CARTESIAN_POINT ( 'NONE',  ( -40.52287095715005449, -23.48783264082476308, -1.443836473390097908 ) ) ;
#78012 = CARTESIAN_POINT ( 'NONE',  ( -42.63428171904830322, -24.35071581493543036, 9.817618358456037697 ) ) ;
#78013 = CARTESIAN_POINT ( 'NONE',  ( -28.34221723987227293, -24.69535842467096032, 1.737203919470178271 ) ) ;
#78014 = CARTESIAN_POINT ( 'NONE',  ( 19.60348439636399931, 10.09110264789753053, 11.49999999999999645 ) ) ;
#78015 = DIRECTION ( 'NONE',  ( 0.000000000000000000, 0.000000000000000000, 1.000000000000000000 ) ) ;
#78016 = CARTESIAN_POINT ( 'NONE',  ( 11.64696156460271581, 19.30390316350253244, -1.500000000000002220 ) ) ;
#78017 = CARTESIAN_POINT ( 'NONE',  ( 2.184583272949580213, -20.89682302726931340, 11.49999999999998934 ) ) ;
#78018 = LINE ( 'NONE', #70433, #88057 ) ;
#78020 = ORIENTED_EDGE ( 'NONE', *, *, #22351, .F. ) ;
#78019 = DIRECTION ( 'NONE',  ( 0.000000000000000000, 0.000000000000000000, 1.000000000000000000 ) ) ;
#78021 = ORIENTED_EDGE ( 'NONE', *, *, #7531, .T. ) ;
#78022 = FACE_OUTER_BOUND ( 'NONE', #65907, .T. ) ;
#78023 = ADVANCED_FACE ( 'NONE', ( #41164 ), #79206, .F. ) ;
#78024 = VECTOR ( 'NONE', #81423, 1000.000000000000114 ) ;
#78025 = CARTESIAN_POINT ( 'NONE',  ( 29.77147767949870527, -4.540774720514427543, 26.15915692125055614 ) ) ;
#78026 = ORIENTED_EDGE ( 'NONE', *, *, #12155, .F. ) ;
#78027 = CARTESIAN_POINT ( 'NONE',  ( -3.044128750896296420, -20.94304649679510888, -1.500000000000002220 ) ) ;
#78028 = CARTESIAN_POINT ( 'NONE',  ( -126.6228709571500275, -23.48783264082479505, -1.443836473390057051 ) ) ;
#78029 = CARTESIAN_POINT ( 'NONE',  ( -59.79865720102922921, -25.03722704563418944, 7.590184509431679771 ) ) ;
#78030 = CARTESIAN_POINT ( 'NONE',  ( -88.62287095715002749, -24.50321055353805377, 9.387540953477525818 ) ) ;
#78031 = FACE_OUTER_BOUND ( 'NONE', #82737, .T. ) ;
#78032 = CARTESIAN_POINT ( 'NONE',  ( -81.52287095715010423, -23.47593901973090524, -1.443836447538996648 ) ) ;
#78033 = CARTESIAN_POINT ( 'NONE',  ( 19.81268554055766273, 9.900562300003143079, -1.500000000000002220 ) ) ;
#78034 = CARTESIAN_POINT ( 'NONE',  ( -71.59683346284329275, -23.96119346886880308, -0.6495511937832095795 ) ) ;
#78035 = ORIENTED_EDGE ( 'NONE', *, *, #70046, .F. ) ;
#78036 = CARTESIAN_POINT ( 'NONE',  ( 14.43441819135927950, 3.316774720514427344, -28.36222020317712378 ) ) ;
#78037 = CARTESIAN_POINT ( 'NONE',  ( -37.51296537665867703, -23.73766607897670866, -1.055555164236442245 ) ) ;
#78038 = CARTESIAN_POINT ( 'NONE',  ( -40.37291966744255234, -25.30367284796214378, 5.540795143838759707 ) ) ;
#78039 = EDGE_CURVE ( 'NONE', #5376, #77258, #79710, .T. ) ;
#78040 = ADVANCED_FACE ( 'NONE', ( #40155 ), #63512, .F. ) ;
#78041 = DIRECTION ( 'NONE',  ( -1.000000000000000000, -0.000000000000000000, -0.000000000000000000 ) ) ;
#78042 = DIRECTION ( 'NONE',  ( -0.000000000000000000, 1.000000000000000000, -0.000000000000000000 ) ) ;
#78043 = CARTESIAN_POINT ( 'NONE',  ( -0.2416374764669896869, -19.45557994585427508, -1.500000000000002220 ) ) ;
#78044 = EDGE_CURVE ( 'NONE', #38164, #97904, #93424, .T. ) ;
#78045 = CARTESIAN_POINT ( 'NONE',  ( 20.92345209525186078, -4.499874906010187026, -1.500000000000002220 ) ) ;
#78046 = CARTESIAN_POINT ( 'NONE',  ( -38.52287095715009713, -23.96177878511310055, 10.65340807706330573 ) ) ;
#78047 = CARTESIAN_POINT ( 'NONE',  ( 8.971512145086503409, -1.000000000000001110, -3.746884140868835367 ) ) ;
#78048 = VECTOR ( 'NONE', #22150, 1000.000000000000000 ) ;
#78049 = CARTESIAN_POINT ( 'NONE',  ( -51.50150689877243337, -24.15543982623907127, -0.2315651400026664530 ) ) ;
#78050 = DIRECTION ( 'NONE',  ( 0.000000000000000000, 0.000000000000000000, 1.000000000000000000 ) ) ;
#78051 = CARTESIAN_POINT ( 'NONE',  ( -22.63693132222386950, 1.387278323242118416, -1.500000000000002220 ) ) ;
#78052 = B_SPLINE_CURVE_WITH_KNOTS ( 'NONE', 3,
 ( #27916, #11682, #65512, #89815, #96432, #20285, #51259, #89321, #66999, #26922, #5574, #19790, #82198, #13174, #81708, #81206, #73106, #44145, #42665, #20785, #97911, #42168, #12683, #90314, #28404, #59371, #43646, #35041, #96932, #73598, #74584, #43156, #5074, #4593, #36024, #66512, #82693, #36519, #67485, #98409, #90814, #99412, #60386, #53762, #67988, #6071, #84188, #38021, #83692, #46144, #45149, #21778, #75571, #6574, #84691, #39020, #44643, #98912, #69972, #15683, #15179, #37026, #92800, #69476, #7072, #92304, #77570, #77068, #60874, #7573, #457, #23792, #29906, #22277, #14679, #31413, #22774, #52754, #54264, #68971, #62370, #29405, #100395, #14173, #76075, #13671, #53261, #93298, #91801, #45642, #38522, #76566, #83186, #30908, #99896, #37525, #61875, #61377, #91309, #68479, #30407, #23281, #85193, #46650, #8073, #47150, #56773, #54765, #87199, #1977, #95313, #95807, #47652, #55770, #79077, #17688, #10570, #24301, #32416, #86695, #33406, #25802, #63894, #63389, #80087, #16682, #86199, #48662, #17182, #9575, #41533, #25295, #8581, #32920, #55267, #64897, #41037, #40027, #85703, #78566, #16182, #78067, #40539, #18188, #2981, #87704, #62890, #71489, #39528, #964, #72487, #70480, #93809, #9074, #64398, #31917, #79585, #49161, #48153, #94807, #33915, #94303, #71992, #70986, #1476, #24791, #56275, #10075, #2473, #96810, #43531, #82083, #50147, #26800, #82576, #88706, #57763, #74468, #90192, #26303, #4960, #12567, #11564, #36406, #19176, #88209, #35906, #66874, #97800, #73975, #35423, #57278, #27795, #28292, #13056, #58261, #20671, #97311, #51639, #42044, #81088, #51135, #59251, #27302, #89203, #44017, #74949, #5454, #67367, #19672, #66383, #96313, #18677, #49651, #43033, #42542, #80584, #12062, #11076, #4474, #58748, #72988, #3477, #34415, #73477, #89700, #65396, #50637, #3974, #34915, #65889, #81591, #20174, #84569, #22158, #6950, #92676, #68855, #75951, #99773, #15555, #52632, #44524, #45528, #75448, #61259, #60260, #37904, #91678, #5948, #98286, #21169, #15056, #98793, #91183, #28793, #68359, #46516, #14051, #99292, #30280, #46027, #59758, #76946, #83059, #92181, #29789, #30790, #29289, #6456, #53145, #7442, #67867, #69353, #13554, #90691, #100270, #52136, #22655, #76447, #38397, #60756, #14559, #53645, #61758, #84071, #23154, #54146, #85069, #77445, #36904, #7947, #38898, #37413, #21658, #83567, #45032, #1849, #17058, #9951, #10447, #86574, #48025, #48533, #94178, #79459, #87074, #17565, #24663, #62252, #40903, #78950, #47524, #95191, #31792, #838, #32787, #1352, #55643, #56647, #40408, #33281, #69858, #71864, #70861, #93176, #2353, #9449, #64269, #25675, #337, #71361, #87579, #18063, #49031, #77940, #63769, #79960, #16052, #31283, #23663, #54635, #85569, #24169, #47023, #55141, #8453, #39400, #78448, #86074, #8950, #56144, #70354, #16548, #62761, #39898, #32287, #25169, #63257, #93679, #94683, #33792, #58144, #81474, #57644, #97189, #64776, #35794, #88585, #19557, #43415, #11450, #18560, #2860, #74350, #95691, #51023, #27684, #65768, #50516, #66766, #58633, #89579, #89081, #34299, #96198, #88088, #11948, #49534, #4352, #3365, #42915, #34797, #80464, #41409, #26177, #20061, #41923, #65275, #72364, #42429, #57151, #10956, #73361, #96683, #81964, #72865, #12445, #26685, #35303, #3856, #4841, #19058, #50032, #27185, #97684, #80967, #28180, #73854, #66266, #59138, #90077, #20548, #82456, #51522, #21540, #29168, #52516, #99655, #12937, #60143, #59637, #83447, #91066, #68737, #13937, #30161, #61135, #36789, #13437, #76325, #44910, #92062, #36295, #7317, #75834, #91561, #14929, #6332, #90569, #74837, #45903, #67251, #22532, #53525, #37288, #22039, #38272, #83952, #68239, #14433, #5833, #67752, #21048, #60640, #52017, #6825, #75335, #53022, #99168, #82946, #43904, #98173, #84448, #44411, #98671, #5335, #29667, #61636, #45407, #37783, #76819, #69229, #28675, #100145, #30667, #92556, #23028, #54018, #85442, #62629, #78325, #1723, #54509, #56019, #69736, #77323, #86949, #84947, #16936, #32159, #711, #85953, #1225, #63132, #63638, #8830, #94559, #32661, #25044, #39767, #7824, #17437, #94058, #93548, #9827, #46896, #15929, #47900, #16426, #70730, #55517, #38771, #24544, #77816, #95067, #71236, #70231, #25553, #8326, #46392, #40281, #48400, #79333, #86451, #78819, #15431, #9316, #40777, #71739, #47399, #214, #23531, #39271, #2232, #31159, #33161, #64145, #62129, #93051, #31658, #24042, #55015, #41282, #18933, #2732, #3730, #57022, #80846, #26564, #72238, #34174, #33669, #64650, #96070, #80338, #95565, #42308, #10329, #48905, #65145, #57523, #27059, #87452, #58022, #26049, #34674, #88460, #11823, #87960, #10832, #50400, #58516, #18439, #49912, #89453, #49412, #17944, #41798, #79831, #81342, #72741, #11331, #73237, #65644, #88960, #96558, #19435, #42794, #73726, #4221, #35175, #3241, #66144, #97061, #27564, #56522, #48742, #47224, #2558, #8661, #78146, #63979, #10162, #46726, #94889, #47729, #39097, #17778, #24874, #79663, #2065, #25381, #33004, #94392, #55850, #77652, #48232, #41121, #33495, #78645, #72078, #17269, #64482, #62452, #1051, #56358, #31993, #87790, #25886, #55347, #71572, #95396, #56858, #9151, #86778, #16266, #8159, #70054, #63470, #39603, #540, #32498, #31488, #79163, #9662, #62963, #87277, #93379, #23867, #93890, #54843, #85784, #70555, #24378, #40618, #86279, #1558, #40112, #16759, #71068, #3263, #71257, #39798, #78845, #1254, #49435, #25067, #9848, #25576, #56549, #41308, #65173, #9345, #86970, #40800, #87985, #33697, #47924, #72768, #17462, #34202, #48426, #10859, #40308, #96099, #1747, #32685, #26077, #26588, #8850, #18961, #95590, #94586, #49940, #63664, #70756, #64675, #57050, #18463, #87477, #17970, #32182, #10352, #80368, #57548, #71762, #88487, #79857, #63155, #24566, #94082, #41823, #55543, #2254, #33188, #86474, #16960, #56045, #79356, #64170, #48929, #95091, #72268, #2756, #97582, #81366, #3756, #66670, #73263, #28083, #42819, #19456, #34698, #4249, #82357, #36686, #42330, #65669, #67651, #13332, #51421, #27083, #35695, #74251, #50423, #90967, #20449, #59533, #67158, #36193, #98570, #21437, #27587, #19954, #81864, #29066, #89975, #11848, #51920, #4745, #60039, #12343, #58049, #88986, #43313, #97088, #73750, #12836, #96585, #35198, #43805, #58538, #80870, #74737, #59037, #66170, #5236, #98066, #11357, #89478, #50926, #20948, #28573, #90473, #82849, #44312, #75239, #5731, #69125, #100049, #84848, #8234, #21934, #30057, #53417, #31055, #77220, #91455, #15831, #61031, #46799, #91962, #54410, #52919, #39174, #14329, #83851, #69638, #77721, #52415, #84345, #44807, #23427, #30563, #85345, #70129, #83348, #76716, #616, #31562, #92952, #60540, #7217, #62524, #99064, #93454, #13832, #45306, #76227, #62027, #75725, #37678, #6228, #37184, #22434, #68637, #14828, #38673, #68140, #99555, #29562, #45796, #38166, #7726, #61535, #116, #6725, #92452, #22924, #15327, #53915, #46291, #47301, #19711, #40187, #3515, #27345, #94467, #1126, #85857, #58305, #78226, #34955, #11607, #49697, #34460, #50684, #96354, #1633, #26842, #16840, #78719, #70630, #73029, #32064, #88752, #86358, #65435, #17344, #63038, #23947, #8736, #42584, #24451, #47800, #54914, #24949, #74019, #71140, #55925, #80627, #73521, #16335, #4011, #39674, #19220, #86847, #89242, #55419, #32565, #11114, #65930, #93960, #9223, #81630, #42084, #12104, #63545, #57806, #50187, #81126, #43074, #96850, #4514, #35461, #66431, #44567, #37453, #37945, #90238, #98333, #21212, #29333, #53187, #66920, #74998, #28840, #75995, #21705, #35951, #5498, #22203, #59292, #28334, #60304, #59805, #52179, #84118, #67917, #51182, #75494, #97840, #6998, #83615, #82618, #97353, #20713, #58793, #52678, #45075, #60803, #45574, #68404, #5002, #83110, #27838, #43571, #14602, #89744, #51685, #13097, #6503, #20212, #14099, #99336, #90739, #13600, #76491, #29832, #91724, #82125, #44065, #74507, #36447, #67413, #12609, #5996, #36946, #98837, #91228, #69399, #31842, #30835, #7490, #61302, #92719, #70401, #24714, #30328, #53687, #46073, #92228, #1400, #22700, #78495, #55193, #93224, #77988, #63308, #39452, #46564, #889, #86621, #9497, #15601, #7995, #69898, #55693, #8502, #38446, #62300, #15106, #68894, #84618, #86122, #100318, #61800, #99821, #38943, #17107, #85116, #383, #62811, #77493, #48072, #93725, #23713, #23207, #24218, #47074, #54192, #31331, #54684, #16598, #76992, #85615, #16104, #47575, #79000, #8995, #39949, #70909, #32335, #94227, #33328, #95238, #87119, #88134, #17613, #3409, #79509, #11494, #64825, #96733, #41457, #48585, #9997, #2907, #56700, #40953, #11002, #25217, #63817, #72414, #95738, #26728, #1895, #57688, #56195, #34345, #18602, #89129, #50562, #71915, #81015, #81519, #2400, #72912, #34843, #64319, #71408, #25722, #32841, #42471, #87631, #33837, #57201, #49578, #19103, #26227, #18115, #49081, #80511, #50075, #65324, #80008, #3904, #10496, #65812, #41969, #73410, #96244, #27232, #88633, #58187, #19601, #40459, #94730, #60187, #12983, #83494, #90617, #13981, #6381, #42963, #36337, #75881, #60684, #52561, #20103, #67295, #22084, #58675, #29716, #53070, #51069, #82010, #21588, #4398, #36839, #11994, #91607, #20600, #28220, #51569, #98721, #73899, #59180, #89624, #82500, #90121, #67802, #43948, #29219, #91112, #35837, #12495, #75380, #74394, #43460, #35346, #37341, #74881, #21096, #44957, #5384, #4891, #66309, #68285, #99214, #52064, #66808, #97237, #98215, #27727, #28725, #97730, #59685, #82992, #13485, #44453, #5878, #100191, #54067, #93098, #61681, #39818, #54551, #7870, #22574, #15972, #62175, #32201, #94101, #68781, #24088, #24588, #53571, #46942, #78370, #70776, #83997, #77865, #31202, #55059, #14480, #76862, #84991, #38816, #8372, #1273, #84496, #92598, #15476, #62678, #39317, #14978, #47442, #23076, #8872, #45951, #70278, #46437, #69781, #63175, #85489, #37828, #23581, #7364, #45457, #758, #69277, #76371, #38317, #6874, #31711, #93595, #85997, #16470, #99699, #92107, #258, #30204, #61186, #30711, #77369, #94607, #25087, #65192, #47944, #80388, #34220, #56568, #87499, #73280, #10877, #18979, #88503, #17987, #95610, #95110, #33207, #41843, #25598, #72785, #3283, #79377, #56063, #18483, #17483, #86991, #78865, #9870, #57069, #11373, #16978, #40327, #42348, #49958, #26097, #9366, #96116, #26605, #79876, #64695, #80887, #88004, #64189, #49454, #3774, #96601, #2279, #48948, #10370, #57566, #41329, #34713, #65687, #72285, #48447, #2777, #55561, #40820, #33716, #86495, #71279, #71783, #1767, #32706, #63687, #13854, #27100, #59554, #74758, #67670, #68158, #19975, #28100, #51439, #90491, #36705, #44330, #75259, #82376, #19475, #98591, #36211, #4762, #52436, #89494, #58555, #20967, #59057, #12855, #44826, #98085, #81385, #5253, #27606, #37205, #50439, #29085, #67175, #60059, #21457, #58069, #43823, #90986, #75747, #83367, #35216, #28591, #89002, #73767, #6247, #11866, #66188, #97109, #42837, #4267, #12359, #50944, #81882, #35716, #43332, #66689, #13354, #74270, #97600, #89993, #20467, #51938, #82867, #5751, #15849, #54430, #22453, #99575, #62046, #61050, #85364, #21953, #93471, #14849, #77238, #633, #69146, #76247, #60560, #31581, #52938, #8252, #46821, #22945, #7745, #23964, #69657, #76736, #134, #16353, #53438, #45325, #46312, #6744, #92972, #91982, #38691, #92472, #37698, #99084, #83869, #77737, #30080, #84367, #29583, #100067, #47319, #45815, #30583, #31075, #23447, #70147, #54933, #91478, #53936, #62545, #78243, #39191, #68658, #84867, #8754, #7238, #39692, #14349, #38187, #61554, #85876, #15349, #95489, #49333, #49838, #79252, #86867, #9750, #56947, #70651, #17362, #16859, #40705, #48324, #25975, #71659, #87881, #18365, #94484, #71159, #33591, #32584, #9241, #63057, #65072, #2158, #48831, #72662, #33091, #47818, #32081, #3159, #93978, #80265, #10758, #94984, #79757, #95989, #41212, #64070, #72165, #88380, #11253, #25471, #17867, #78740, #64570, #63564, #10250, #56447, #40203, #1143, #24470, #41722, #1649, #24968, #55436, #87372, #18861, #2655, #34100, #26487, #57451, #80771, #86375, #55942, #36089, #43215, #75141, #42721, #19847, #35601, #59430, #11744, #65571, #44209, #4646, #28968, #42229, #74641, #89873, #82752, #83253, #35099, #20343, #20846, #66572, #51823, #90371, #13235, #97485, #34599, #5632, #51317, #50822, #67549, #4147, #73654, #5135, #74153, #27978, #59942, #12734, #96486, #73162, #28465, #36578, #66068, #26977, #98467, #58931, #90870, #3653, #67057, #82257, #21341, #57948, #96988, #43704, #97966, #52319, #88887, #27487, #81763, #19360, #50325, #81261, #58443, #12234, #89377, #76133, #45206, #46198, #45702, #38078, #521, #84754, #68047, #92364, #14231, #77129, #69033, #29461, #99961, #85250, #8143, #44705, #30471, #77631, #62433, #54325, #21841, #61437, #23851, #60444, #31471, #54825, #52816, #83751, #23340, #6130, #38584, #92863, #14735, #93359, #7637, #39080, #46708, #76627, #53821, #6631, #13734, #70034, #22834, #37585, #37083, #15241, #98971, #69544, #24, #29966, #30967, #91365, #75630, #68537, #99467, #60935, #91866, #22337, #61933, #53321, #15743, #7128, #84250, #95870, #25357, #64460, #72053, #41099, #2041, #78624, #40090, #31976, #32983, #72547, #94867, #24359, #56835, #9638, #41602, #86756, #62944, #93868, #48212, #1534, #55326, #56336, #70537, #8641, #17244, #40598, #2537, #47207, #33469, #86260, #17751, #63958, #33975, #26365, #1025, #25861, #16740, #9131, #16246, #55829, #64958, #32474, #79140, #87256, #63448, #3039, #48722, #71548, #47708, #79640, #18250, #71045, #94368, #10135, #95373, #24855, #39585, #87768, #49222, #85760, #78126, #80150, #10640, #97858, #98356, #50208, #58326, #81653, #89763, #66941, #74531, #5022, #12123, #49719, #28352, #66455, #34977, #82638, #19241, #88773, #20234, #89263, #43097, #44088, #27858, #11137, #35483, #57830, #51203, #73052, #74040, #81150, #18740, #12631, #35970, #43591, #4537, #97375, #57338, #58814, #59315, #75017, #19731, #51703, #82145, #13120, #3537, #11627, #90259, #20735, #5515, #36466, #67431, #88268, #80652, #42106, #50703, #34479, #26863, #65456, #96373, #42605, #73541, #4033, #65952, #96874, #27364, #70300, #45097, #21231, #52699, #31732, #86513, #90757, #13618, #16997, #63198, #780, #75516, #85509, #23599, #98859, #40346, #62698, #8893, #16490, #86014, #46963, #21725, #77387, #69797, #31226, #47964, #39338, #67936, #1291, #54571, #78887, #62195, #6015, #93614, #29353, #9387, #55583, #77884, #60328, #52202, #15992, #83130, #24108, #91252, #83638, #44588, #14120, #55081, #71301, #36970, #7887, #28862, #94121, #47462, #38838, #8390, #78389, #276, #59824, #39839, #70800, #32221, #24605, #93118, #42859, #48967, #41348, #2797, #89022, #10897, #40839, #73302, #26119, #58088, #33734, #79398, #9888, #64716, #18005, #71805, #72801, #87013, #72301, #41862, #79897, #19498, #3308, #57090, #2296, #34240, #80405, #50458, #11889, #17505, #42369, #1787, #33226, #65214, #96620, #64207, #32726, #95130, #49475, #3796, #63709, #25619, #95634, #88025, #96138, #81409, #56589, #10390, #18501, #80904, #26625, #87525, #65707, #57586, #27122, #88523, #34735, #18998, #49977, #94625, #11392, #56081, #25106, #48469, #36727, #98109, #89514, #28615, #74291, #35237, #29104, #21477, #60080, #20986, #82888, #73788, #75277, #44845, #19999, #91497, #14370, #12381, #43354, #83387, #66208, #98612, #52455, #59578, #60580, #21975, #67693, #37226, #6269, #5273, #52957, #4287, #20489, #12873, #50967, #91004, #35737, #13373, #67194, #81904, #97127, #27627, #13874, #4782, #66708, #58573, #43847, #83888, #90017, #74776, #44351, #51460, #29601, #5770, #97619, #75769, #36231, #68178, #28120, #82395, #90509, #99104, #59080, #51959, #47338, #7765, #32099, #45346, #77756, #92991, #85892, #86393, #38211, #46331, #23982, #69675, #54954, #62567, #93492, #155, #37717, #16372, #54449, #22966, #70670, #7257, #76757, #8270, #77262, #31098, #63073, #15872, #99596, #23468, #31600, #78260, #85383, #53957, #46838, #8773, #39710, #76268, #62067, #1164, #93998, #24487, #53461, #39209, #55454, #92000, #6762, #68676, #84390, #14870, #100087, #30099, #30601, #61072, #22470, #45838, #84886, #69167, #61573, #92496, #15368, #38712, #70168, #652, #72680, #87392, #34118, #3179, #40722, #17381, #79274, #55960, #9261, #71679, #18384, #73181, #78760, #1667, #3671, #49858, #87901, #63581, #72184, #10272, #86889, #26999, #56966, #96010, #65091, #26505, #11269, #9768, #47839, #48344, #40225, #57468, #33109, #17887, #33611, #64593, #88402, #41229, #18877, #80788, #42251, #2673, #71178, #34619, #25994, #95003, #65588, #25495, #96503, #2177, #57966, #64087, #56466, #16876, #32606, #94504, #24985, #48850, #49353, #79775, #95507, #80283, #10777, #41740, #12753, #52335, #97986, #88905, #90392, #59958, #75647, #20361, #83272, #59448, #13750, #4165, #43233, #67567, #74170, #29477, #42739, #44721, #66590, #28986, #75158, #19376, #28484, #58461, #6147, #37099, #5156, #89395, #11763, #74658, #81282, #36106, #20867, #4666, #44227, #73672, #68063, #35616, #67076, #90886, #58954, #66089, #51838, #35116, #43725, #82278, #19868, #98987, #82772, #98485, #5649, #36598, #13254, #81782, #97502, #97004, #21361, #27506, #50342, #50842, #12253, #27997, #89893, #51336, #37603, #68552, #22850, #76642, #99486, #30983, #45223, #83767, #61452, #15257, #46722, #21857, #77648, #76148, #54340, #92379, #93374, #60952, #6647, #536, #70550, #29981, #92877, #38600, #91879, #23356, #84769, #22352, #46213, #53339, #52830, #15757, #8155, #39093, #7651, #69559, #60462, #61950, #1044, #84267, #78141, #91380, #14751, #45719, #70050, #14249, #85264, #31484, #77147, #47219, #8656, #62447, #23862, #54839, #53838, #38, #7143, #39598, #85779, #30484, #16261, #38095, #69048, #99975, #95390, #94385, #71062, #24373, #55844, #33488, #88285, #93885, #16754, #18757, #64974, #2552, #78640, #87271, #18266, #56352, #41115, #26382, #64476, #9656, #25880, #49736, #73068, #79156, #71565, #32998, #80665, #72072, #1551, #3056, #17771, #11151, #63973, #9146, #32491, #24868, #62957, #2058, #42128, #48226, #94883, #56851, #40611, #31988, #87783, #48736, #63464, #49238, #10154, #55342, #86274, #47724, #72562, #40105, #86772, #33998, #25374, #17262, #79656, #80168, #10659, #95887, #41619, #57353, #4554, #27875, #35985, #59837, #73558, #81668, #35500, #82657, #28369, #42621, #12140, #28874, #65971, #34991, #66957, #66475, #58832, #90774, #74550, #57850, #34496, #74056, #52220, #19747, #97390, #12643, #43111, #21246, #5037, #89780, #97871, #20250, #36481, #4049, #51217, #82160, #20748, #96891, #26880, #5530, #43606, #83149, #3552, #59328, #90274, #44104, #44603, #27383, #51716, #13135, #13633, #58345, #75032, #67446, #98371, #65471, #89280, #96388, #88790, #19255, #50226, #81165, #50722, #11645, #45113, #14134, #46104, #61836, #75530, #77032, #76526, #91270, #7031, #76031, #67949, #7533, #38487, #69435, #99860, #30365, #6033, #53723, #92758, #46609, #14641, #54226, #22738, #85151, #21742, #99373, #100354, #30871, #37984, #15641, #77531, #84653, #23242, #8028, #45605, #92262, #6538, #36985, #98876, #15141, #68437, #52715, #61339, #83652, #29366, #60345, #68934, #29869, #37485, #60840, #91757, #84150, #22238, #53222, #98700, #36316, #11974, #20576, #59158, #35324, #75857, #5362, #44434, #52041, #21074, #82479, #6361, #12472, #4867, #66789, #52537, #74858, #4376, #36815, #90102, #21565, #97707, #42942, #73877, #28201, #81988, #83473, #27209, #50540, #13960, #29198, #60167, #89107, #75358, #82970, #51548, #67276, #91089, #98194, #43440, #28704, #44936, #65791, #74371, #35815, #12960, #96706, #59664, #66285, #67782, #43928, #58163, #19580, #13460, #97211, #58653, #81494, #90595, #27707, #5858, #89601, #20081, #51049, #93573, #7848, #61659, #76351, #69758, #15456, #85976, #47421, #30688, #54532, #6853, #60663, #39297, #100171, #24068, #37318, #239, #84971, #77843, #78349, #30182, #38297, #92577, #31181, #55038, #37807, #14956, #69253, #29693, #8349, #46416, #45930, #62658, #99679, #68759, #62155, #23055, #54045, #16451, #38797, #91585, #77348, #61165, #93078, #23563, #53046, #85467, #92084, #31690, #68265, #15952, #737, #99192, #70254, #45436, #46918, #22065, #83976, #14456, #22554, #53546, #84476, #76840, #7342, #80912, #88530, #64214, #4295, #73309, #73797, #42866, #41869, #49985, #79907, #97135, #35245, #26633, #10397, #33234, #96146, #2303, #57593, #11403, #26126, #65715, #95140, #66215, #9896, #87532, #18012, #72813, #57097, #48975, #42377, #25626, #56598, #10906, #65222, #96628, #71813, #27131, #41355, #3804, #3316, #27635, #72309, #88034, #34247, #20007, #2806, #34742, #58580, #33743, #40847, #64724, #95641, #50467, #18508, #19006, #58095, #89031, #19506, #81416, #11897, #89523, #50974, #49482, #80412, #20496, #45354, #90516, #76276, #59586, #83900, #82402, #37725, #43854, #12881, #99113, #6770, #81911, #68186, #60589, #91012, #20994, #60088, #52965, #68685, #29609, #37235, #29113, #21485, #12389, #83396, #14378, #99604, #13380, #30107, #52464, #61080, #97626, #67203, #6277, #13881, #44855, #35745, #92009, #51966, #91505, #43362, #28622, #28130, #82895, #44360, #21984, #75284, #22480, #74298, #5281, #74783, #75778, #36242, #51468, #4790, #98116, #66716, #59087, #90024, #5779, #36734, #67702, #98619, #76765, #63080, #39718, #77764, #62574, #47846, #23992, #31105, #54961, #71185, #94511, #164, #93000, #54456, #40233, #93499, #85900, #46845, #100095, #1675, #78768, #70175, #53965, #7265, #39218, #45846, #660, #16379, #69682, #8780, #38219, #9268, #62076, #31607, #55463, #23475, #86400, #47345, #30609, #8277, #78269, #22975, #63589, #70677, #32107, #1171, #94006, #24494, #46339, #7774, #61584, #16885, #92504, #32613, #15376, #53470, #84399, #14879, #85390, #84895, #77270, #15880, #69175, #38720, #96017, #9775, #48352, #26001, #80291, #11277, #86897, #42258, #40729, #18884, #56973, #57974, #35124, #71687, #65596, #66097, #64094, #57476, #19384, #87400, #55970, #95012, #17389, #96512, #41236, #87909, #41748, #72689, #3679, #49361, #34627, #73189, #18391, #27007, #49865, #25503, #88913, #33619, #50351, #2680, #81290, #56475, #11774, #17895, #48857, #42747, #73680, #24992, #4174, #79281, #34126, #64601, #79782, #2184, #80797, #33116, #10279, #3186, #65098, #72191, #26512, #95515, #10784, #88410, #91387, #67576, #21864, #12263, #82286, #21369, #98493, #75167, #83774, #14256, #59966, #60469, #29485, #28495, #36608, #66598, #20876, #89404, #68070, #5657, #74667, #52838, #58962, #28005, #28995, #59456, #51847, #45232, #13757, #76155, #97014, #83279, #75654, #90896, #5164, #52343, #98994, #6654, #27514, #82780, #37610, #58469, #37108, #4675, #13262, #19876, #43242, #50851, #44730, #81790, #74179, #12762, #6155, #35624, #97510, #89902, #20371, #36115, #51345, #43733, #67084, #97994, #90401, #44236, #46220, #23871, #38606, #85787, #54346, #60960, #85273, #8162, #84775, #54846, #91885, #62966, #15263, #46729, #70558, #69566, #45725, #29988, #1055, #22358, #78149, #16269, #92883, #77655, #47228, #8664, #39606, #15764, #61459, #22857, #14756, #39100, #76648, #31491, #30490, #70057, #61957, #7150, #68562, #53347, #31996, #69056, #92385, #99493, #543, #84274, #38102, #44, #23362, #93893, #99981, #24381, #53844, #62455, #30990, #55350, #77154, #7657, #93383, #86282, #16764, #47732, #78648, #9155, #71071, #9667, #32501, #80674, #56362, #41125, #56861, #87793, #18766, #64485, #49748, #57363, #88295, #24877, #34007, #72081, #73077, #40621, #17781, #33499, #71575, #63473, #42137, #2563, #26889, #40115, #72572, #18277, #11162, #81174, #33007, #95400, #25889, #3067, #96399, #2068, #48745, #49249, #3562, #64983, #80176, #79666, #65480, #63982, #94893, #95897, #10668, #41630, #57861, #26392, #94395, #34507, #25385, #88800, #19265, #55854, #50236, #87280, #1561, #86781, #17273, #48235, #79166, #10165, #19756, #35994, #21751, #58354, #29377, #52725, #50732, #81677, #11653, #59337, #35511, #20757, #66968, #98886, #60354, #75044, #98381, #42630, #58842, #89290, #51227, #89789, #67455, #82171, #28884, #59848, #66486, #12151, #5540, #74069, #43120, #4058, #97399, #13144, #67959, #73568, #12654, #4563, #35002, #44613, #65982, #21255, #90785, #97880, #51729, #6043, #82666, #20259, #44116, #91280, #96900, #43618, #74559, #5047, #27394, #36490, #52229, #28378, #27885, #90286, #83159, #13643, #75539, #36994, #14144, #53732, #31885, #99869, #84663, #92767, #61348, #39498, #54235, #7542, #23253, #38497, #78033, #92272, #23757, #69939, #83662, #30376, #29878, #22749, #15150, #38989, #46114, #427, #31380, #7042, #84159, #46619, #45615, #22249, #76041, #37994, #77041, #61846, #85668, #69446, #60849, #45122, #16149, #6548, #93269, #62343, #100364, #85161, #8545, #15650, #30880, #77540, #935, #24266, #8039, #54734, #91767, #47120, #76535, #70448, #62858, #53231, #37495, #68447, #93775, #14650, #68944, #99383, #25263, #3451, #71457, #56242, #64362, #32889, #11048, #25769, #39994, #49127, #87167, #88177, #55738, #63861, #48627, #72454, #24757, #78537, #57242, #17656, #42012, #55240, #87673, #2440, #95780, #96282, #48119, #79552, #33883, #10042, #64867, #2948, #26270, #41002, #47618, #18645, #95284, #94775, #80553, #17153, #86664, #18154, #71959, #33374, #72955, #56741, #9041, #80054, #41501, #49623, #10540, #34386, #65363, #86166, #16648, #70955, #1443, #32381, #63357, #94274, #79048, #9542, #40503, #1945, #44495, #67841, #65859, #96777, #12036, #51607, #5423, #51108, #36375, #43987, #74919, #82052, #19148, #98256, #35878, #4442, #52107, #89171, #58232, #59219, #58717, #12533, #13523, #97769, #90657, #26769, #13023, #67335, #66847, #35392, #4931, #28764, #21136, #57734, #43501, #83033, #75418, #59727, #34883, #74438, #36875, #73450, #5920, #88676, #50116, #42512, #43003, #82543, #28263, #90165, #81055, #11537, #66354, #3943, #27276, #19644, #73945, #50608, #97279, #27767, #81561, #89668, #20145, #20639, #99260, #61724, #60726, #37380, #91153, #22128, #100239, #54600, #60228, #83537, #85535, #31250, #69318, #45000, #53613, #92147, #68326, #8418, #38365, #77411, #76415, #30753, #16019, #39369, #45499, #37872, #99742, #46987, #7409, #29759, #69822, #22622, #77910, #30247, #75920, #6426, #61228, #14524, #91647, #92644, #6918, #68825, #23123, #84538, #98761, #54112, #15022, #53111, #85033, #76911, #29254, #21628, #14019, #38864, #52601, #84042, #15519, #93141, #45992, #46483, #7916, #306, #62221, #23625, #63223, #71329, #94653, #41378, #64745, #805, #25132, #33762, #18528, #10416, #78419, #56112, #80433, #16517, #88053, #10924, #95662, #86040, #55611, #95159, #40870, #48498, #24137, #26143, #47991, #72330, #56618, #70324, #17027, #47487, #9411, #78918, #25643, #40374, #87547, #18029, #62725, #87040, #9916, #86540, #48996, #93641, #57116, #1816, #79422, #2823, #32753, #8916, #31757, #49500, #55104, #79925, #39866, #17531, #71830, #70825, #1315, #32253, #2323, #94145, #24631, #63736, #33252, #64234, #6172, #3823, #50996, #35270, #88552, #41888, #65242, #60484, #42397, #34761, #72835, #11919, #26652, #96163, #42884, #97161, #29502, #3334, #91401, #57613, #37123, #73816, #76171, #73330, #19524, #66235, #21878, #11422, #19027, #45246, #4318, #30003, #65734, #34270, #83792, #58116, #27655, #58600, #89547, #52854, #20031, #14272, #6670, #37622, #81931, #50002, #68580, #13771, #50488, #99505, #96652, #27151, #89053, #60975, #81438, #44748, #91900, #22377, #80935, #53362, #84289, #75670, #68084, #99007, #77669, #31007, #92400, #85804, #99996, #38116, #15780, #70073, #71086, #16284, #39119, #53859, #47244, #93399, #63491, #24893, #30505, #55366, #55873, #84793, #78169, #9173, #77169, #45739, #15276, #7167, #86297, #61973, #7674, #46746, #561, #8682, #1579, #46238, #92900, #8178, #93907, #39622, #38621, #78664, #23378, #40132, #54361, #16785, #69581, #32516, #64, #85293, #69072, #23891, #31508, #70576, #62471, #61476, #54863, #1071, #76662, #32012, #62986, #24398, #47749, #94410, #14773, #22873, #57876, #73584, #18294, #81190, #25402, #56377, #27408, #34021, #10180, #95915, #10682, #4072, #35022, #49762, #50251, #19279, #49265, #26407, #87298, #65996, #11668, #3084, #17796, #9680, #41143, #48759, #80689, #79685, #72095, #79183, #2576, #88310, #42649, #48252, #71590, #96914, #86796, #57382, #33022, #41644, #80193, #33517, #17288, #18781, #73091, #42152, #64999, #64501, #95416, #63997, #11181, #94910, #3581, #25904, #34523, #72590, #56878, #40639, #2084, #65496, #96417, #26903, #87808, #88813, #68465, #4577, #76062, #99400, #97412, #27900, #58367, #5558, #82182, #67469, #82680, #45136, #6563, #21270, #21765, #91296, #90299, #98395, #58856, #37510, #13656, #28391, #75555, #44629, #12668, #89802, #52246, #20272, #51240, #50748, #43632, #59865, #14160, #19774, #43134, #89306, #52739, #28898, #35527, #13161, #6057, #44132, #90800, #75057, #81694, #37011, #36505, #74571, #5061, #66498, #83172, #36008, #67976, #66983, #98899, #51747, #97896, #12166, #74085, #29394, #20768, #59351, #60373, #83678, #14666, #53247, #30896, #85180, #16166, #91783, #47134, #45631, #23776, #61863, #62875, #30391, #7559, #23267, #78051, #99883, #62358, #24287, #92292, #60863, #61364, #22264, #70465, #46131, #92785, #46636, #77554, #8565, #54251, #39514, #951, #31900, #15667, #84176, #93791, #39006, #38510, #55254, #69459, #86183, #22764, #16666, #53749, #84678, #47637, #78553, #29895, #9058, #40009, #69959, #100382, #8057, #70969, #76550, #7058, #444, #38010, #31397, #68960, #77057, #93284, #54751, #85686, #15164, #72470, #25783, #40524, #33897, #80072, #50130, #11550, #86682, #42028, #42528, #71474, #64883, #64380, #88691, #1460, #95793, #49145, #72972, #32400, #94791, #2456, #56759, #26286, #57750, #1963, #79570, #33390, #80567, #57262, #32905, #65377, #10060, #63876, #25280, #88192, #95299, #87688, #19160, #2965, #55755, #10557, #56258, #18662, #18173, #17169, #41516, #87183, #63375, #49637, #11062, #3464, #34400, #96298, #9556, #26785, #94289, #48135, #81074, #24773, #17671, #48644, #79064, #41021, #71975, #82559, #97784, #60244, #91171, #36390, #36888, #5934, #4945, #19658, #12550, #51122, #28778, #43516, #90675, #59741, #97293, #73961, #67353, #35409, #12048, #65874, #27780, #74933, #29274, #34901, #58244, #21642, #67854, #98775, #96793, #83046, #21152, #58734, #66366, #52615, #3956, #82066, #5438, #83554, #14036, #20158, #74453, #35891, #73463, #13041, #43018, #44508, #28276, #27289, #89188, #52122, #4457, #89682, #13536, #50623, #81575, #75434, #66861, #44000, #59235, #51625, #90179, #20653, #98273, #69334, #8437, #93661, #85553, #46502, #16036, #31776, #76927, #39386, #15537, #70341, #60740, #30264, #69843, #77428, #23140, #99277, #823, #22639, #47003, #31269, #45016, #92165, #91664, #53631, #322, #15039, #62238, #93157, #68841, #45515, #7931, #6936, #84057, #37396, #99759, #38881, #62747, #6441, #29775, #24155, #77926, #23648, #22144, #54618, #55123, #61243, #37888, #86059, #75937, #84553, #68344, #53129, #14541, #46010, #7428, #38382, #76430, #54128, #100254, #30773, #61743, #92661, #85052, #33779, #17044, #9429, #47509, #87060, #65259, #32772, #17549, #25662, #94670, #72850, #87564, #40889, #55630, #49014, #95178, #96184, #26670, #1336, #57136, #86561, #39885, #18548, #79444, #3352, #16533, #79948, #64256, #88071, #57629, #40394, #48515, #71849, #10433, #34287, #48012, #25153, #9935, #95679, #41394, #56634, #56132, #41909, #78936, #71346, #72350, #2339, #33268, #78435, #18050, #2846, #64763, #8935, #26162, #49517, #1836, #63754, #63242, #80451, #94164, #10944, #70844, #32270, #24648, #44396, #89564, #65750, #96671, #51011, #4336, #27170, #59126, #73347, #11438, #20049, #43399, #74824, #50019, #5318, #3840, #20534, #66752, #36776, #98655, #34782, #28661, #29154, #58131, #51508, #82933, #50504, #19045, #89068, #80954, #59622, #35288, #81945, #4828, #35782, #67240, #75323, #19544, #66251, #12431, #98154, #12922, #81460, #52004, #97176, #13421, #27671, #90555, #11936, #5817, #42901, #73837, #36282, #67740, #88570, #21033, #74337, #58620, #97669, #28167, #42417, #43891, #90061, #82440, #7305, #69215, #60127, #61625, #31148, #46884, #92049, #54492, #30654, #85430, #75820, #45395, #83940, #100131, #84436, #77802, #8315, #23016, #23517, #93038, #22519, #92544, #29653, #39259, #15916, #76804, #60627, #83433, #45889, #52503, #38256, #54004, #99153, #13921, #14420, #84934, #70219, #21526, #44898, #699, #91053, #15417, #6319, #14915, #53513, #91548, #46377, #37767, #61118, #38756, #77311, #22021, #68724, #37274, #53010, #76311, #7812, #69725, #203, #68226, #62117, #6811, #99642, #30144, #95050, #56008, #47386, #86933, #32144, #93535, #87436, #79817, #95552, #80325, #72224, #39756, #17425, #41784, #78313, #49397, #72725, #70715, #1212, #31645, #79319, #55501, #40764, #48384, #18427, #10815, #25541, #26034, #62614, #78804, #8819, #71222, #9302, #17931, #1712, #48890, #10314, #86439, #63121, #56509, #94045, #24531, #24031, #16924, #33147 ),
 .UNSPECIFIED., .F., .F.,
 ( 4, 2, 2, 2, 2, 2, 2, 2, 2, 2, 2, 2, 2, 2, 2, 2, 2, 2, 2, 2, 2, 2, 2, 2, 2, 2, 2, 2, 2, 2, 2, 2, 2, 2, 2, 2, 2, 2, 2, 2, 2, 2, 2, 2, 2, 2, 2, 2, 2, 2, 2, 2, 2, 2, 2, 2, 2, 2, 2, 2, 2, 2, 2, 2, 2, 2, 2, 2, 2, 2, 2, 2, 2, 2, 2, 2, 2, 2, 2, 2, 2, 2, 2, 2, 2, 2, 2, 2, 2, 2, 2, 2, 2, 2, 2, 2, 2, 2, 2, 2, 2, 2, 2, 2, 2, 2, 2, 2, 2, 2, 2, 2, 2, 2, 2, 2, 2, 2, 2, 2, 2, 2, 2, 2, 2, 2, 2, 2, 2, 2, 2, 2, 2, 2, 2, 2, 2, 2, 2, 2, 2, 2, 2, 2, 2, 2, 2, 2, 2, 2, 2, 2, 2, 2, 2, 2, 2, 2, 2, 2, 2, 2, 2, 2, 2, 2, 2, 2, 2, 2, 2, 2, 2, 2, 2, 2, 2, 2, 2, 2, 2, 2, 2, 2, 2, 2, 2, 2, 2, 2, 2, 2, 2, 2, 2, 2, 2, 2, 2, 2, 2, 2, 2, 2, 2, 2, 2, 2, 2, 2, 2, 2, 2, 2, 2, 2, 2, 2, 2, 2, 2, 2, 2, 2, 2, 2, 2, 2, 2, 2, 2, 2, 2, 2, 2, 2, 2, 2, 2, 2, 2, 2, 2, 2, 2, 2, 2, 2, 2, 2, 2, 2, 2, 2, 2, 2, 2, 2, 2, 2, 2, 2, 2, 2, 2, 2, 2, 2, 2, 2, 2, 2, 2, 2, 2, 2, 2, 2, 2, 2, 2, 2, 2, 2, 2, 2, 2, 2, 2, 2, 2, 2, 2, 2, 2, 2, 2, 2, 2, 2, 2, 2, 2, 2, 2, 2, 2, 2, 2, 2, 2, 2, 2, 2, 2, 2, 2, 2, 2, 2, 2, 2, 2, 2, 2, 2, 2, 2, 2, 2, 2, 2, 2, 2, 2, 2, 2, 2, 2, 2, 2, 2, 2, 2, 2, 2, 2, 2, 2, 2, 2, 2, 2, 2, 2, 2, 2, 2, 2, 2, 2, 2, 2, 2, 2, 2, 2, 2, 2, 2, 2, 2, 2, 2, 2, 2, 2, 2, 2, 2, 2, 2, 2, 2, 2, 2, 2, 2, 2, 2, 2, 2, 2, 2, 2, 2, 2, 2, 2, 2, 2, 2, 2, 2, 2, 2, 2, 2, 2, 2, 2, 2, 2, 2, 2, 2, 2, 2, 2, 2, 2, 2, 2, 2, 2, 2, 2, 2, 2, 2, 2, 2, 2, 2, 2, 2, 2, 2, 2, 2, 2, 2, 2, 2, 2, 2, 2, 2, 2, 2, 2, 2, 2, 2, 2, 2, 2, 2, 2, 2, 2, 2, 2, 2, 2, 2, 2, 2, 2, 2, 2, 2, 2, 2, 2, 2, 2, 2, 2, 2, 2, 2, 2, 2, 2, 2, 2, 2, 2, 2, 2, 2, 2, 2, 2, 2, 2, 2, 2, 2, 2, 2, 2, 2, 2, 2, 2, 2, 2, 2, 2, 2, 2, 2, 2, 2, 2, 2, 2, 2, 2, 2, 2, 2, 2, 2, 2, 2, 2, 2, 2, 2, 2, 2, 2, 2, 2, 2, 2, 2, 2, 2, 2, 2, 2, 2, 2, 2, 2, 2, 2, 2, 2, 2, 2, 2, 2, 2, 2, 2, 2, 2, 2, 2, 2, 2, 2, 2, 2, 2, 2, 2, 2, 2, 2, 2, 2, 2, 2, 2, 2, 2, 2, 2, 2, 2, 2, 2, 2, 2, 2, 2, 2, 2, 2, 2, 2, 2, 2, 2, 2, 2, 2, 2, 2, 2, 2, 2, 2, 2, 2, 2, 2, 2, 2, 2, 2, 2, 2, 2, 2, 2, 2, 2, 2, 2, 2, 2, 2, 2, 2, 2, 2, 2, 2, 2, 2, 2, 2, 2, 2, 2, 2, 2, 2, 2, 2, 2, 2, 2, 2, 2, 2, 2, 2, 2, 2, 2, 2, 2, 2, 2, 2, 2, 2, 2, 2, 2, 2, 2, 2, 2, 2, 2, 2, 2, 2, 2, 2, 2, 2, 2, 2, 2, 2, 2, 2, 2, 2, 2, 2, 2, 2, 2, 2, 2, 2, 2, 2, 2, 2, 2, 2, 2, 2, 2, 2, 2, 2, 2, 2, 2, 2, 2, 2, 2, 2, 2, 2, 2, 2, 2, 2, 2, 2, 2, 2, 2, 2, 2, 2, 2, 2, 2, 2, 2, 2, 2, 2, 2, 2, 2, 2, 2, 2, 2, 2, 2, 2, 2, 2, 2, 2, 2, 2, 2, 2, 2, 2, 2, 2, 2, 2, 2, 2, 2, 2, 2, 2, 2, 2, 2, 2, 2, 2, 2, 2, 2, 2, 2, 2, 2, 2, 2, 2, 2, 2, 2, 2, 2, 2, 2, 2, 2, 2, 2, 2, 2, 2, 2, 2, 2, 2, 2, 2, 2, 2, 2, 2, 2, 2, 2, 2, 2, 2, 2, 2, 2, 2, 2, 2, 2, 2, 2, 2, 2, 2, 2, 2, 2, 2, 2, 2, 2, 2, 2, 2, 2, 2, 2, 2, 2, 2, 2, 2, 2, 2, 2, 2, 2, 2, 2, 2, 2, 2, 2, 2, 2, 2, 2, 2, 2, 2, 2, 2, 2, 2, 2, 2, 2, 2, 2, 2, 2, 2, 2, 2, 2, 2, 2, 2, 2, 2, 2, 2, 2, 2, 2, 2, 2, 2, 2, 2, 2, 2, 2, 2, 2, 2, 2, 2, 2, 2, 2, 2, 2, 2, 2, 2, 2, 2, 2, 2, 2, 2, 2, 2, 2, 2, 2, 2, 2, 2, 2, 2, 2, 2, 2, 2, 2, 2, 2, 2, 2, 2, 2, 2, 2, 2, 2, 2, 2, 2, 2, 2, 2, 2, 2, 2, 2, 2, 2, 2, 2, 2, 2, 2, 2, 2, 2, 2, 2, 2, 2, 2, 2, 2, 2, 2, 2, 2, 2, 2, 2, 2, 2, 2, 2, 2, 2, 2, 2, 2, 2, 2, 2, 2, 2, 2, 2, 2, 2, 2, 2, 2, 2, 2, 2, 2, 2, 2, 2, 2, 2, 2, 2, 2, 2, 2, 2, 2, 2, 2, 2, 2, 2, 2, 2, 2, 2, 2, 2, 2, 2, 2, 2, 2, 2, 2, 2, 2, 2, 2, 2, 2, 2, 2, 2, 2, 2, 2, 2, 2, 2, 2, 2, 2, 2, 2, 2, 2, 2, 2, 2, 2, 2, 2, 2, 2, 2, 2, 2, 2, 2, 2, 2, 2, 2, 2, 2, 2, 2, 2, 2, 2, 2, 2, 2, 2, 2, 2, 2, 2, 2, 2, 2, 2, 2, 2, 2, 2, 2, 2, 2, 2, 2, 2, 2, 2, 2, 2, 2, 2, 2, 2, 2, 2, 2, 2, 2, 2, 2, 2, 2, 2, 2, 2, 2, 2, 2, 2, 2, 2, 2, 2, 2, 2, 2, 2, 2, 2, 2, 2, 2, 2, 2, 2, 2, 2, 2, 2, 2, 2, 2, 2, 2, 2, 2, 2, 2, 2, 2, 2, 2, 2, 2, 2, 2, 2, 2, 2, 2, 2, 2, 2, 2, 2, 2, 2, 2, 2, 2, 2, 2, 2, 2, 2, 2, 2, 2, 2, 2, 2, 2, 2, 2, 2, 2, 2, 2, 2, 2, 2, 2, 2, 2, 2, 2, 2, 2, 2, 2, 2, 2, 2, 2, 2, 2, 2, 2, 2, 2, 2, 2, 2, 2, 2, 2, 2, 2, 2, 2, 2, 2, 2, 2, 2, 2, 2, 2, 2, 2, 2, 2, 2, 2, 2, 2, 2, 2, 2, 2, 2, 2, 2, 2, 2, 2, 2, 2, 2, 2, 2, 2, 2, 2, 2, 2, 2, 2, 2, 2, 2, 2, 2, 2, 2, 2, 2, 2, 2, 2, 2, 2, 2, 2, 2, 2, 2, 2, 2, 2, 2, 2, 2, 2, 2, 2, 2, 2, 2, 2, 2, 2, 2, 2, 2, 2, 2, 2, 2, 2, 2, 2, 2, 2, 2, 2, 2, 2, 2, 2, 2, 2, 2, 2, 2, 2, 2, 2, 2, 2, 2, 2, 2, 2, 2, 2, 2, 2, 2, 2, 2, 2, 2, 2, 2, 2, 2, 2, 2, 2, 2, 2, 2, 2, 2, 2, 2, 2, 2, 2, 2, 2, 2, 2, 2, 2, 2, 2, 2, 2, 2, 2, 2, 2, 2, 2, 2, 2, 2, 2, 2, 2, 2, 2, 2, 2, 2, 2, 2, 2, 2, 2, 2, 2, 2, 2, 2, 2, 2, 2, 2, 2, 2, 2, 2, 2, 2, 2, 2, 2, 2, 2, 2, 2, 2, 2, 2, 2, 2, 2, 2, 2, 2, 2, 2, 2, 2, 2, 2, 2, 2, 2, 2, 2, 2, 2, 2, 2, 2, 2, 2, 2, 2, 2, 2, 2, 2, 2, 2, 2, 2, 2, 2, 2, 2, 2, 2, 2, 2, 2, 2, 2, 2, 2, 2, 2, 2, 2, 2, 2, 2, 2, 2, 2, 2, 2, 2, 2, 2, 2, 2, 2, 2, 2, 2, 2, 2, 2, 2, 2, 2, 2, 2, 2, 2, 2, 2, 2, 2, 2, 2, 2, 2, 2, 2, 2, 2, 2, 2, 2, 2, 2, 2, 2, 2, 2, 2, 2, 2, 2, 2, 2, 2, 2, 2, 2, 2, 2, 2, 2, 2, 2, 2, 2, 2, 2, 2, 2, 2, 2, 2, 2, 2, 2, 2, 2, 2, 2, 2, 2, 2, 2, 2, 2, 2, 2, 2, 2, 2, 2, 2, 2, 2, 2, 2, 2, 2, 2, 2, 2, 2, 2, 2, 2, 2, 2, 2, 2, 2, 2, 2, 2, 2, 2, 2, 2, 2, 2, 2, 2, 2, 2, 2, 2, 2, 2, 2, 2, 2, 2, 2, 2, 2, 2, 2, 2, 2, 2, 2, 2, 2, 2, 2, 2, 2, 2, 2, 2, 2, 2, 2, 2, 2, 2, 2, 2, 2, 2, 2, 2, 2, 2, 2, 2, 2, 2, 2, 2, 2, 2, 2, 2, 2, 2, 2, 2, 2, 2, 2, 2, 2, 2, 2, 2, 2, 2, 2, 2, 2, 2, 2, 2, 2, 2, 2, 2, 2, 2, 2, 2, 2, 2, 2, 2, 2, 2, 2, 2, 2, 2, 2, 2, 2, 2, 2, 2, 2, 2, 2, 2, 2, 2, 2, 2, 2, 2, 2, 2, 2, 2, 2, 2, 2, 2, 2, 2, 2, 2, 2, 2, 2, 2, 2, 2, 2, 2, 2, 2, 2, 2, 2, 2, 2, 2, 2, 2, 2, 2, 2, 2, 2, 2, 2, 2, 2, 2, 2, 2, 2, 2, 2, 2, 2, 2, 2, 2, 2, 2, 2, 2, 2, 2, 2, 2, 2, 2, 2, 2, 2, 2, 2, 2, 2, 2, 2, 2, 2, 2, 2, 2, 2, 2, 2, 2, 2, 2, 2, 2, 2, 2, 2, 2, 2, 2, 2, 2, 2, 2, 2, 2, 2, 2, 2, 2, 2, 2, 2, 2, 2, 2, 2, 2, 2, 2, 2, 2, 2, 2, 2, 2, 2, 2, 2, 2, 2, 2, 2, 2, 2, 2, 2, 2, 2, 2, 2, 2, 2, 2, 2, 2, 2, 2, 2, 2, 2, 2, 2, 2, 2, 2, 2, 2, 2, 2, 2, 2, 2, 2, 2, 2, 2, 2, 2, 2, 2, 2, 2, 2, 2, 2, 2, 2, 2, 2, 2, 2, 2, 2, 2, 2, 2, 2, 2, 2, 2, 2, 2, 2, 2, 2, 2, 2, 2, 2, 2, 2, 2, 2, 2, 2, 2, 2, 2, 2, 2, 2, 2, 2, 2, 2, 2, 2, 2, 2, 2, 2, 2, 2, 2, 2, 2, 2, 2, 2, 2, 2, 2, 2, 2, 2, 2, 2, 2, 2, 2, 2, 2, 2, 2, 2, 2, 2, 2, 2, 2, 2, 2, 2, 2, 2, 2, 2, 2, 2, 2, 2, 2, 2, 2, 2, 2, 2, 2, 2, 2, 2, 2, 2, 2, 2, 2, 2, 2, 2, 2, 2, 2, 2, 2, 2, 2, 2, 2, 2, 2, 2, 2, 2, 2, 2, 2, 2, 2, 2, 2, 2, 2, 2, 2, 2, 2, 2, 2, 2, 2, 2, 2, 2, 2, 2, 2, 2, 2, 2, 2, 2, 2, 2, 2, 2, 2, 2, 2, 2, 2, 2, 2, 2, 2, 2, 2, 2, 2, 2, 2, 2, 2, 2, 2, 2, 2, 2, 2, 2, 2, 2, 2, 2, 2, 2, 2, 2, 2, 2, 2, 2, 2, 2, 2, 2, 2, 2, 2, 2, 2, 2, 4 ),
 ( 0.000000000000000000, 0.0004882812500000001084, 0.0009765625000000002168, 0.001464843750000000434, 0.001953125000000000000, 0.002441406250000000000, 0.002929687499999999566, 0.003417968749999999566, 0.003906249999999999133, 0.004394531249999998265, 0.004882812499999997398, 0.005371093749999997398, 0.005859374999999997398, 0.006347656249999998265, 0.006835937499999998265, 0.007324218749999998265, 0.007812499999999998265, 0.008300781249999998265, 0.008789062499999998265, 0.009277343749999998265, 0.009765624999999998265, 0.01025390624999999827, 0.01074218749999999827, 0.01123046874999999827, 0.01171874999999999827, 0.01220703125000000000, 0.01269531250000000000, 0.01318359375000000000, 0.01367187500000000000, 0.01416015625000000000, 0.01464843750000000000, 0.01513671875000000000, 0.01562500000000000000, 0.01611328125000000000, 0.01660156250000000000, 0.01708984375000000000, 0.01757812500000000000, 0.01806640625000000000, 0.01855468750000000000, 0.01904296875000000000, 0.01953125000000000000, 0.02001953125000000000, 0.02050781250000000000, 0.02099609375000000000, 0.02148437500000000000, 0.02197265625000000000, 0.02246093750000000000, 0.02294921875000000000, 0.02343750000000000000, 0.02392578125000000347, 0.02441406250000000347, 0.02490234375000000347, 0.02539062500000000347, 0.02587890625000000347, 0.02636718750000000347, 0.02685546875000000347, 0.02734375000000000347, 0.02783203125000000347, 0.02832031250000000347, 0.02880859375000000347, 0.02929687500000000347, 0.02978515625000000347, 0.03027343750000000347, 0.03076171875000000347, 0.03125000000000000000, 0.03173828125000000000, 0.03222656250000000000, 0.03271484375000000000, 0.03320312500000000000, 0.03369140625000000000, 0.03417968750000000000, 0.03466796875000000000, 0.03515625000000000000, 0.03564453125000000000, 0.03613281250000000000, 0.03662109375000000000, 0.03710937500000000000, 0.03759765625000000000, 0.03808593750000000000, 0.03857421875000000000, 0.03906250000000000000, 0.03955078125000000000, 0.04003906250000000000, 0.04052734375000000000, 0.04101562500000000000, 0.04150390625000000000, 0.04199218750000000000, 0.04248046875000000000, 0.04296875000000000000, 0.04345703125000000000, 0.04394531250000000000, 0.04443359375000000000, 0.04492187500000000000, 0.04541015625000000000, 0.04589843750000000000, 0.04638671875000000000, 0.04687500000000000000, 0.04736328125000000694, 0.04785156250000000694, 0.04833984375000000694, 0.04882812500000000694, 0.04931640625000000694, 0.04980468750000000694, 0.05029296875000000694, 0.05078125000000000694, 0.05126953125000000694, 0.05175781250000000694, 0.05224609375000000694, 0.05273437500000000694, 0.05322265625000000694, 0.05371093750000000694, 0.05419921875000000694, 0.05468750000000000694, 0.05517578125000000694, 0.05566406250000000694, 0.05615234375000000694, 0.05664062500000000694, 0.05712890625000000694, 0.05761718750000000694, 0.05810546875000000694, 0.05859375000000000694, 0.05908203125000000694, 0.05957031250000000694, 0.06005859375000000694, 0.06054687500000000694, 0.06103515625000000694, 0.06152343750000000694, 0.06201171875000000694, 0.06250000000000000000, 0.06298828125000000000, 0.06347656250000000000, 0.06396484375000000000, 0.06445312500000000000, 0.06494140625000000000, 0.06542968750000000000, 0.06591796875000000000, 0.06640625000000000000, 0.06689453125000000000, 0.06738281250000000000, 0.06787109375000000000, 0.06835937500000000000, 0.06884765625000000000, 0.06933593750000000000, 0.06982421875000000000, 0.07031250000000000000, 0.07080078125000000000, 0.07128906250000000000, 0.07177734375000000000, 0.07226562500000000000, 0.07275390625000000000, 0.07324218750000000000, 0.07373046875000000000, 0.07421875000000000000, 0.07470703125000000000, 0.07519531250000000000, 0.07568359375000000000, 0.07617187500000000000, 0.07666015625000000000, 0.07714843750000000000, 0.07763671875000000000, 0.07812500000000000000, 0.07861328125000000000, 0.07910156250000000000, 0.07958984375000000000, 0.08007812500000000000, 0.08056640625000000000, 0.08105468750000000000, 0.08154296875000000000, 0.08203125000000000000, 0.08251953125000000000, 0.08300781250000000000, 0.08349609375000000000, 0.08398437500000000000, 0.08447265625000000000, 0.08496093750000000000, 0.08544921875000000000, 0.08593750000000000000, 0.08642578125000000000, 0.08691406250000000000, 0.08740234375000000000, 0.08789062500000000000, 0.08837890625000000000, 0.08886718750000000000, 0.08935546875000000000, 0.08984375000000000000, 0.09033203125000000000, 0.09082031250000000000, 0.09130859375000000000, 0.09179687500000000000, 0.09228515625000000000, 0.09277343750000000000, 0.09326171875000000000, 0.09375000000000000000, 0.09423828125000001388, 0.09472656250000001388, 0.09521484375000001388, 0.09570312500000001388, 0.09619140625000001388, 0.09667968750000001388, 0.09716796875000001388, 0.09765625000000001388, 0.09814453125000001388, 0.09863281250000001388, 0.09912109375000001388, 0.09960937500000001388, 0.1000976562500000139, 0.1005859375000000139, 0.1010742187500000139, 0.1015625000000000139, 0.1020507812500000139, 0.1025390625000000139, 0.1030273437500000139, 0.1035156250000000139, 0.1040039062500000139, 0.1044921875000000139, 0.1049804687500000139, 0.1054687500000000139, 0.1059570312500000139, 0.1064453125000000139, 0.1069335937500000139, 0.1074218750000000139, 0.1079101562500000139, 0.1083984375000000139, 0.1088867187500000139, 0.1093750000000000139, 0.1098632812500000139, 0.1103515625000000139, 0.1108398437500000139, 0.1113281250000000139, 0.1118164062500000139, 0.1123046875000000139, 0.1127929687500000139, 0.1132812500000000139, 0.1137695312500000139, 0.1142578125000000139, 0.1147460937500000139, 0.1152343750000000139, 0.1157226562500000139, 0.1162109375000000139, 0.1166992187500000139, 0.1171875000000000139, 0.1176757812500000139, 0.1181640625000000139, 0.1186523437500000139, 0.1191406250000000139, 0.1196289062500000139, 0.1201171875000000139, 0.1206054687500000139, 0.1210937500000000139, 0.1215820312500000139, 0.1220703125000000139, 0.1225585937500000139, 0.1230468750000000139, 0.1235351562500000139, 0.1240234375000000139, 0.1245117187500000139, 0.1250000000000000000, 0.1254882812500000000, 0.1259765625000000000, 0.1264648437500000000, 0.1269531250000000000, 0.1274414062500000000, 0.1279296875000000000, 0.1284179687500000000, 0.1289062500000000000, 0.1293945312500000000, 0.1298828125000000000, 0.1303710937500000000, 0.1308593750000000000, 0.1313476562500000000, 0.1318359375000000000, 0.1323242187500000000, 0.1328125000000000000, 0.1333007812500000000, 0.1337890625000000000, 0.1342773437500000000, 0.1347656250000000000, 0.1352539062500000000, 0.1357421875000000000, 0.1362304687500000000, 0.1367187500000000000, 0.1372070312500000000, 0.1376953125000000000, 0.1381835937500000000, 0.1386718750000000000, 0.1391601562500000000, 0.1396484375000000000, 0.1401367187500000000, 0.1406250000000000000, 0.1411132812500000000, 0.1416015625000000000, 0.1420898437500000000, 0.1425781250000000000, 0.1430664062500000000, 0.1435546875000000000, 0.1440429687500000000, 0.1445312500000000000, 0.1450195312500000000, 0.1455078125000000000, 0.1459960937500000000, 0.1464843750000000000, 0.1469726562500000000, 0.1474609375000000000, 0.1479492187500000000, 0.1484375000000000000, 0.1489257812500000000, 0.1494140625000000000, 0.1499023437500000000, 0.1503906250000000000, 0.1508789062500000000, 0.1513671875000000000, 0.1518554687500000000, 0.1523437500000000000, 0.1528320312500000000, 0.1533203125000000000, 0.1538085937500000000, 0.1542968750000000000, 0.1547851562500000000, 0.1552734375000000000, 0.1557617187500000000, 0.1562500000000000000, 0.1567382812500000000, 0.1572265625000000000, 0.1577148437500000000, 0.1582031250000000000, 0.1586914062500000000, 0.1591796875000000000, 0.1596679687500000000, 0.1601562500000000000, 0.1606445312500000000, 0.1611328125000000000, 0.1616210937500000000, 0.1621093750000000000, 0.1625976562500000000, 0.1630859375000000000, 0.1635742187500000000, 0.1640625000000000000, 0.1645507812500000000, 0.1650390625000000000, 0.1655273437500000000, 0.1660156250000000000, 0.1665039062500000000, 0.1669921875000000000, 0.1674804687500000000, 0.1679687500000000000, 0.1684570312500000000, 0.1689453125000000000, 0.1694335937500000000, 0.1699218750000000000, 0.1704101562500000000, 0.1708984375000000000, 0.1713867187500000000, 0.1718750000000000000, 0.1723632812500000000, 0.1728515625000000000, 0.1733398437500000000, 0.1738281250000000000, 0.1743164062500000000, 0.1748046875000000000, 0.1752929687500000000, 0.1757812500000000000, 0.1762695312500000000, 0.1767578125000000000, 0.1772460937500000000, 0.1777343750000000000, 0.1782226562500000000, 0.1787109375000000000, 0.1791992187500000000, 0.1796875000000000000, 0.1801757812500000000, 0.1806640625000000000, 0.1811523437500000000, 0.1816406250000000000, 0.1821289062500000000, 0.1826171875000000000, 0.1831054687500000000, 0.1835937500000000000, 0.1840820312500000000, 0.1845703125000000000, 0.1850585937500000000, 0.1855468750000000000, 0.1860351562500000000, 0.1865234375000000000, 0.1870117187500000000, 0.1875000000000000000, 0.1879882812500000278, 0.1884765625000000278, 0.1889648437500000278, 0.1894531250000000278, 0.1899414062500000278, 0.1904296875000000278, 0.1909179687500000278, 0.1914062500000000278, 0.1918945312500000278, 0.1923828125000000278, 0.1928710937500000278, 0.1933593750000000278, 0.1938476562500000278, 0.1943359375000000278, 0.1948242187500000278, 0.1953125000000000278, 0.1958007812500000278, 0.1962890625000000278, 0.1967773437500000278, 0.1972656250000000278, 0.1977539062500000278, 0.1982421875000000278, 0.1987304687500000278, 0.1992187500000000278, 0.1997070312500000278, 0.2001953125000000278, 0.2006835937500000278, 0.2011718750000000278, 0.2016601562500000278, 0.2021484375000000278, 0.2026367187500000278, 0.2031250000000000278, 0.2036132812500000278, 0.2041015625000000278, 0.2045898437500000278, 0.2050781250000000278, 0.2055664062500000278, 0.2060546875000000278, 0.2065429687500000278, 0.2070312500000000278, 0.2075195312500000278, 0.2080078125000000278, 0.2084960937500000278, 0.2089843750000000278, 0.2094726562500000278, 0.2099609375000000278, 0.2104492187500000278, 0.2109375000000000278, 0.2114257812500000278, 0.2119140625000000278, 0.2124023437500000278, 0.2128906250000000278, 0.2133789062500000278, 0.2138671875000000278, 0.2143554687500000278, 0.2148437500000000278, 0.2153320312500000278, 0.2158203125000000278, 0.2163085937500000278, 0.2167968750000000278, 0.2172851562500000278, 0.2177734375000000278, 0.2182617187500000278, 0.2187500000000000278, 0.2192382812500000278, 0.2197265625000000278, 0.2202148437500000278, 0.2207031250000000278, 0.2211914062500000278, 0.2216796875000000278, 0.2221679687500000278, 0.2226562500000000278, 0.2231445312500000278, 0.2236328125000000278, 0.2241210937500000278, 0.2246093750000000278, 0.2250976562500000278, 0.2255859375000000278, 0.2260742187500000278, 0.2265625000000000278, 0.2270507812500000278, 0.2275390625000000278, 0.2280273437500000278, 0.2285156250000000278, 0.2290039062500000278, 0.2294921875000000278, 0.2299804687500000278, 0.2304687500000000278, 0.2309570312500000278, 0.2314453125000000278, 0.2319335937500000278, 0.2324218750000000278, 0.2329101562500000278, 0.2333984375000000278, 0.2338867187500000278, 0.2343750000000000278, 0.2348632812500000278, 0.2353515625000000278, 0.2358398437500000278, 0.2363281250000000278, 0.2368164062500000278, 0.2373046875000000278, 0.2377929687500000278, 0.2382812500000000278, 0.2387695312500000278, 0.2392578125000000278, 0.2397460937500000278, 0.2402343750000000278, 0.2407226562500000278, 0.2412109375000000278, 0.2416992187500000278, 0.2421875000000000278, 0.2426757812500000278, 0.2431640625000000278, 0.2436523437500000278, 0.2441406250000000278, 0.2446289062500000278, 0.2451171875000000278, 0.2456054687500000278, 0.2460937500000000278, 0.2465820312500000278, 0.2470703125000000278, 0.2475585937500000278, 0.2480468750000000278, 0.2485351562500000278, 0.2490234375000000278, 0.2495117187500000278, 0.2500000000000000000, 0.2504882812500000000, 0.2509765625000000000, 0.2514648437500000000, 0.2519531250000000000, 0.2524414062500000000, 0.2529296875000000000, 0.2534179687500000000, 0.2539062500000000000, 0.2543945312500000000, 0.2548828125000000000, 0.2553710937500000000, 0.2558593750000000000, 0.2563476562500000000, 0.2568359375000000000, 0.2573242187500000000, 0.2578125000000000000, 0.2583007812500000000, 0.2587890625000000000, 0.2592773437500000000, 0.2597656250000000000, 0.2602539062500000000, 0.2607421875000000000, 0.2612304687500000000, 0.2617187500000000000, 0.2622070312500000000, 0.2626953125000000000, 0.2631835937500000000, 0.2636718750000000000, 0.2641601562500000000, 0.2646484375000000000, 0.2651367187500000000, 0.2656250000000000000, 0.2661132812500000000, 0.2666015625000000000, 0.2670898437500000000, 0.2675781250000000000, 0.2680664062500000000, 0.2685546875000000000, 0.2690429687500000000, 0.2695312500000000000, 0.2700195312500000000, 0.2705078125000000000, 0.2709960937500000000, 0.2714843750000000000, 0.2719726562500000000, 0.2724609375000000000, 0.2729492187500000000, 0.2734375000000000000, 0.2739257812500000000, 0.2744140625000000000, 0.2749023437500000000, 0.2753906250000000000, 0.2758789062500000000, 0.2763671875000000000, 0.2768554687500000000, 0.2773437500000000000, 0.2778320312500000000, 0.2783203125000000000, 0.2788085937500000000, 0.2792968750000000000, 0.2797851562500000000, 0.2802734375000000000, 0.2807617187500000000, 0.2812500000000000000, 0.2817382812500000000, 0.2822265625000000000, 0.2827148437500000000, 0.2832031250000000000, 0.2836914062500000000, 0.2841796875000000000, 0.2846679687500000000, 0.2851562500000000000, 0.2856445312500000000, 0.2861328125000000000, 0.2866210937500000000, 0.2871093750000000000, 0.2875976562500000000, 0.2880859375000000000, 0.2885742187500000000, 0.2890625000000000000, 0.2895507812500000000, 0.2900390625000000000, 0.2905273437500000000, 0.2910156250000000000, 0.2915039062500000000, 0.2919921875000000000, 0.2924804687500000000, 0.2929687500000000000, 0.2934570312500000000, 0.2939453125000000000, 0.2944335937500000000, 0.2949218750000000000, 0.2954101562500000000, 0.2958984375000000000, 0.2963867187500000000, 0.2968750000000000000, 0.2973632812500000000, 0.2978515625000000000, 0.2983398437500000000, 0.2988281250000000000, 0.2993164062500000000, 0.2998046875000000000, 0.3002929687500000000, 0.3007812500000000000, 0.3012695312500000000, 0.3017578125000000000, 0.3022460937500000000, 0.3027343750000000000, 0.3032226562500000000, 0.3037109375000000000, 0.3041992187500000000, 0.3046875000000000000, 0.3051757812500000000, 0.3056640625000000000, 0.3061523437500000000, 0.3066406250000000000, 0.3071289062500000000, 0.3076171875000000000, 0.3081054687500000000, 0.3085937500000000000, 0.3090820312500000000, 0.3095703125000000000, 0.3100585937500000000, 0.3105468750000000000, 0.3110351562500000000, 0.3115234375000000000, 0.3120117187500000000, 0.3125000000000000000, 0.3129882812500000000, 0.3134765625000000000, 0.3139648437500000000, 0.3144531250000000000, 0.3149414062500000000, 0.3154296875000000000, 0.3159179687500000000, 0.3164062500000000000, 0.3168945312500000000, 0.3173828125000000000, 0.3178710937500000000, 0.3183593750000000000, 0.3188476562500000000, 0.3193359375000000000, 0.3198242187500000000, 0.3203125000000000000, 0.3208007812500000000, 0.3212890625000000000, 0.3217773437500000000, 0.3222656250000000000, 0.3227539062500000000, 0.3232421875000000000, 0.3237304687500000000, 0.3242187500000000000, 0.3247070312500000000, 0.3251953125000000000, 0.3256835937500000000, 0.3261718750000000000, 0.3266601562500000000, 0.3271484375000000000, 0.3276367187500000000, 0.3281250000000000000, 0.3286132812500000000, 0.3291015625000000000, 0.3295898437500000000, 0.3300781250000000000, 0.3305664062500000000, 0.3310546875000000000, 0.3315429687500000000, 0.3320312500000000000, 0.3325195312500000000, 0.3330078125000000000, 0.3334960937500000000, 0.3339843750000000000, 0.3344726562500000000, 0.3349609375000000000, 0.3354492187500000000, 0.3359375000000000000, 0.3364257812500000000, 0.3369140625000000000, 0.3374023437500000000, 0.3378906250000000000, 0.3383789062500000000, 0.3388671875000000000, 0.3393554687500000000, 0.3398437500000000000, 0.3403320312500000000, 0.3408203125000000000, 0.3413085937500000000, 0.3417968750000000000, 0.3422851562500000000, 0.3427734375000000000, 0.3432617187500000000, 0.3437500000000000000, 0.3442382812500000000, 0.3447265625000000000, 0.3452148437500000000, 0.3457031250000000000, 0.3461914062500000000, 0.3466796875000000000, 0.3471679687500000000, 0.3476562500000000000, 0.3481445312500000000, 0.3486328125000000000, 0.3491210937500000000, 0.3496093750000000000, 0.3500976562500000000, 0.3505859375000000000, 0.3510742187500000000, 0.3515625000000000000, 0.3520507812500000000, 0.3525390625000000000, 0.3530273437500000000, 0.3535156250000000000, 0.3540039062500000000, 0.3544921875000000000, 0.3549804687500000000, 0.3554687500000000000, 0.3559570312500000000, 0.3564453125000000000, 0.3569335937500000000, 0.3574218750000000000, 0.3579101562500000000, 0.3583984375000000000, 0.3588867187500000000, 0.3593750000000000000, 0.3598632812500000000, 0.3603515625000000000, 0.3608398437500000000, 0.3613281250000000000, 0.3618164062500000000, 0.3623046875000000000, 0.3627929687500000000, 0.3632812500000000000, 0.3637695312500000000, 0.3642578125000000000, 0.3647460937500000000, 0.3652343750000000000, 0.3657226562500000000, 0.3662109375000000000, 0.3666992187500000000, 0.3671875000000000000, 0.3676757812500000000, 0.3681640625000000000, 0.3686523437500000000, 0.3691406250000000000, 0.3696289062500000000, 0.3701171875000000000, 0.3706054687500000000, 0.3710937500000000000, 0.3715820312500000000, 0.3720703125000000000, 0.3725585937500000000, 0.3730468750000000000, 0.3735351562500000000, 0.3740234375000000000, 0.3745117187500000000, 0.3750000000000000000, 0.3754882812500000555, 0.3759765625000000555, 0.3764648437500000555, 0.3769531250000000555, 0.3774414062500000555, 0.3779296875000000555, 0.3784179687500000555, 0.3789062500000000555, 0.3793945312500000555, 0.3798828125000000555, 0.3803710937500000555, 0.3808593750000000555, 0.3813476562500000555, 0.3818359375000000555, 0.3823242187500000555, 0.3828125000000000555, 0.3833007812500000555, 0.3837890625000000555, 0.3842773437500000555, 0.3847656250000000555, 0.3852539062500000555, 0.3857421875000000555, 0.3862304687500000555, 0.3867187500000000555, 0.3872070312500000555, 0.3876953125000000555, 0.3881835937500000555, 0.3886718750000000555, 0.3891601562500000555, 0.3896484375000000555, 0.3901367187500000555, 0.3906250000000000555, 0.3911132812500000555, 0.3916015625000000555, 0.3920898437500000555, 0.3925781250000000555, 0.3930664062500000555, 0.3935546875000000555, 0.3940429687500000555, 0.3945312500000000555, 0.3950195312500000555, 0.3955078125000000555, 0.3959960937500000555, 0.3964843750000000555, 0.3969726562500000555, 0.3974609375000000555, 0.3979492187500000555, 0.3984375000000000555, 0.3989257812500000555, 0.3994140625000000555, 0.3999023437500000555, 0.4003906250000000555, 0.4008789062500000555, 0.4013671875000000555, 0.4018554687500000555, 0.4023437500000000555, 0.4028320312500000555, 0.4033203125000000555, 0.4038085937500000555, 0.4042968750000000555, 0.4047851562500000555, 0.4052734375000000555, 0.4057617187500000555, 0.4062500000000000555, 0.4067382812500000555, 0.4072265625000000555, 0.4077148437500000555, 0.4082031250000000555, 0.4086914062500000555, 0.4091796875000000555, 0.4096679687500000555, 0.4101562500000000555, 0.4106445312500000555, 0.4111328125000000555, 0.4116210937500000555, 0.4121093750000000555, 0.4125976562500000555, 0.4130859375000000555, 0.4135742187500000555, 0.4140625000000000555, 0.4145507812500000555, 0.4150390625000000555, 0.4155273437500000555, 0.4160156250000000555, 0.4165039062500000555, 0.4169921875000000555, 0.4174804687500000555, 0.4179687500000000555, 0.4184570312500000555, 0.4189453125000000555, 0.4194335937500000555, 0.4199218750000000555, 0.4204101562500000555, 0.4208984375000000555, 0.4213867187500000555, 0.4218750000000000555, 0.4223632812500000555, 0.4228515625000000555, 0.4233398437500000555, 0.4238281250000000555, 0.4243164062500000555, 0.4248046875000000555, 0.4252929687500000555, 0.4257812500000000555, 0.4262695312500000555, 0.4267578125000000555, 0.4272460937500000555, 0.4277343750000000555, 0.4282226562500000555, 0.4287109375000000555, 0.4291992187500000555, 0.4296875000000000555, 0.4301757812500000555, 0.4306640625000000555, 0.4311523437500000555, 0.4316406250000000555, 0.4321289062500000555, 0.4326171875000000555, 0.4331054687500000555, 0.4335937500000000555, 0.4340820312500000555, 0.4345703125000000555, 0.4350585937500000555, 0.4355468750000000555, 0.4360351562500000555, 0.4365234375000000555, 0.4370117187500000555, 0.4375000000000000555, 0.4379882812500000555, 0.4384765625000000555, 0.4389648437500000555, 0.4394531250000000555, 0.4399414062500000555, 0.4404296875000000555, 0.4409179687500000555, 0.4414062500000000555, 0.4418945312500000555, 0.4423828125000000555, 0.4428710937500000555, 0.4433593750000000555, 0.4438476562500000555, 0.4443359375000000555, 0.4448242187500000555, 0.4453125000000000555, 0.4458007812500000555, 0.4462890625000000555, 0.4467773437500000555, 0.4472656250000000555, 0.4477539062500000555, 0.4482421875000000555, 0.4487304687500000555, 0.4492187500000000555, 0.4497070312500000555, 0.4501953125000000555, 0.4506835937500000555, 0.4511718750000000555, 0.4516601562500000555, 0.4521484375000000555, 0.4526367187500000555, 0.4531250000000000555, 0.4536132812500000555, 0.4541015625000000555, 0.4545898437500000555, 0.4550781250000000555, 0.4555664062500000555, 0.4560546875000000555, 0.4565429687500000555, 0.4570312500000000555, 0.4575195312500000555, 0.4580078125000000555, 0.4584960937500000555, 0.4589843750000000555, 0.4594726562500000555, 0.4599609375000000555, 0.4604492187500000555, 0.4609375000000000555, 0.4614257812500000555, 0.4619140625000000555, 0.4624023437500000555, 0.4628906250000000555, 0.4633789062500000555, 0.4638671875000000555, 0.4643554687500000555, 0.4648437500000000555, 0.4653320312500000555, 0.4658203125000000555, 0.4663085937500000555, 0.4667968750000000555, 0.4672851562500000555, 0.4677734375000000555, 0.4682617187500000555, 0.4687500000000000555, 0.4692382812500000555, 0.4697265625000000555, 0.4702148437500000555, 0.4707031250000000555, 0.4711914062500000555, 0.4716796875000000555, 0.4721679687500000555, 0.4726562500000000555, 0.4731445312500000555, 0.4736328125000000555, 0.4741210937500000555, 0.4746093750000000555, 0.4750976562500000555, 0.4755859375000000555, 0.4760742187500000555, 0.4765625000000000555, 0.4770507812500000555, 0.4775390625000000555, 0.4780273437500000555, 0.4785156250000000555, 0.4790039062500000555, 0.4794921875000000555, 0.4799804687500000555, 0.4804687500000000555, 0.4809570312500000555, 0.4814453125000000555, 0.4819335937500000555, 0.4824218750000000555, 0.4829101562500000555, 0.4833984375000000555, 0.4838867187500000555, 0.4843750000000000555, 0.4848632812500000555, 0.4853515625000000555, 0.4858398437500000555, 0.4863281250000000555, 0.4868164062500000555, 0.4873046875000000555, 0.4877929687500000555, 0.4882812500000000555, 0.4887695312500000555, 0.4892578125000000555, 0.4897460937500000555, 0.4902343750000000555, 0.4907226562500000555, 0.4912109375000000555, 0.4916992187500000555, 0.4921875000000000555, 0.4926757812500000555, 0.4931640625000000555, 0.4936523437500000555, 0.4941406250000000555, 0.4946289062500000555, 0.4951171875000000555, 0.4956054687500000555, 0.4960937500000000555, 0.4965820312500000555, 0.4970703125000000555, 0.4975585937500000555, 0.4980468750000000555, 0.4985351562500000555, 0.4990234375000000555, 0.4995117187500000555, 0.5000000000000000000, 0.5004882812500000000, 0.5009765625000000000, 0.5014648437500000000, 0.5019531250000000000, 0.5024414062500000000, 0.5029296875000000000, 0.5034179687500000000, 0.5039062500000000000, 0.5043945312500000000, 0.5048828125000000000, 0.5053710937500000000, 0.5058593750000000000, 0.5063476562500000000, 0.5068359375000000000, 0.5073242187500000000, 0.5078125000000000000, 0.5083007812500000000, 0.5087890625000000000, 0.5092773437500000000, 0.5097656250000000000, 0.5102539062500000000, 0.5107421875000000000, 0.5112304687500000000, 0.5117187500000000000, 0.5122070312500000000, 0.5126953125000000000, 0.5131835937500000000, 0.5136718750000000000, 0.5141601562500000000, 0.5146484375000000000, 0.5151367187500000000, 0.5156250000000000000, 0.5161132812500000000, 0.5166015625000000000, 0.5170898437500000000, 0.5175781250000000000, 0.5180664062500000000, 0.5185546875000000000, 0.5190429687500000000, 0.5195312500000000000, 0.5200195312500000000, 0.5205078125000000000, 0.5209960937500000000, 0.5214843750000000000, 0.5219726562500000000, 0.5224609375000000000, 0.5229492187500000000, 0.5234375000000000000, 0.5239257812500000000, 0.5244140625000000000, 0.5249023437500000000, 0.5253906250000000000, 0.5258789062500000000, 0.5263671875000000000, 0.5268554687500000000, 0.5273437500000000000, 0.5278320312500000000, 0.5283203125000000000, 0.5288085937500000000, 0.5292968750000000000, 0.5297851562500000000, 0.5302734375000000000, 0.5307617187500000000, 0.5312500000000000000, 0.5317382812500000000, 0.5322265625000000000, 0.5327148437500000000, 0.5332031250000000000, 0.5336914062500000000, 0.5341796875000000000, 0.5346679687500000000, 0.5351562500000000000, 0.5356445312500000000, 0.5361328125000000000, 0.5366210937500000000, 0.5371093750000000000, 0.5375976562500000000, 0.5380859375000000000, 0.5385742187500000000, 0.5390625000000000000, 0.5395507812500000000, 0.5400390625000000000, 0.5405273437500000000, 0.5410156250000000000, 0.5415039062500000000, 0.5419921875000000000, 0.5424804687500000000, 0.5429687500000000000, 0.5434570312500000000, 0.5439453125000000000, 0.5444335937500000000, 0.5449218750000000000, 0.5454101562500000000, 0.5458984375000000000, 0.5463867187500000000, 0.5468750000000000000, 0.5473632812500000000, 0.5478515625000000000, 0.5483398437500000000, 0.5488281250000000000, 0.5493164062500000000, 0.5498046875000000000, 0.5502929687500000000, 0.5507812500000000000, 0.5512695312500000000, 0.5517578125000000000, 0.5522460937500000000, 0.5527343750000000000, 0.5532226562500000000, 0.5537109375000000000, 0.5541992187500000000, 0.5546875000000000000, 0.5551757812500000000, 0.5556640625000000000, 0.5561523437500000000, 0.5566406250000000000, 0.5571289062500000000, 0.5576171875000000000, 0.5581054687500000000, 0.5585937500000000000, 0.5590820312500000000, 0.5595703125000000000, 0.5600585937500000000, 0.5605468750000000000, 0.5610351562500000000, 0.5615234375000000000, 0.5620117187500000000, 0.5625000000000000000, 0.5629882812500000000, 0.5634765625000000000, 0.5639648437500000000, 0.5644531250000000000, 0.5649414062500000000, 0.5654296875000000000, 0.5659179687500000000, 0.5664062500000000000, 0.5668945312500000000, 0.5673828125000000000, 0.5678710937500000000, 0.5683593750000000000, 0.5688476562500000000, 0.5693359375000000000, 0.5698242187500000000, 0.5703125000000000000, 0.5708007812500000000, 0.5712890625000000000, 0.5717773437500000000, 0.5722656250000000000, 0.5727539062500000000, 0.5732421875000000000, 0.5737304687500000000, 0.5742187500000000000, 0.5747070312500000000, 0.5751953125000000000, 0.5756835937500000000, 0.5761718750000000000, 0.5766601562500000000, 0.5771484375000000000, 0.5776367187500000000, 0.5781250000000000000, 0.5786132812500000000, 0.5791015625000000000, 0.5795898437500000000, 0.5800781250000000000, 0.5805664062500000000, 0.5810546875000000000, 0.5815429687500000000, 0.5820312500000000000, 0.5825195312500000000, 0.5830078125000000000, 0.5834960937500000000, 0.5839843750000000000, 0.5844726562500000000, 0.5849609375000000000, 0.5854492187500000000, 0.5859375000000000000, 0.5864257812500000000, 0.5869140625000000000, 0.5874023437500000000, 0.5878906250000000000, 0.5883789062500000000, 0.5888671875000000000, 0.5893554687500000000, 0.5898437500000000000, 0.5903320312500000000, 0.5908203125000000000, 0.5913085937500000000, 0.5917968750000000000, 0.5922851562500000000, 0.5927734375000000000, 0.5932617187500000000, 0.5937500000000000000, 0.5942382812500000000, 0.5947265625000000000, 0.5952148437500000000, 0.5957031250000000000, 0.5961914062500000000, 0.5966796875000000000, 0.5971679687500000000, 0.5976562500000000000, 0.5981445312500000000, 0.5986328125000000000, 0.5991210937500000000, 0.5996093750000000000, 0.6000976562500000000, 0.6005859375000000000, 0.6010742187500000000, 0.6015625000000000000, 0.6020507812500000000, 0.6025390625000000000, 0.6030273437500000000, 0.6035156250000000000, 0.6040039062500000000, 0.6044921875000000000, 0.6049804687500000000, 0.6054687500000000000, 0.6059570312500000000, 0.6064453125000000000, 0.6069335937500000000, 0.6074218750000000000, 0.6079101562500000000, 0.6083984375000000000, 0.6088867187500000000, 0.6093750000000000000, 0.6098632812500000000, 0.6103515625000000000, 0.6108398437500000000, 0.6113281250000000000, 0.6118164062500000000, 0.6123046875000000000, 0.6127929687500000000, 0.6132812500000000000, 0.6137695312500000000, 0.6142578125000000000, 0.6147460937500000000, 0.6152343750000000000, 0.6157226562500000000, 0.6162109375000000000, 0.6166992187500000000, 0.6171875000000000000, 0.6176757812500000000, 0.6181640625000000000, 0.6186523437500000000, 0.6191406250000000000, 0.6196289062500000000, 0.6201171875000000000, 0.6206054687500000000, 0.6210937500000000000, 0.6215820312500000000, 0.6220703125000000000, 0.6225585937500000000, 0.6230468750000000000, 0.6235351562500000000, 0.6240234375000000000, 0.6245117187500000000, 0.6250000000000000000, 0.6254882812500000000, 0.6259765625000000000, 0.6264648437500000000, 0.6269531250000000000, 0.6274414062500000000, 0.6279296875000000000, 0.6284179687500000000, 0.6289062500000000000, 0.6293945312500000000, 0.6298828125000000000, 0.6303710937500000000, 0.6308593750000000000, 0.6313476562500000000, 0.6318359375000000000, 0.6323242187500000000, 0.6328125000000000000, 0.6333007812500000000, 0.6337890625000000000, 0.6342773437500000000, 0.6347656250000000000, 0.6352539062500000000, 0.6357421875000000000, 0.6362304687500000000, 0.6367187500000000000, 0.6372070312500000000, 0.6376953125000000000, 0.6381835937500000000, 0.6386718750000000000, 0.6391601562500000000, 0.6396484375000000000, 0.6401367187500000000, 0.6406250000000000000, 0.6411132812500000000, 0.6416015625000000000, 0.6420898437500000000, 0.6425781250000000000, 0.6430664062500000000, 0.6435546875000000000, 0.6440429687500000000, 0.6445312500000000000, 0.6450195312500000000, 0.6455078125000000000, 0.6459960937500000000, 0.6464843750000000000, 0.6469726562500000000, 0.6474609375000000000, 0.6479492187500000000, 0.6484375000000000000, 0.6489257812500000000, 0.6494140625000000000, 0.6499023437500000000, 0.6503906250000000000, 0.6508789062500000000, 0.6513671875000000000, 0.6518554687500000000, 0.6523437500000000000, 0.6528320312500000000, 0.6533203125000000000, 0.6538085937500000000, 0.6542968750000000000, 0.6547851562500000000, 0.6552734375000000000, 0.6557617187500000000, 0.6562500000000000000, 0.6567382812500000000, 0.6572265625000000000, 0.6577148437500000000, 0.6582031250000000000, 0.6586914062500000000, 0.6591796875000000000, 0.6596679687500000000, 0.6601562500000000000, 0.6606445312500000000, 0.6611328125000000000, 0.6616210937500000000, 0.6621093750000000000, 0.6625976562500000000, 0.6630859375000000000, 0.6635742187500000000, 0.6640625000000000000, 0.6645507812500000000, 0.6650390625000000000, 0.6655273437500000000, 0.6660156250000000000, 0.6665039062500000000, 0.6669921875000000000, 0.6674804687500000000, 0.6679687500000000000, 0.6684570312500000000, 0.6689453125000000000, 0.6694335937500000000, 0.6699218750000000000, 0.6704101562500000000, 0.6708984375000000000, 0.6713867187500000000, 0.6718750000000000000, 0.6723632812500000000, 0.6728515625000000000, 0.6733398437500000000, 0.6738281250000000000, 0.6743164062500000000, 0.6748046875000000000, 0.6752929687500000000, 0.6757812500000000000, 0.6762695312500000000, 0.6767578125000000000, 0.6772460937500000000, 0.6777343750000000000, 0.6782226562500000000, 0.6787109375000000000, 0.6791992187500000000, 0.6796875000000000000, 0.6801757812500000000, 0.6806640625000000000, 0.6811523437500000000, 0.6816406250000000000, 0.6821289062500000000, 0.6826171875000000000, 0.6831054687500000000, 0.6835937500000000000, 0.6840820312500000000, 0.6845703125000000000, 0.6850585937500000000, 0.6855468750000000000, 0.6860351562500000000, 0.6865234375000000000, 0.6870117187500000000, 0.6875000000000000000, 0.6879882812500000000, 0.6884765625000000000, 0.6889648437500000000, 0.6894531250000000000, 0.6899414062500000000, 0.6904296875000000000, 0.6909179687500000000, 0.6914062500000000000, 0.6918945312500000000, 0.6923828125000000000, 0.6928710937500000000, 0.6933593750000000000, 0.6938476562500000000, 0.6943359375000000000, 0.6948242187500000000, 0.6953125000000000000, 0.6958007812500000000, 0.6962890625000000000, 0.6967773437500000000, 0.6972656250000000000, 0.6977539062500000000, 0.6982421875000000000, 0.6987304687500000000, 0.6992187500000000000, 0.6997070312500000000, 0.7001953125000000000, 0.7006835937500000000, 0.7011718750000000000, 0.7016601562500000000, 0.7021484375000000000, 0.7026367187500000000, 0.7031250000000000000, 0.7036132812500000000, 0.7041015625000000000, 0.7045898437500000000, 0.7050781250000000000, 0.7055664062500000000, 0.7060546875000000000, 0.7065429687500000000, 0.7070312500000000000, 0.7075195312500000000, 0.7080078125000000000, 0.7084960937500000000, 0.7089843750000000000, 0.7094726562500000000, 0.7099609375000000000, 0.7104492187500000000, 0.7109375000000000000, 0.7114257812500000000, 0.7119140625000000000, 0.7124023437500000000, 0.7128906250000000000, 0.7133789062500000000, 0.7138671875000000000, 0.7143554687500000000, 0.7148437500000000000, 0.7153320312500000000, 0.7158203125000000000, 0.7163085937500000000, 0.7167968750000000000, 0.7172851562500000000, 0.7177734375000000000, 0.7182617187500000000, 0.7187500000000000000, 0.7192382812500000000, 0.7197265625000000000, 0.7202148437500000000, 0.7207031250000000000, 0.7211914062500000000, 0.7216796875000000000, 0.7221679687500000000, 0.7226562500000000000, 0.7231445312500000000, 0.7236328125000000000, 0.7241210937500000000, 0.7246093750000000000, 0.7250976562500000000, 0.7255859375000000000, 0.7260742187500000000, 0.7265625000000000000, 0.7270507812500000000, 0.7275390625000000000, 0.7280273437500000000, 0.7285156250000000000, 0.7290039062500000000, 0.7294921875000000000, 0.7299804687500000000, 0.7304687500000000000, 0.7309570312500000000, 0.7314453125000000000, 0.7319335937500000000, 0.7324218750000000000, 0.7329101562500000000, 0.7333984375000000000, 0.7338867187500000000, 0.7343750000000000000, 0.7348632812500000000, 0.7353515625000000000, 0.7358398437500000000, 0.7363281250000000000, 0.7368164062500000000, 0.7373046875000000000, 0.7377929687500000000, 0.7382812500000000000, 0.7387695312500000000, 0.7392578125000000000, 0.7397460937500000000, 0.7402343750000000000, 0.7407226562500000000, 0.7412109375000000000, 0.7416992187500000000, 0.7421875000000000000, 0.7426757812500000000, 0.7431640625000000000, 0.7436523437500000000, 0.7441406250000000000, 0.7446289062500000000, 0.7451171875000000000, 0.7456054687500000000, 0.7460937500000000000, 0.7465820312500000000, 0.7470703125000000000, 0.7475585937500000000, 0.7480468750000000000, 0.7485351562500000000, 0.7490234375000000000, 0.7495117187500000000, 0.7500000000000000000, 0.7504882812500001110, 0.7509765625000001110, 0.7514648437500001110, 0.7519531250000001110, 0.7524414062500001110, 0.7529296875000001110, 0.7534179687500001110, 0.7539062500000001110, 0.7543945312500001110, 0.7548828125000001110, 0.7553710937500001110, 0.7558593750000001110, 0.7563476562500001110, 0.7568359375000001110, 0.7573242187500001110, 0.7578125000000001110, 0.7583007812500001110, 0.7587890625000001110, 0.7592773437500001110, 0.7597656250000001110, 0.7602539062500001110, 0.7607421875000001110, 0.7612304687500001110, 0.7617187500000001110, 0.7622070312500001110, 0.7626953125000001110, 0.7631835937500001110, 0.7636718750000001110, 0.7641601562500001110, 0.7646484375000001110, 0.7651367187500001110, 0.7656250000000001110, 0.7661132812500001110, 0.7666015625000001110, 0.7670898437500001110, 0.7675781250000001110, 0.7680664062500001110, 0.7685546875000001110, 0.7690429687500001110, 0.7695312500000001110, 0.7700195312500001110, 0.7705078125000001110, 0.7709960937500001110, 0.7714843750000001110, 0.7719726562500001110, 0.7724609375000001110, 0.7729492187500001110, 0.7734375000000001110, 0.7739257812500001110, 0.7744140625000001110, 0.7749023437500001110, 0.7753906250000001110, 0.7758789062500001110, 0.7763671875000001110, 0.7768554687500001110, 0.7773437500000001110, 0.7778320312500001110, 0.7783203125000001110, 0.7788085937500001110, 0.7792968750000001110, 0.7797851562500001110, 0.7802734375000001110, 0.7807617187500001110, 0.7812500000000001110, 0.7817382812500001110, 0.7822265625000001110, 0.7827148437500001110, 0.7832031250000001110, 0.7836914062500001110, 0.7841796875000001110, 0.7846679687500001110, 0.7851562500000001110, 0.7856445312500001110, 0.7861328125000001110, 0.7866210937500001110, 0.7871093750000001110, 0.7875976562500001110, 0.7880859375000001110, 0.7885742187500001110, 0.7890625000000001110, 0.7895507812500001110, 0.7900390625000001110, 0.7905273437500001110, 0.7910156250000001110, 0.7915039062500001110, 0.7919921875000001110, 0.7924804687500001110, 0.7929687500000001110, 0.7934570312500001110, 0.7939453125000001110, 0.7944335937500001110, 0.7949218750000001110, 0.7954101562500001110, 0.7958984375000001110, 0.7963867187500001110, 0.7968750000000001110, 0.7973632812500001110, 0.7978515625000001110, 0.7983398437500001110, 0.7988281250000001110, 0.7993164062500001110, 0.7998046875000001110, 0.8002929687500001110, 0.8007812500000001110, 0.8012695312500001110, 0.8017578125000001110, 0.8022460937500001110, 0.8027343750000001110, 0.8032226562500001110, 0.8037109375000001110, 0.8041992187500001110, 0.8046875000000001110, 0.8051757812500001110, 0.8056640625000001110, 0.8061523437500001110, 0.8066406250000001110, 0.8071289062500001110, 0.8076171875000001110, 0.8081054687500001110, 0.8085937500000001110, 0.8090820312500001110, 0.8095703125000001110, 0.8100585937500001110, 0.8105468750000001110, 0.8110351562500001110, 0.8115234375000001110, 0.8120117187500001110, 0.8125000000000001110, 0.8129882812500001110, 0.8134765625000001110, 0.8139648437500001110, 0.8144531250000001110, 0.8149414062500001110, 0.8154296875000001110, 0.8159179687500001110, 0.8164062500000001110, 0.8168945312500001110, 0.8173828125000001110, 0.8178710937500001110, 0.8183593750000001110, 0.8188476562500001110, 0.8193359375000001110, 0.8198242187500001110, 0.8203125000000001110, 0.8208007812500001110, 0.8212890625000001110, 0.8217773437500001110, 0.8222656250000001110, 0.8227539062500001110, 0.8232421875000001110, 0.8237304687500001110, 0.8242187500000001110, 0.8247070312500001110, 0.8251953125000001110, 0.8256835937500001110, 0.8261718750000001110, 0.8266601562500001110, 0.8271484375000001110, 0.8276367187500001110, 0.8281250000000001110, 0.8286132812500001110, 0.8291015625000001110, 0.8295898437500001110, 0.8300781250000001110, 0.8305664062500001110, 0.8310546875000001110, 0.8315429687500001110, 0.8320312500000001110, 0.8325195312500001110, 0.8330078125000001110, 0.8334960937500001110, 0.8339843750000001110, 0.8344726562500001110, 0.8349609375000001110, 0.8354492187500001110, 0.8359375000000001110, 0.8364257812500001110, 0.8369140625000001110, 0.8374023437500001110, 0.8378906250000001110, 0.8383789062500001110, 0.8388671875000001110, 0.8393554687500001110, 0.8398437500000001110, 0.8403320312500001110, 0.8408203125000001110, 0.8413085937500001110, 0.8417968750000001110, 0.8422851562500001110, 0.8427734375000001110, 0.8432617187500001110, 0.8437500000000001110, 0.8442382812500001110, 0.8447265625000001110, 0.8452148437500001110, 0.8457031250000001110, 0.8461914062500001110, 0.8466796875000001110, 0.8471679687500001110, 0.8476562500000001110, 0.8481445312500001110, 0.8486328125000001110, 0.8491210937500001110, 0.8496093750000001110, 0.8500976562500001110, 0.8505859375000001110, 0.8510742187500001110, 0.8515625000000001110, 0.8520507812500001110, 0.8525390625000001110, 0.8530273437500001110, 0.8535156250000001110, 0.8540039062500001110, 0.8544921875000001110, 0.8549804687500001110, 0.8554687500000001110, 0.8559570312500001110, 0.8564453125000001110, 0.8569335937500001110, 0.8574218750000001110, 0.8579101562500001110, 0.8583984375000001110, 0.8588867187500001110, 0.8593750000000001110, 0.8598632812500001110, 0.8603515625000001110, 0.8608398437500001110, 0.8613281250000001110, 0.8618164062500001110, 0.8623046875000001110, 0.8627929687500001110, 0.8632812500000001110, 0.8637695312500001110, 0.8642578125000001110, 0.8647460937500001110, 0.8652343750000001110, 0.8657226562500001110, 0.8662109375000001110, 0.8666992187500001110, 0.8671875000000001110, 0.8676757812500001110, 0.8681640625000001110, 0.8686523437500001110, 0.8691406250000001110, 0.8696289062500001110, 0.8701171875000001110, 0.8706054687500001110, 0.8710937500000001110, 0.8715820312500001110, 0.8720703125000001110, 0.8725585937500001110, 0.8730468750000001110, 0.8735351562500001110, 0.8740234375000001110, 0.8745117187500001110, 0.8750000000000001110, 0.8754882812500001110, 0.8759765625000001110, 0.8764648437500001110, 0.8769531250000001110, 0.8774414062500001110, 0.8779296875000001110, 0.8784179687500001110, 0.8789062500000001110, 0.8793945312500001110, 0.8798828125000001110, 0.8803710937500001110, 0.8808593750000001110, 0.8813476562500001110, 0.8818359375000001110, 0.8823242187500001110, 0.8828125000000001110, 0.8833007812500001110, 0.8837890625000001110, 0.8842773437500001110, 0.8847656250000001110, 0.8852539062500001110, 0.8857421875000001110, 0.8862304687500001110, 0.8867187500000001110, 0.8872070312500001110, 0.8876953125000001110, 0.8881835937500001110, 0.8886718750000001110, 0.8891601562500001110, 0.8896484375000001110, 0.8901367187500001110, 0.8906250000000001110, 0.8911132812500001110, 0.8916015625000001110, 0.8920898437500001110, 0.8925781250000001110, 0.8930664062500001110, 0.8935546875000001110, 0.8940429687500001110, 0.8945312500000001110, 0.8950195312500001110, 0.8955078125000001110, 0.8959960937500001110, 0.8964843750000001110, 0.8969726562500001110, 0.8974609375000001110, 0.8979492187500001110, 0.8984375000000001110, 0.8989257812500001110, 0.8994140625000001110, 0.8999023437500001110, 0.9003906250000001110, 0.9008789062500001110, 0.9013671875000001110, 0.9018554687500001110, 0.9023437500000001110, 0.9028320312500001110, 0.9033203125000001110, 0.9038085937500001110, 0.9042968750000001110, 0.9047851562500001110, 0.9052734375000001110, 0.9057617187500001110, 0.9062500000000001110, 0.9067382812500001110, 0.9072265625000001110, 0.9077148437500001110, 0.9082031250000001110, 0.9086914062500001110, 0.9091796875000001110, 0.9096679687500001110, 0.9101562500000001110, 0.9106445312500001110, 0.9111328125000001110, 0.9116210937500001110, 0.9121093750000001110, 0.9125976562500001110, 0.9130859375000001110, 0.9135742187500001110, 0.9140625000000001110, 0.9145507812500001110, 0.9150390625000001110, 0.9155273437500001110, 0.9160156250000001110, 0.9165039062500001110, 0.9169921875000001110, 0.9174804687500001110, 0.9179687500000001110, 0.9184570312500001110, 0.9189453125000001110, 0.9194335937500001110, 0.9199218750000001110, 0.9204101562500001110, 0.9208984375000001110, 0.9213867187500001110, 0.9218750000000001110, 0.9223632812500001110, 0.9228515625000001110, 0.9233398437500001110, 0.9238281250000001110, 0.9243164062500001110, 0.9248046875000001110, 0.9252929687500001110, 0.9257812500000001110, 0.9262695312500001110, 0.9267578125000001110, 0.9272460937500001110, 0.9277343750000001110, 0.9282226562500001110, 0.9287109375000001110, 0.9291992187500001110, 0.9296875000000001110, 0.9301757812500001110, 0.9306640625000001110, 0.9311523437500001110, 0.9316406250000001110, 0.9321289062500001110, 0.9326171875000001110, 0.9331054687500001110, 0.9335937500000001110, 0.9340820312500001110, 0.9345703125000001110, 0.9350585937500001110, 0.9355468750000001110, 0.9360351562500001110, 0.9365234375000001110, 0.9370117187500001110, 0.9375000000000001110, 0.9379882812500001110, 0.9384765625000001110, 0.9389648437500001110, 0.9394531250000001110, 0.9399414062500001110, 0.9404296875000001110, 0.9409179687500001110, 0.9414062500000001110, 0.9418945312500001110, 0.9423828125000001110, 0.9428710937500001110, 0.9433593750000001110, 0.9438476562500001110, 0.9443359375000001110, 0.9448242187500001110, 0.9453125000000001110, 0.9458007812500001110, 0.9462890625000001110, 0.9467773437500001110, 0.9472656250000001110, 0.9477539062500001110, 0.9482421875000001110, 0.9487304687500001110, 0.9492187500000001110, 0.9497070312500001110, 0.9501953125000001110, 0.9506835937500001110, 0.9511718750000001110, 0.9516601562500001110, 0.9521484375000001110, 0.9526367187500001110, 0.9531250000000001110, 0.9536132812500001110, 0.9541015625000001110, 0.9545898437500001110, 0.9550781250000001110, 0.9555664062500001110, 0.9560546875000001110, 0.9565429687500001110, 0.9570312500000001110, 0.9575195312500001110, 0.9580078125000001110, 0.9584960937500001110, 0.9589843750000001110, 0.9594726562500001110, 0.9599609375000001110, 0.9604492187500001110, 0.9609375000000001110, 0.9614257812500001110, 0.9619140625000001110, 0.9624023437500001110, 0.9628906250000001110, 0.9633789062500001110, 0.9638671875000001110, 0.9643554687500001110, 0.9648437500000001110, 0.9653320312500001110, 0.9658203125000001110, 0.9663085937500001110, 0.9667968750000001110, 0.9672851562500001110, 0.9677734375000001110, 0.9682617187500001110, 0.9687500000000001110, 0.9692382812500001110, 0.9697265625000001110, 0.9702148437500001110, 0.9707031250000001110, 0.9711914062500001110, 0.9716796875000001110, 0.9721679687500001110, 0.9726562500000001110, 0.9731445312500001110, 0.9736328125000001110, 0.9741210937500001110, 0.9746093750000001110, 0.9750976562500001110, 0.9755859375000001110, 0.9760742187500001110, 0.9765625000000001110, 0.9770507812500001110, 0.9775390625000001110, 0.9780273437500001110, 0.9785156250000001110, 0.9790039062500001110, 0.9794921875000001110, 0.9799804687500001110, 0.9804687500000001110, 0.9809570312500001110, 0.9814453125000001110, 0.9819335937500001110, 0.9824218750000001110, 0.9829101562500001110, 0.9833984375000001110, 0.9838867187500001110, 0.9843750000000001110, 0.9848632812500001110, 0.9853515625000001110, 0.9858398437500001110, 0.9863281250000001110, 0.9868164062500001110, 0.9873046875000001110, 0.9877929687500001110, 0.9882812500000001110, 0.9887695312500001110, 0.9892578125000001110, 0.9897460937500001110, 0.9902343750000001110, 0.9907226562500001110, 0.9912109375000001110, 0.9916992187500001110, 0.9921875000000001110, 0.9926757812500001110, 0.9931640625000001110, 0.9936523437500001110, 0.9941406250000001110, 0.9946289062500001110, 0.9951171875000001110, 0.9956054687500001110, 0.9960937500000001110, 0.9965820312500001110, 0.9970703125000001110, 0.9975585937500001110, 0.9980468750000001110, 0.9985351562500001110, 0.9990234375000001110, 0.9995117187500001110, 1.000000000000000000 ),
 .UNSPECIFIED. ) ;
#78053 = DIRECTION ( 'NONE',  ( -0.06283980576413537855, -0.000000000000000000, -0.9980236263794188822 ) ) ;
#78054 = DIRECTION ( 'NONE',  ( -0.000000000000000000, 1.000000000000000000, -0.000000000000000000 ) ) ;
#78055 = CARTESIAN_POINT ( 'NONE',  ( 19.22361159462649027, -4.937694622890139939, 11.49999999999999645 ) ) ;
#78056 = CARTESIAN_POINT ( 'NONE',  ( -48.62287095715004881, -24.65952944569303895, 1.056160979905692798 ) ) ;
#78057 = CARTESIAN_POINT ( 'NONE',  ( 8.456965425111590662, -0.2003331576018148041, 3.712238059855193839 ) ) ;
#78058 = PLANE ( 'NONE',  #30981 ) ;
#78059 = EDGE_CURVE ( 'NONE', #74051, #84269, #16307, .T. ) ;
#78060 = VERTEX_POINT ( 'NONE', #63009 ) ;
#78061 = FACE_OUTER_BOUND ( 'NONE', #41878, .T. ) ;
#78062 = CARTESIAN_POINT ( 'NONE',  ( -80.52287095715006160, -23.47596703998600631, 11.44779298504228571 ) ) ;
#78064 = CARTESIAN_POINT ( 'NONE',  ( -51.60452015029387951, -25.10935914944338165, 3.558373330915750810 ) ) ;
#78063 = LOCAL_TIME ( 0, 54, 15.00000000000000000, #87585 ) ;
#78065 = CARTESIAN_POINT ( 'NONE',  ( -2.129050106866105185, 21.58297100922832357, 11.49999999999998934 ) ) ;
#78066 = CARTESIAN_POINT ( 'NONE',  ( -29.62287095715006302, -23.87261080661619062, 10.65372852762611622 ) ) ;
#78067 = CARTESIAN_POINT ( 'NONE',  ( 8.918240691521024388, 17.32521578647535776, -1.500000000000002220 ) ) ;
#78068 = FACE_OUTER_BOUND ( 'NONE', #76218, .T. ) ;
#78069 = VECTOR ( 'NONE', #10814, 1000.000000000000000 ) ;
#78070 = ORIENTED_EDGE ( 'NONE', *, *, #9170, .F. ) ;
#78071 = LOCAL_TIME ( 0, 54, 15.00000000000000000, #62616 ) ;
#78072 = CARTESIAN_POINT ( 'NONE',  ( -9.549598871097368047, 18.00506641634745009, 11.49999999999999645 ) ) ;
#78073 = CARTESIAN_POINT ( 'NONE',  ( -80.62882275262062137, -24.73486907724918282, 1.287355809206963908 ) ) ;
#78074 = EDGE_CURVE ( 'NONE', #52671, #5568, #38287, .T. ) ;
#78075 = DIRECTION ( 'NONE',  ( 0.000000000000000000, 0.9999999999976377785, 2.173523156925979975E-06 ) ) ;
#78076 = EDGE_CURVE ( 'NONE', #76732, #59182, #56479, .T. ) ;
#78077 = ORIENTED_EDGE ( 'NONE', *, *, #40849, .T. ) ;
#78078 = DIRECTION ( 'NONE',  ( 0.7071067811865513475, -0.7071067811865437980, 0.000000000000000000 ) ) ;
#78079 = CARTESIAN_POINT ( 'NONE',  ( -35.62287095715005592, -29.50250243563736774, 8.947779886222148704 ) ) ;
#78080 = CARTESIAN_POINT ( 'NONE',  ( -48.87380231474225667, -25.25214687568168870, 6.137092009077116828 ) ) ;
#78081 = CARTESIAN_POINT ( 'NONE',  ( -40.47157810787772547, -24.92592662359560762, 8.075495903017996469 ) ) ;
#78082 = PLANE ( 'NONE',  #20327 ) ;
#78083 = CARTESIAN_POINT ( 'NONE',  ( 10.01938154005162218, -17.43019892170380913, 11.49999999999998934 ) ) ;
#78084 = EDGE_CURVE ( 'NONE', #33683, #94497, #86326, .T. ) ;
#78085 = CARTESIAN_POINT ( 'NONE',  ( -45.62287095715004881, -23.47593901973091235, -1.443836447539009749 ) ) ;
#78086 = ORIENTED_EDGE ( 'NONE', *, *, #34917, .F. ) ;
#78087 = CARTESIAN_POINT ( 'NONE',  ( -36.52287095715006870, -23.47593901973090169, -1.443836447538997314 ) ) ;
#78088 = EDGE_CURVE ( 'NONE', #70270, #95088, #48021, .T. ) ;
#78089 = CARTESIAN_POINT ( 'NONE',  ( 21.91704834537361180, 6.644925864936762849, 11.49999999999999645 ) ) ;
#78090 = CARTESIAN_POINT ( 'NONE',  ( 18.72737137862276313, -12.84423604280260278, 11.49999999999998934 ) ) ;
#78091 = VERTEX_POINT ( 'NONE', #56902 ) ;
#78092 = CARTESIAN_POINT ( 'NONE',  ( -53.62287095715005592, -24.66019654487199375, 8.947790411086135265 ) ) ;
#78093 = CARTESIAN_POINT ( 'NONE',  ( -95.52287095715006160, -29.50248789122583659, 2.256150453626215580 ) ) ;
#78094 = CARTESIAN_POINT ( 'NONE',  ( -39.45282898296882479, -25.27930806443914591, 4.061648798908704450 ) ) ;
#78095 = CARTESIAN_POINT ( 'NONE',  ( -30.57287095715005520, -25.10878950975746804, 7.249410248868700002 ) ) ;
#78096 = CARTESIAN_POINT ( 'NONE',  ( -128.5901391630868318, -23.73791477778912196, 11.05961554403169522 ) ) ;
#78097 = AXIS2_PLACEMENT_3D ( 'NONE', #100355, #53724, #84655 ) ;
#78098 = B_SPLINE_CURVE_WITH_KNOTS ( 'NONE', 3,
 ( #60207, #20129, #89647, #13504 ),
 .UNSPECIFIED., .F., .F.,
 ( 4, 4 ),
 ( 0.000000000000000000, 9.999999999998206125E-05 ),
 .UNSPECIFIED. ) ;
#78099 = CARTESIAN_POINT ( 'NONE',  ( -98.89303308397303738, -25.25460725902716774, 6.110950176806278833 ) ) ;
#78100 = VERTEX_POINT ( 'NONE', #87836 ) ;
#78101 = CARTESIAN_POINT ( 'NONE',  ( 20.39576089869593289, -0.2533167397448486957, 11.49999999999998934 ) ) ;
#78102 = ORIENTED_EDGE ( 'NONE', *, *, #73811, .T. ) ;
#78103 = CARTESIAN_POINT ( 'NONE',  ( 3.160899137004691717, 22.77513019406404382, -1.500000000000002220 ) ) ;
#78104 = CARTESIAN_POINT ( 'NONE',  ( -7.312991930324885814, -5.876774720514414518, 20.02088365235844947 ) ) ;
#78105 = CARTESIAN_POINT ( 'NONE',  ( -54.49651346487743098, -24.35071581493543391, 9.817618358456034144 ) ) ;
#78106 = ORIENTED_EDGE ( 'NONE', *, *, #86831, .T. ) ;
#78107 = CARTESIAN_POINT ( 'NONE',  ( -110.9909297185884327, -25.15277794460069671, 6.986250878905948980 ) ) ;
#78108 = EDGE_CURVE ( 'NONE', #63195, #85963, #2014, .T. ) ;
#78109 = CARTESIAN_POINT ( 'NONE',  ( -53.53250099041933652, -24.66019654487199375, 8.947790411086122830 ) ) ;
#78111 = ORIENTED_EDGE ( 'NONE', *, *, #69834, .T. ) ;
#78110 = CARTESIAN_POINT ( 'NONE',  ( 12.49974722350246736, 17.29906535522423638, 11.49999999999999645 ) ) ;
#78112 = CIRCLE ( 'NONE', #27942, 2.000000000000001776 ) ;
#78113 = ORIENTED_EDGE ( 'NONE', *, *, #76312, .F. ) ;
#78114 = CARTESIAN_POINT ( 'NONE',  ( -21.66996937300057269, -4.939502015459471096, -1.500000000000002220 ) ) ;
#78115 = AXIS2_PLACEMENT_3D ( 'NONE', #88455, #88954, #58512 ) ;
#78116 = CARTESIAN_POINT ( 'NONE',  ( -7.851838630353038972, -19.11370409007043847, -1.500000000000002220 ) ) ;
#78117 = EDGE_LOOP ( 'NONE', ( #2190, #14592, #87114, #13617 ) ) ;
#78118 = EDGE_CURVE ( 'NONE', #18750, #7644, #58396, .T. ) ;
#78119 = CARTESIAN_POINT ( 'NONE',  ( -108.9545715455115129, -25.27682575596922021, 4.170144840047737667 ) ) ;
#78120 = CARTESIAN_POINT ( 'NONE',  ( -95.50376022624848815, -24.83644354573579349, 8.397322867130096569 ) ) ;
#78121 = VERTEX_POINT ( 'NONE', #66025 ) ;
#78122 = CARTESIAN_POINT ( 'NONE',  ( -83.62287095715007013, -23.47596703998600631, 11.44779298504227860 ) ) ;
#78123 = ORIENTED_EDGE ( 'NONE', *, *, #9698, .F. ) ;
#78124 = DIRECTION ( 'NONE',  ( -0.000000000000000000, 0.000000000000000000, -1.000000000000000000 ) ) ;
#78125 = CARTESIAN_POINT ( 'NONE',  ( -48.52287095715006160, -24.64898659630367561, 1.056161002820821038 ) ) ;
#78126 = CARTESIAN_POINT ( 'NONE',  ( 4.013313563623547964, -20.52093592976233438, -1.500000000000002220 ) ) ;
#78127 = CARTESIAN_POINT ( 'NONE',  ( -18.25314811174894913, -11.95880190493418738, 11.49999999999999645 ) ) ;
#78128 = CARTESIAN_POINT ( 'NONE',  ( -44.62287095715004881, -29.50250243563736774, 8.947779886222148704 ) ) ;
#78129 = CARTESIAN_POINT ( 'NONE',  ( -99.50401037219587863, -25.08800262214248988, 7.296243261531031088 ) ) ;
#78130 = CARTESIAN_POINT ( 'NONE',  ( 22.01961411883556252, 4.383451955130949429, 11.49999999999998934 ) ) ;
#78131 = FACE_OUTER_BOUND ( 'NONE', #57820, .T. ) ;
#78132 = CARTESIAN_POINT ( 'NONE',  ( -58.52287095715006160, -24.34917612406836440, 0.1852690917426536021 ) ) ;
#78133 = AXIS2_PLACEMENT_3D ( 'NONE', #16557, #847, #56152 ) ;
#78134 = CARTESIAN_POINT ( 'NONE',  ( -54.62287095715005592, -24.65952944569304606, 1.056160979905694131 ) ) ;
#78135 = PRODUCT_DEFINITION_FORMATION_WITH_SPECIFIED_SOURCE ( 'ANY', '', #20704, .NOT_KNOWN. ) ;
#78136 = ORIENTED_EDGE ( 'NONE', *, *, #15077, .F. ) ;
#78137 = EDGE_LOOP ( 'NONE', ( #60766, #37576, #9143, #73607 ) ) ;
#78138 = VERTEX_POINT ( 'NONE', #96942 ) ;
#78139 = EDGE_CURVE ( 'NONE', #76298, #60943, #73609, .T. ) ;
#78140 = B_SPLINE_CURVE_WITH_KNOTS ( 'NONE', 3,
 ( #9614, #53416, #39565, #16220, #47185, #78104, #70515, #1006, #78602, #9111, #40070, #71024, #32452, #24831, #55808, #40575, #71527, #19218, #49199 ),
 .UNSPECIFIED., .F., .F.,
 ( 4, 1, 1, 1, 1, 1, 1, 1, 1, 1, 1, 1, 1, 1, 1, 1, 4 ),
 ( 0.000000000000000000, 0.07834298519370234970, 0.1505633028794191031, 0.2161510566599780803, 0.2756797924514261533, 0.3287070503654628273, 0.3759044348322084228, 0.4173018977400322349, 0.4526927480535833936, 0.5172652917530119465, 0.5812165680623057051, 0.6453218939728029291, 0.7120244933797633680, 0.7801300447160454121, 0.8502182262116654288, 0.9226485217347378809, 1.000000000000000000 ),
 .UNSPECIFIED. ) ;
#78141 = CARTESIAN_POINT ( 'NONE',  ( 4.555389213293416617, -20.86945110937667280, -1.500000000000002220 ) ) ;
#78142 = CARTESIAN_POINT ( 'NONE',  ( -7.019573500991415749, 21.25910006591672996, 11.49999999999999645 ) ) ;
#78143 = VERTEX_POINT ( 'NONE', #41674 ) ;
#78144 = CARTESIAN_POINT ( 'NONE',  ( 12.48895993392301307, -16.95307763291877379, 11.49999999999998934 ) ) ;
#78145 = CARTESIAN_POINT ( 'NONE',  ( -30.59774034470085624, -24.76209092868932160, 1.363670884829966123 ) ) ;
#78146 = CARTESIAN_POINT ( 'NONE',  ( -18.10700488460823721, -8.296952762055457953, -1.500000000000002220 ) ) ;
#78147 = LINE ( 'NONE', #94890, #50157 ) ;
#78148 = CARTESIAN_POINT ( 'NONE',  ( 3.025806405283164136, -5.876774720514419847, 20.84867811309776542 ) ) ;
#78149 = CARTESIAN_POINT ( 'NONE',  ( -20.58003014649542095, 7.718188279156099618, -1.500000000000002220 ) ) ;
#78150 = LINE ( 'NONE', #55351, #36601 ) ;
#78151 = VECTOR ( 'NONE', #42737, 1000.000000000000114 ) ;
#78152 = VERTEX_POINT ( 'NONE', #50277 ) ;
#78153 = CARTESIAN_POINT ( 'NONE',  ( -104.6228709571500559, -29.50248528299804818, 1.056150453629042030 ) ) ;
#78154 = EDGE_CURVE ( 'NONE', #76877, #76243, #43168, .T. ) ;
#78155 = CARTESIAN_POINT ( 'NONE',  ( -121.5228709571500474, -24.50216790748205398, 0.6166512839542598323 ) ) ;
#78156 = CARTESIAN_POINT ( 'NONE',  ( 8.324980675869593227, 19.10421180063631752, 11.49999999999999645 ) ) ;
#78157 = EDGE_CURVE ( 'NONE', #97072, #16621, #18328, .T. ) ;
#78158 = EDGE_CURVE ( 'NONE', #45042, #71192, #4101, .T. ) ;
#78159 = CARTESIAN_POINT ( 'NONE',  ( 31.63608488009066733, -3.316774720514426456, 27.34773273846990804 ) ) ;
#78160 = DIRECTION ( 'NONE',  ( -0.000000000000000000, -0.000000000000000000, -1.000000000000000000 ) ) ;
#78161 = ADVANCED_FACE ( 'NONE', ( #10710 ), #34561, .F. ) ;
#78162 = CARTESIAN_POINT ( 'NONE',  ( -90.52287095715006160, -25.00158670708909625, 2.256160236439166411 ) ) ;
#78163 = CARTESIAN_POINT ( 'NONE',  ( -4.607724273132460802, 20.83226218841027944, 11.49999999999998934 ) ) ;
#78164 = CARTESIAN_POINT ( 'NONE',  ( -98.59636631811120822, -23.73791477778911840, 11.05961554403170410 ) ) ;
#78165 = DIRECTION ( 'NONE',  ( 0.000000000000000000, -2.173523156925979552E-06, 0.9999999999976378895 ) ) ;
#78166 = LINE ( 'NONE', #33515, #45444 ) ;
#78167 = CARTESIAN_POINT ( 'NONE',  ( -69.32992225813151776, -25.30188801935125653, 5.302352381037461093 ) ) ;
#78168 = B_SPLINE_CURVE_WITH_KNOTS ( 'NONE', 3,
 ( #86017, #72806, #16494, #63712, #47967, #65217 ),
 .UNSPECIFIED., .F., .F.,
 ( 4, 2, 4 ),
 ( 0.000000000000000000, 0.001380901958385387894, 0.002761803916770775788 ),
 .UNSPECIFIED. ) ;
#78169 = CARTESIAN_POINT ( 'NONE',  ( 17.87336509531889561, -13.68139028912531785, -1.500000000000002220 ) ) ;
#78170 = VECTOR ( 'NONE', #26530, 1000.000000000000114 ) ;
#78171 = B_SPLINE_SURFACE_WITH_KNOTS ( 'NONE', 3, 1, ( 
 ( #70726, #48395 ),
 ( #62125, #100141 ),
 ( #56016, #23025 ),
 ( #39268, #63129 ),
 ( #15926, #84943 ),
 ( #71232, #46893 ),
 ( #77320, #77811 ),
 ( #24541, #38767 ),
 ( #70228, #708 ),
 ( #79329, #61633 ),
 ( #93047, #31654 ) ),
 .UNSPECIFIED., .F., .F., .F.,
 ( 4, 1, 1, 1, 1, 1, 1, 1, 4 ),
 ( 2, 2 ),
 ( 0.000000000000000000, 0.1280675485958910620, 0.2506083188676687667, 0.3706301659145028737, 0.4900722467299511442, 0.6103747641546218849, 0.7343130699115234528, 0.8632165042449871928, 1.000000000000000000 ),
 ( 0.000000000000000000, 1.000000000000000000 ),
 .UNSPECIFIED. ) ;
#78172 = DIRECTION ( 'NONE',  ( -3.773278334444167608E-23, 1.000000000000000000, 0.000000000000000000 ) ) ;
#78173 = ORIENTED_EDGE ( 'NONE', *, *, #11204, .F. ) ;
#78174 = CARTESIAN_POINT ( 'NONE',  ( -78.94971039626406650, -25.28065224745481032, 5.786440773245404401 ) ) ;
#78175 = CARTESIAN_POINT ( 'NONE',  ( -81.62287095715005592, -24.64965695001468404, 8.947790433994182280 ) ) ;
#78176 = CARTESIAN_POINT ( 'NONE',  ( 16.89532177248590372, -10.13005384644002227, 11.49999999999999645 ) ) ;
#78177 = LINE ( 'NONE', #85810, #89246 ) ;
#78178 = CARTESIAN_POINT ( 'NONE',  ( -119.5228709571500758, -23.47596703998600631, 11.44779298504227860 ) ) ;
#78179 = B_SPLINE_CURVE_WITH_KNOTS ( 'NONE', 3,
 ( #56782, #87717, #18199, #95817, #45539, #60273 ),
 .UNSPECIFIED., .F., .F.,
 ( 4, 2, 4 ),
 ( 6.384118678608962257E-06, 0.001386860460828373467, 0.002767336802978137989 ),
 .UNSPECIFIED. ) ;
#78180 = ADVANCED_FACE ( 'NONE', ( #28416 ), #18810, .T. ) ;
#78181 = EDGE_CURVE ( 'NONE', #78336, #77156, #68495, .T. ) ;
#78182 = ORIENTED_EDGE ( 'NONE', *, *, #5567, .T. ) ;
#78183 = CARTESIAN_POINT ( 'NONE',  ( 0.4325450954222598288, 0.000000000000000000, 0.000000000000000000 ) ) ;
#78184 = CARTESIAN_POINT ( 'NONE',  ( -58.62287095715004881, -29.50247984919015209, -1.443849546365056913 ) ) ;
#78185 = CARTESIAN_POINT ( 'NONE',  ( -52.52287095715005449, -23.47593901973090524, -1.443836447538997092 ) ) ;
#78186 = CARTESIAN_POINT ( 'NONE',  ( -23.62875734969026453, -6.143225279485574397, 24.50402280011862288 ) ) ;
#78187 = CARTESIAN_POINT ( 'NONE',  ( 0.5484783294719396407, -19.75002165935583776, -1.500000000000002220 ) ) ;
#78188 = ORIENTED_EDGE ( 'NONE', *, *, #34671, .F. ) ;
#78189 = AXIS2_PLACEMENT_3D ( 'NONE', #11323, #27048, #25544 ) ;
#78190 = CARTESIAN_POINT ( 'NONE',  ( 4.784292611721462585, 6.376774720514426953, -25.54547254883130947 ) ) ;
#78191 = EDGE_CURVE ( 'NONE', #26463, #98147, #11701, .T. ) ;
#78192 = CALENDAR_DATE ( 2026, 9, 10 ) ;
#78193 = ORIENTED_EDGE ( 'NONE', *, *, #69966, .T. ) ;
#78194 = PLANE ( 'NONE',  #1403 ) ;
#78195 = CARTESIAN_POINT ( 'NONE',  ( -53.62287095715005592, -23.47593901973091235, -1.443836447539009749 ) ) ;
#78196 = CARTESIAN_POINT ( 'NONE',  ( -69.75874677887840392, -25.29662546892861386, 5.475966365782060308 ) ) ;
#78197 = CARTESIAN_POINT ( 'NONE',  ( 31.90158556755667973, -4.901725665521331265, -4.230180255418043878 ) ) ;
#78198 = FACE_OUTER_BOUND ( 'NONE', #85776, .T. ) ;
#78199 = CARTESIAN_POINT ( 'NONE',  ( -89.49044894935767047, -25.12049752546738191, 2.832404795212222659 ) ) ;
#78200 = CARTESIAN_POINT ( 'NONE',  ( 14.76093561896378326, 3.316774720514426456, -26.55548769130088260 ) ) ;
#78201 = CARTESIAN_POINT ( 'NONE',  ( 19.27460657395150889, -5.330843762518559181, -1.500000000000002220 ) ) ;
#78202 = ADVANCED_FACE ( 'NONE', ( #82210 ), #47526, .T. ) ;
#78203 = FACE_OUTER_BOUND ( 'NONE', #36312, .T. ) ;
#78204 = CARTESIAN_POINT ( 'NONE',  ( 22.02124265030973760, 5.356774720514425603, 12.85402280011862430 ) ) ;
#78205 = ORIENTED_EDGE ( 'NONE', *, *, #35893, .T. ) ;
#78206 = EDGE_CURVE ( 'NONE', #86377, #77091, #67021, .T. ) ;
#78207 = AXIS2_PLACEMENT_3D ( 'NONE', #32259, #72337, #40379 ) ;
#78208 = EDGE_CURVE ( 'NONE', #58683, #27962, #59382, .T. ) ;
#78210 = CARTESIAN_POINT ( 'NONE',  ( -79.64684267427536213, -23.48786465467241058, 11.44779295918254824 ) ) ;
#78209 = CC_DESIGN_APPROVAL ( #83531, ( #19046 ) ) ;
#78211 = CARTESIAN_POINT ( 'NONE',  ( -110.3009842343709721, -25.18430154008630595, 3.294836824253255081 ) ) ;
#78212 = CARTESIAN_POINT ( 'NONE',  ( -35.49723519497781865, -24.15503026093914940, -0.2815557561904327155 ) ) ;
#78213 = CARTESIAN_POINT ( 'NONE',  ( -29.49875734969026198, -5.965225279485572685, 10.11402280011862587 ) ) ;
#78214 = CARTESIAN_POINT ( 'NONE',  ( -118.3656671591979261, -25.31826104724058979, 3.540018580561490324 ) ) ;
#78215 = DIRECTION ( 'NONE',  ( -0.7689940216596065081, 0.000000000000000000, 0.6392559695863502256 ) ) ;
#78216 = DIRECTION ( 'NONE',  ( 3.773278334444166432E-23, -1.000000000000000000, 0.000000000000000000 ) ) ;
#78217 = AXIS2_PLACEMENT_3D ( 'NONE', #15058, #40409, #8454 ) ;
#78218 = CARTESIAN_POINT ( 'NONE',  ( -90.62287095715004170, -29.50250786944525672, 11.44777988621623344 ) ) ;
#78219 = ORIENTED_EDGE ( 'NONE', *, *, #92533, .F. ) ;
#78220 = CARTESIAN_POINT ( 'NONE',  ( 20.23688964843749005, 1.552196809742036221, 11.49999999999998934 ) ) ;
#78221 = VECTOR ( 'NONE', #100333, 1000.000000000000000 ) ;
#78222 = CARTESIAN_POINT ( 'NONE',  ( -65.05438548721848235, 6.376774720514426953, 30.51402280011862089 ) ) ;
#78223 = CARTESIAN_POINT ( 'NONE',  ( -88.52287095715006160, -23.48786465467241769, 11.44779295918254292 ) ) ;
#78224 = ORIENTED_EDGE ( 'NONE', *, *, #71798, .F. ) ;
#78225 = DIRECTION ( 'NONE',  ( 3.773278334444167608E-23, -1.000000000000000000, 0.000000000000000000 ) ) ;
#78226 = CARTESIAN_POINT ( 'NONE',  ( 5.670567493371958534, -19.34269084982597775, -1.500000000000002220 ) ) ;
#78227 = CARTESIAN_POINT ( 'NONE',  ( -9.089321149825819290, -19.05894737874082168, 11.49999999999999645 ) ) ;
#78228 = CARTESIAN_POINT ( 'NONE',  ( 22.02032638543937182, 1.892999326154024553, 11.49999999999998934 ) ) ;
#78229 = CARTESIAN_POINT ( 'NONE',  ( 9.245221688665949955, -18.36014492602614467, -1.500000000000002220 ) ) ;
#78230 = CARTESIAN_POINT ( 'NONE',  ( 15.77315497053715987, 4.795106742339076078, -28.11009842133919534 ) ) ;
#78231 = ORIENTED_EDGE ( 'NONE', *, *, #58731, .T. ) ;
#78232 = DIRECTION ( 'NONE',  ( 0.000000000000000000, -0.9999999999976377785, -2.173523156925979128E-06 ) ) ;
#78233 = EDGE_LOOP ( 'NONE', ( #34573, #28503, #63459, #97158 ) ) ;
#78234 = CARTESIAN_POINT ( 'NONE',  ( 22.81105451610979173, -1.684774720501991396, -18.46691820600746681 ) ) ;
#78235 = CARTESIAN_POINT ( 'NONE',  ( -110.6228709571501128, -24.83620972994592080, 8.398175272781363887 ) ) ;
#78236 = ORIENTED_EDGE ( 'NONE', *, *, #49163, .T. ) ;
#78237 = ORIENTED_EDGE ( 'NONE', *, *, #88865, .F. ) ;
#78238 = B_SPLINE_CURVE_WITH_KNOTS ( 'NONE', 3,
 ( #47737, #77659, #93897, #549 ),
 .UNSPECIFIED., .F., .F.,
 ( 4, 4 ),
 ( 0.2389318754978128900, 0.2399326225385782496 ),
 .UNSPECIFIED. ) ;
#78239 = ORIENTED_EDGE ( 'NONE', *, *, #82637, .F. ) ;
#78240 = DIRECTION ( 'NONE',  ( 0.000000000000000000, 0.000000000000000000, 1.000000000000000000 ) ) ;
#78241 = CARTESIAN_POINT ( 'NONE',  ( -55.62287095715004170, -24.99156045073392463, 7.747789690856161648 ) ) ;
#78242 = DIRECTION ( 'NONE',  ( -0.000000000000000000, 0.000000000000000000, 1.000000000000000000 ) ) ;
#78243 = CARTESIAN_POINT ( 'NONE',  ( -14.43086120294938368, -14.79396848081076854, -1.500000000000002220 ) ) ;
#78244 = CARTESIAN_POINT ( 'NONE',  ( 16.98214085172422827, 13.50221961261776293, 11.49999999999999645 ) ) ;
#78245 = ORIENTED_EDGE ( 'NONE', *, *, #36830, .F. ) ;
#78246 = AXIS2_PLACEMENT_3D ( 'NONE', #18872, #4158, #26498 ) ;
#78247 = CARTESIAN_POINT ( 'NONE',  ( -41.62287095715006302, -23.47596703998600276, 11.44779298504227505 ) ) ;
#78248 = CARTESIAN_POINT ( 'NONE',  ( 3.714584954927674154, -5.876774720514402972, 18.16171433633635246 ) ) ;
#78249 = CARTESIAN_POINT ( 'NONE',  ( 3.752539591237177508, -22.04708138622333635, 11.49999999999998934 ) ) ;
#78250 = CARTESIAN_POINT ( 'NONE',  ( -47.58188357232938159, -24.51419770103156637, 9.386484678747176957 ) ) ;
#78251 = CARTESIAN_POINT ( 'NONE',  ( -101.5228709571500758, -24.64965694238407323, 8.947790433994194714 ) ) ;
#78252 = EDGE_LOOP ( 'NONE', ( #92259, #59594, #2476, #32368 ) ) ;
#78253 = CARTESIAN_POINT ( 'NONE',  ( -117.2170119873909329, -25.33573473601760995, 6.311387531435581622 ) ) ;
#78254 = CARTESIAN_POINT ( 'NONE',  ( -35.48359714022421940, -24.52399227489126687, 9.353111116836519301 ) ) ;
#78255 = CIRCLE ( 'NONE', #55622, 130.7884398600581335 ) ;
#78256 = ORIENTED_EDGE ( 'NONE', *, *, #19976, .T. ) ;
#78257 = CARTESIAN_POINT ( 'NONE',  ( -110.5228709571500616, -23.47596703998600631, 11.44779298504228038 ) ) ;
#78258 = VERTEX_POINT ( 'NONE', #3606 ) ;
#78259 = FACE_OUTER_BOUND ( 'NONE', #77526, .T. ) ;
#78260 = CARTESIAN_POINT ( 'NONE',  ( -20.81765089029956783, 3.879123387127271005, -1.500000000000002220 ) ) ;
#78261 = ORIENTED_EDGE ( 'NONE', *, *, #93067, .F. ) ;
#78262 = DIRECTION ( 'NONE',  ( -0.000000000000000000, 1.000000000000000000, -0.000000000000000000 ) ) ;
#78263 = ADVANCED_FACE ( 'NONE', ( #65524 ), #57901, .F. ) ;
#78264 = CARTESIAN_POINT ( 'NONE',  ( -20.57666286913221754, 7.287794730890116313, 11.49999999999998934 ) ) ;
#78265 = PLANE ( 'NONE',  #75625 ) ;
#78266 = ADVANCED_FACE ( 'NONE', ( #21298 ), #85592, .T. ) ;
#78267 = FACE_OUTER_BOUND ( 'NONE', #88344, .T. ) ;
#78268 = CARTESIAN_POINT ( 'NONE',  ( 6.259688558337090036, -5.876774720514413630, 19.73360741988579292 ) ) ;
#78269 = CARTESIAN_POINT ( 'NONE',  ( -18.25314811174894913, -11.95880190493418738, -1.500000000000002220 ) ) ;
#78270 = CARTESIAN_POINT ( 'NONE',  ( -30.57287095715005520, -23.78465599299007849, 10.96065251130191776 ) ) ;
#78271 = EDGE_LOOP ( 'NONE', ( #63458, #52958 ) ) ;
#78272 = CARTESIAN_POINT ( 'NONE',  ( 7.089543269230769162, -5.876774720514413630, 19.75741185897435415 ) ) ;
#78273 = CARTESIAN_POINT ( 'NONE',  ( -85.64374319538433156, -23.85049219812685450, 10.88485053497527133 ) ) ;
#78274 = VERTEX_POINT ( 'NONE', #75089 ) ;
#78275 = ADVANCED_FACE ( 'NONE', ( #44156 ), #2560, .F. ) ;
#78276 = EDGE_CURVE ( 'NONE', #88974, #40829, #86703, .T. ) ;
#78277 = ORIENTED_EDGE ( 'NONE', *, *, #61054, .T. ) ;
#78278 = EDGE_CURVE ( 'NONE', #26092, #27769, #16691, .T. ) ;
#78279 = AXIS2_PLACEMENT_3D ( 'NONE', #26441, #4605, #35553 ) ;
#78280 = B_SPLINE_CURVE_WITH_KNOTS ( 'NONE', 3,
 ( #97080, #20941, #44305, #20440 ),
 .UNSPECIFIED., .F., .F.,
 ( 4, 4 ),
 ( 0.000000000000000000, 9.999999999997510880E-05 ),
 .UNSPECIFIED. ) ;
#78281 = ORIENTED_EDGE ( 'NONE', *, *, #77008, .F. ) ;
#78282 = SECURITY_CLASSIFICATION ( '', '', #82582 ) ;
#78283 = CARTESIAN_POINT ( 'NONE',  ( -2.701720430790311767, 5.965225279485594001, -28.90526747363640681 ) ) ;
#78284 = CARTESIAN_POINT ( 'NONE',  ( -82.55076503047374104, -24.15543982623907482, -0.2315651400026498552 ) ) ;
#78285 = CARTESIAN_POINT ( 'NONE',  ( -17.82860346875387947, 11.52481846644873187, -1.500000000000002220 ) ) ;
#78286 = B_SPLINE_CURVE_WITH_KNOTS ( 'NONE', 3,
 ( #83442, #100140, #13432, #36784 ),
 .UNSPECIFIED., .F., .F.,
 ( 4, 4 ),
 ( 0.000000000000000000, 0.0001002978982766898939 ),
 .UNSPECIFIED. ) ;
#78287 = CARTESIAN_POINT ( 'NONE',  ( -94.58429178781234725, -24.65952944569304606, 1.056160979905703234 ) ) ;
#78288 = CARTESIAN_POINT ( 'NONE',  ( -30.62155233649868791, -24.14929313691197521, 10.49653219292474482 ) ) ;
#78289 = CARTESIAN_POINT ( 'NONE',  ( -7.160000000000000142, 0.1579206558577706254, 7.788828319098143105 ) ) ;
#78290 = DIRECTION ( 'NONE',  ( -1.000000000000000000, -3.773278334444166432E-23, -8.201307841325785021E-29 ) ) ;
#78292 = CARTESIAN_POINT ( 'NONE',  ( 4.312616920666290987, -18.91975033782923887, 11.49999999999998934 ) ) ;
#78291 = AXIS2_PLACEMENT_3D ( 'NONE', #84542, #7416, #59731 ) ;
#78293 = CARTESIAN_POINT ( 'NONE',  ( -40.93200155000062068, -25.32724636324323342, 4.398074533285874388 ) ) ;
#78294 = ORIENTED_EDGE ( 'NONE', *, *, #91912, .T. ) ;
#78295 = CARTESIAN_POINT ( 'NONE',  ( 1.793504005174451077, 19.40006364325761012, 11.49999999999999645 ) ) ;
#78296 = DIRECTION ( 'NONE',  ( -0.9978940991575084851, 0.000000000000000000, -0.06486421869277853025 ) ) ;
#78297 = AXIS2_PLACEMENT_3D ( 'NONE', #21503, #19642, #27765 ) ;
#78298 = CARTESIAN_POINT ( 'NONE',  ( -79.62463646828913966, -25.18409543558836816, 6.717720826779347121 ) ) ;
#78299 = EDGE_CURVE ( 'NONE', #13389, #41697, #15694, .T. ) ;
#78300 = ORIENTED_EDGE ( 'NONE', *, *, #84533, .T. ) ;
#78301 = CARTESIAN_POINT ( 'NONE',  ( 4.585161930874343206, -5.876774720514426953, 21.47592444013076118 ) ) ;
#78302 = CARTESIAN_POINT ( 'NONE',  ( -59.52287095715006870, -23.96177878511308990, 10.65340807706329862 ) ) ;
#78303 = CARTESIAN_POINT ( 'NONE',  ( -30.53953689203329702, -23.47593904782709018, -1.430909884246568842 ) ) ;
#78304 = CARTESIAN_POINT ( 'NONE',  ( -93.63080997736221889, -24.15620529776628445, 10.23563542870659404 ) ) ;
#78306 = ADVANCED_FACE ( 'NONE', ( #87207 ), #48160, .T. ) ;
#78305 = CARTESIAN_POINT ( 'NONE',  ( 0.7808950796103379943, -19.64173473864696717, -1.500000000000002220 ) ) ;
#78307 = B_SPLINE_SURFACE_WITH_KNOTS ( 'NONE', 3, 3, ( 
 ( #39620, #72588, #34019, #8680 ),
 ( #62984, #47747, #36006, #58854 ),
 ( #89304, #88811, #26405, #65994 ),
 ( #11666, #96912, #4575, #73581 ),
 ( #73089, #18779, #97409, #27406 ),
 ( #19277, #27898, #20766, #58365 ),
 ( #95912, #59349, #35020, #75055 ) ),
 .UNSPECIFIED., .F., .F., .F.,
 ( 4, 3, 4 ),
 ( 4, 4 ),
 ( 0.7945040050992236980, 0.8970133687736498995, 0.9995227324480762121 ),
 ( 0.6596616264046517575, 0.6609788945409680316 ),
 .UNSPECIFIED. ) ;
#78308 = CARTESIAN_POINT ( 'NONE',  ( -41.34727404100192416, -25.31583668745965809, 4.610738936032308111 ) ) ;
#78309 = ORIENTED_EDGE ( 'NONE', *, *, #34640, .T. ) ;
#78310 = CARTESIAN_POINT ( 'NONE',  ( 18.62697458635512859, 10.92912097662538251, 11.49999999999998934 ) ) ;
#78311 = DIRECTION ( 'NONE',  ( -1.000000000000000000, -0.000000000000000000, -0.000000000000000000 ) ) ;
#78312 = LINE ( 'NONE', #16411, #68241 ) ;
#78313 = CARTESIAN_POINT ( 'NONE',  ( -5.338719972479099241, 22.46511350730333589, -1.500000000000002220 ) ) ;
#78314 = PERSON_AND_ORGANIZATION_ROLE ( 'design_supplier' ) ;
#78315 = FACE_OUTER_BOUND ( 'NONE', #2510, .T. ) ;
#78316 = CARTESIAN_POINT ( 'NONE',  ( 4.215004826710222474, -6.376774720514427841, 21.34072927444733381 ) ) ;
#78317 = FACE_OUTER_BOUND ( 'NONE', #12711, .T. ) ;
#78318 = CARTESIAN_POINT ( 'NONE',  ( -64.62287095715005592, -24.35013146730203459, 9.818937971375113705 ) ) ;
#78319 = CARTESIAN_POINT ( 'NONE',  ( -111.7494854843401555, -25.29824069328104486, 4.020187583360979922 ) ) ;
#78320 = CARTESIAN_POINT ( 'NONE',  ( -121.6228709571500843, -23.96177878511308990, 10.65340807706329862 ) ) ;
#78321 = CARTESIAN_POINT ( 'NONE',  ( -114.5892327960407187, -24.35071581493544102, 9.817618358456016381 ) ) ;
#78322 = CARTESIAN_POINT ( 'NONE',  ( -7.573260116017839216, 18.43532004384545786, 11.49999999999998934 ) ) ;
#78323 = AXIS2_PLACEMENT_3D ( 'NONE', #67439, #61332, #60834 ) ;
#78324 = PLANE ( 'NONE',  #87290 ) ;
#78325 = CARTESIAN_POINT ( 'NONE',  ( 1.944447714513537262, -19.71154682592685958, -1.500000000000002220 ) ) ;
#78326 = CARTESIAN_POINT ( 'NONE',  ( -56.65018345228885011, -23.73766607897670511, -1.055555164236459342 ) ) ;
#78327 = EDGE_CURVE ( 'NONE', #6143, #50179, #63905, .T. ) ;
#78328 = VECTOR ( 'NONE', #43506, 1000.000000000000114 ) ;
#78329 = CARTESIAN_POINT ( 'NONE',  ( -93.52287095715006160, -23.47593901973090524, -1.443836447538996648 ) ) ;
#78330 = CARTESIAN_POINT ( 'NONE',  ( -99.64934318012689118, -25.30535455722350591, 4.927356316503054501 ) ) ;
#78331 = CARTESIAN_POINT ( 'NONE',  ( -8.119355292522030254, -19.11072509857415369, 11.49999999999999645 ) ) ;
#78332 = CARTESIAN_POINT ( 'NONE',  ( -101.9228709571500815, -23.47596703998600631, 11.44779298504227683 ) ) ;
#78333 = EDGE_CURVE ( 'NONE', #66467, #92752, #89173, .T. ) ;
#78334 = DIRECTION ( 'NONE',  ( 0.000000000000000000, -2.173523156925979552E-06, 0.9999999999976378895 ) ) ;
#78335 = CARTESIAN_POINT ( 'NONE',  ( -17.61067154241388977, 14.45706175128816184, 11.49999999999999645 ) ) ;
#78336 = VERTEX_POINT ( 'NONE', #41044 ) ;
#78337 = CARTESIAN_POINT ( 'NONE',  ( -83.62287095715011276, -23.96177878511308634, 10.65340807706329684 ) ) ;
#78338 = CARTESIAN_POINT ( 'NONE',  ( -106.6228709571500275, -23.72747288104469732, -1.053458166803225016 ) ) ;
#78339 = ORIENTED_EDGE ( 'NONE', *, *, #18627, .T. ) ;
#78340 = CARTESIAN_POINT ( 'NONE',  ( 17.48260522047220888, -10.12088315688240314, -1.500000000000002220 ) ) ;
#78341 = B_SPLINE_CURVE_WITH_KNOTS ( 'NONE', 3,
 ( #44424, #13948, #68251, #64156, #2243, #8840 ),
 .UNSPECIFIED., .F., .F.,
 ( 4, 2, 4 ),
 ( 0.000000000000000000, 0.001380764517854766267, 0.002761529035709532533 ),
 .UNSPECIFIED. ) ;
#78342 = FACE_OUTER_BOUND ( 'NONE', #92100, .T. ) ;
#78343 = AXIS2_PLACEMENT_3D ( 'NONE', #98709, #49317, #61670 ) ;
#78344 = CARTESIAN_POINT ( 'NONE',  ( -41.31743941260997133, -25.30152573394828863, 4.668812341817115907 ) ) ;
#78345 = ORIENTED_EDGE ( 'NONE', *, *, #56986, .T. ) ;
#78346 = CARTESIAN_POINT ( 'NONE',  ( -70.62287095715008434, -23.84081130438201157, 10.88220057463249013 ) ) ;
#78347 = CARTESIAN_POINT ( 'NONE',  ( -19.87571804785047647, -11.42512898079034400, 11.49999999999998934 ) ) ;
#78348 = CARTESIAN_POINT ( 'NONE',  ( -41.86664830098052192, -25.28370616383384828, 4.117318242077936397 ) ) ;
#78349 = CARTESIAN_POINT ( 'NONE',  ( -21.62496174240652991, 0.2022338437372764308, -1.500000000000002220 ) ) ;
#78350 = CARTESIAN_POINT ( 'NONE',  ( -41.05437968932909598, -25.04895513844916266, 7.488404314379859983 ) ) ;
#78351 = CARTESIAN_POINT ( 'NONE',  ( 0.7041596644206948863, -20.94928778062849162, 11.49999999999999645 ) ) ;
#78352 = ORIENTED_EDGE ( 'NONE', *, *, #42404, .F. ) ;
#78353 = DIRECTION ( 'NONE',  ( 0.000000000000000000, 0.000000000000000000, 1.000000000000000000 ) ) ;
#78354 = CARTESIAN_POINT ( 'NONE',  ( -124.5899959654626770, -24.15543982623907127, -0.2315651400026562945 ) ) ;
#78355 = CARTESIAN_POINT ( 'NONE',  ( -11.61111146657235871, -18.70866699758865792, 11.49999999999998934 ) ) ;
#78356 = CARTESIAN_POINT ( 'NONE',  ( 33.69795529655567634, 0.6647747205144264315, 23.11160796525322070 ) ) ;
#78357 = AXIS2_PLACEMENT_3D ( 'NONE', #96422, #82185, #43634 ) ;
#78358 = ORIENTED_EDGE ( 'NONE', *, *, #30522, .T. ) ;
#78359 = LINE ( 'NONE', #56559, #63899 ) ;
#78360 = CARTESIAN_POINT ( 'NONE',  ( -126.5228709571500616, -29.50248528299804818, 1.056150453629047137 ) ) ;
#78361 = ORIENTED_EDGE ( 'NONE', *, *, #10198, .F. ) ;
#78362 = LINE ( 'NONE', #33709, #84231 ) ;
#78363 = ORIENTED_EDGE ( 'NONE', *, *, #59043, .F. ) ;
#78364 = VECTOR ( 'NONE', #52000, 1000.000000000000000 ) ;
#78365 = EDGE_LOOP ( 'NONE', ( #10775, #98110, #17518, #9231 ) ) ;
#78366 = LINE ( 'NONE', #18480, #58323 ) ;
#78367 = DIRECTION ( 'NONE',  ( 0.000000000000000000, -1.000000000000000000, 0.000000000000000000 ) ) ;
#78368 = CARTESIAN_POINT ( 'NONE',  ( -36.59394419572883095, -24.15543982623907127, -0.2315651400026672579 ) ) ;
#78369 = B_SPLINE_CURVE_WITH_KNOTS ( 'NONE', 3,
 ( #36901, #12564, #83056, #74464, #60256, #4957 ),
 .UNSPECIFIED., .F., .F.,
 ( 4, 2, 4 ),
 ( 6.384118678618877625E-06, 0.001386860460828382140, 0.002767336802978145362 ),
 .UNSPECIFIED. ) ;
#78370 = CARTESIAN_POINT ( 'NONE',  ( 5.028806042385554953, -19.83023610923392610, -1.500000000000002220 ) ) ;
#78371 = ORIENTED_EDGE ( 'NONE', *, *, #44426, .F. ) ;
#78372 = CARTESIAN_POINT ( 'NONE',  ( -99.52232038167861106, -25.29196717039579312, 5.580301540147455164 ) ) ;
#78373 = CARTESIAN_POINT ( 'NONE',  ( -44.58162010085130333, -24.51314013834316086, 0.6176544820404110681 ) ) ;
#78374 = CARTESIAN_POINT ( 'NONE',  ( -43.62287095715004881, -29.50250786944525672, 11.44777988621624232 ) ) ;
#78375 = CARTESIAN_POINT ( 'NONE',  ( 22.30035941410032763, -0.3387204123245128873, -1.500000000000002220 ) ) ;
#78376 = CARTESIAN_POINT ( 'NONE',  ( -0.1490749075164066184, -21.12010817310450861, 11.44779298504228038 ) ) ;
#78377 = CARTESIAN_POINT ( 'NONE',  ( 1.751198251822017937, 22.56127314141087581, 0.000000000000000000 ) ) ;
#78378 = VERTEX_POINT ( 'NONE', #2483 ) ;
#78379 = FACE_OUTER_BOUND ( 'NONE', #17257, .T. ) ;
#78380 = CARTESIAN_POINT ( 'NONE',  ( -118.5228709571500900, -24.50216790748206108, 0.6166512839542579449 ) ) ;
#78381 = CARTESIAN_POINT ( 'NONE',  ( -18.77111393065419875, 9.022841878967760465, 11.49999999999998934 ) ) ;
#78382 = ORIENTED_EDGE ( 'NONE', *, *, #94550, .T. ) ;
#78384 = ORIENTED_EDGE ( 'NONE', *, *, #37532, .T. ) ;
#78383 = CARTESIAN_POINT ( 'NONE',  ( -122.6228709571500417, -29.50247984919015209, -1.443849546365046699 ) ) ;
#78385 = B_SPLINE_CURVE_WITH_KNOTS ( 'NONE', 3,
 ( #76376, #59184, #53073, #22578 ),
 .UNSPECIFIED., .F., .F.,
 ( 4, 4 ),
 ( 0.3000001472394721591, 0.3090065785115879704 ),
 .UNSPECIFIED. ) ;
#78386 = EDGE_LOOP ( 'NONE', ( #96232, #26248, #82367, #59885 ) ) ;
#78387 = EDGE_CURVE ( 'NONE', #67625, #30682, #4347, .T. ) ;
#78388 = CARTESIAN_POINT ( 'NONE',  ( -50.45832920465950622, -25.25854569161092300, 7.100425421451603825 ) ) ;
#78389 = CARTESIAN_POINT ( 'NONE',  ( -20.81348254183067681, -2.960215062046979373, -1.500000000000002220 ) ) ;
#78390 = ORIENTED_EDGE ( 'NONE', *, *, #93611, .T. ) ;
#78391 = LINE ( 'NONE', #48471, #99670 ) ;
#78393 = EDGE_CURVE ( 'NONE', #21579, #38489, #84805, .T. ) ;
#78392 = CARTESIAN_POINT ( 'NONE',  ( 0.000000000000000000, -1.473225279485573802, 0.000000000000000000 ) ) ;
#78394 = CARTESIAN_POINT ( 'NONE',  ( 11.25623914429021788, -3.316774720514424235, -27.04805245727492391 ) ) ;
#78395 = CARTESIAN_POINT ( 'NONE',  ( -101.1119640259560271, -25.25419526093012479, 7.433727736561444921 ) ) ;
#78396 = CARTESIAN_POINT ( 'NONE',  ( -60.62287095715004881, -23.84081130438200802, 10.88220057463249013 ) ) ;
#78397 = CARTESIAN_POINT ( 'NONE',  ( -117.9228709571500673, -23.47596703998600276, 11.44779298504227683 ) ) ;
#78399 = ORIENTED_EDGE ( 'NONE', *, *, #2703, .T. ) ;
#78398 = CARTESIAN_POINT ( 'NONE',  ( -21.14524153552446606, 6.695245452574716261, 11.49999999999999645 ) ) ;
#78400 = CARTESIAN_POINT ( 'NONE',  ( -88.88918693012689687, -25.26877915520014639, 5.947789088310639904 ) ) ;
#78401 = CARTESIAN_POINT ( 'NONE',  ( -105.5228709571500758, -23.47596703998600631, 11.44779298504228038 ) ) ;
#78402 = VERTEX_POINT ( 'NONE', #40036 ) ;
#78403 = VECTOR ( 'NONE', #89231, 1000.000000000000114 ) ;
#78404 = EDGE_CURVE ( 'NONE', #54320, #74213, #88222, .T. ) ;
#78405 = CARTESIAN_POINT ( 'NONE',  ( -18.74212433040710479, 12.77821124017617649, -1.500000000000002220 ) ) ;
#78406 = ADVANCED_FACE ( 'NONE', ( #80096 ), #11086, .F. ) ;
#78408 = VERTEX_POINT ( 'NONE', #26812 ) ;
#78407 = CARTESIAN_POINT ( 'NONE',  ( -6.487934372591614540, -6.376774720514411854, 19.49432735726520605 ) ) ;
#78409 = B_SPLINE_CURVE_WITH_KNOTS ( 'NONE', 3,
 ( #54148, #31795, #53646, #55142, #86575, #100271, #15556, #46518 ),
 .UNSPECIFIED., .F., .F.,
 ( 4, 2, 2, 4 ),
 ( 6.391158118964588215E-06, 0.002007136338672922248, 0.003007508928949903428, 0.004007881519226885042 ),
 .UNSPECIFIED. ) ;
#78410 = VECTOR ( 'NONE', #16461, 1000.000000000000114 ) ;
#78411 = EDGE_CURVE ( 'NONE', #20807, #35661, #73484, .T. ) ;
#78412 = VERTEX_POINT ( 'NONE', #96818 ) ;
#78413 = ADVANCED_FACE ( 'NONE', ( #35432 ), #19681, .F. ) ;
#78414 = LINE ( 'NONE', #69814, #88805 ) ;
#78415 = CARTESIAN_POINT ( 'NONE',  ( 2.654622155064554789, -19.98241913370796041, -1.500000000000002220 ) ) ;
#78416 = DIRECTION ( 'NONE',  ( 0.7071067811865437980, 0.7071067811865513475, -0.000000000000000000 ) ) ;
#78417 = VERTEX_POINT ( 'NONE', #82096 ) ;
#78418 = LINE ( 'NONE', #23122, #97359 ) ;
#78419 = CARTESIAN_POINT ( 'NONE',  ( -19.80502325505778671, 10.42642913751328670, -1.500000000000002220 ) ) ;
#78420 = ORIENTED_EDGE ( 'NONE', *, *, #4536, .T. ) ;
#78421 = ORIENTED_EDGE ( 'NONE', *, *, #76958, .F. ) ;
#78422 = CARTESIAN_POINT ( 'NONE',  ( -34.52287095715006160, -23.72773821059536203, 11.05748984161097326 ) ) ;
#78423 = CARTESIAN_POINT ( 'NONE',  ( -94.62356963122135767, -24.66019654487199730, 8.947790411086121054 ) ) ;
#78424 = DIRECTION ( 'NONE',  ( -0.7682573101345366862, 0.000000000000000000, 0.6401411605457395515 ) ) ;
#78425 = CARTESIAN_POINT ( 'NONE',  ( 0.000000000000000000, -1.473225279485573802, 0.000000000000000000 ) ) ;
#78426 = CARTESIAN_POINT ( 'NONE',  ( -63.93325875615660436, -24.26743686635980879, 0.04347934593174120760 ) ) ;
#78427 = CARTESIAN_POINT ( 'NONE',  ( -2.459534284235005863, 19.42625828800391119, 11.49999999999998934 ) ) ;
#78428 = CARTESIAN_POINT ( 'NONE',  ( -5.755030174389611730, -5.876774720514410966, 19.56655654527324728 ) ) ;
#78429 = ORIENTED_EDGE ( 'NONE', *, *, #93007, .T. ) ;
#78430 = CARTESIAN_POINT ( 'NONE',  ( 12.90647603486358364, 17.18646895862681134, 11.49999999999998934 ) ) ;
#78431 = CARTESIAN_POINT ( 'NONE',  ( -36.58953762381672448, -23.47593901973091235, -1.443836447539011525 ) ) ;
#78432 = CYLINDRICAL_SURFACE ( 'NONE', #61010, 3.549999999999999378 ) ;
#78433 = DIRECTION ( 'NONE',  ( -3.773278334444166432E-23, 1.000000000000000000, 0.000000000000000000 ) ) ;
#78434 = DIRECTION ( 'NONE',  ( -0.000000000000000000, -1.000000000000000000, -0.000000000000000000 ) ) ;
#78435 = CARTESIAN_POINT ( 'NONE',  ( 9.743704349311032686, 20.77413290702584092, -1.500000000000002220 ) ) ;
#78436 = COORDINATED_UNIVERSAL_TIME_OFFSET ( 0, 0, .AHEAD. ) ;
#78437 = CARTESIAN_POINT ( 'NONE',  ( -120.5562042904834072, -25.00158670708909625, 2.256160236439166411 ) ) ;
#78438 = CARTESIAN_POINT ( 'NONE',  ( -70.41995703322675126, -25.31157400179870720, 5.314953636079311927 ) ) ;
#78439 = CARTESIAN_POINT ( 'NONE',  ( 15.84714387567644955, -12.28532832577633194, 11.49999999999999645 ) ) ;
#78440 = CARTESIAN_POINT ( 'NONE',  ( -79.24831702480813078, -25.26612486446449779, 5.024332913579260484 ) ) ;
#78441 = CARTESIAN_POINT ( 'NONE',  ( -57.62287095715004881, -24.66019654487199020, 8.947790411086131712 ) ) ;
#78442 = FACE_OUTER_BOUND ( 'NONE', #79245, .T. ) ;
#78443 = LINE ( 'NONE', #8944, #21329 ) ;
#78444 = EDGE_LOOP ( 'NONE', ( #5645, #79275, #71637, #96350 ) ) ;
#78445 = LINE ( 'NONE', #32784, #88303 ) ;
#78446 = CARTESIAN_POINT ( 'NONE',  ( -9.430186865587145917, -19.61854929170128869, 11.49999999999998934 ) ) ;
#78447 = CARTESIAN_POINT ( 'NONE',  ( 15.97264540888995299, 3.405665504423739609, -27.93485543958162864 ) ) ;
#78448 = CARTESIAN_POINT ( 'NONE',  ( -15.16924259816527609, 12.53091941037558854, -1.500000000000002220 ) ) ;
#78449 = CARTESIAN_POINT ( 'NONE',  ( 14.61581670307174008, -6.475225279485573360, -27.35847990810646024 ) ) ;
#78450 = CARTESIAN_POINT ( 'NONE',  ( -109.3951644950792996, -25.27925728710133413, 4.495754977740414660 ) ) ;
#78451 = CALENDAR_DATE ( 2026, 9, 10 ) ;
#78452 = CARTESIAN_POINT ( 'NONE',  ( -91.55469187719226909, -23.96169478059713498, 10.65365249895718058 ) ) ;
#78453 = LINE ( 'NONE', #8956, #16708 ) ;
#78454 = CARTESIAN_POINT ( 'NONE',  ( 20.20254288951482735, -3.758238384022974277, 11.49999999999999645 ) ) ;
#78455 = CARTESIAN_POINT ( 'NONE',  ( 4.281508569253434260, -5.876774720514421624, 21.28700241941785265 ) ) ;
#78456 = EDGE_CURVE ( 'NONE', #43726, #22752, #6842, .T. ) ;
#78457 = AXIS2_PLACEMENT_3D ( 'NONE', #49904, #80838, #36652 ) ;
#78458 = CARTESIAN_POINT ( 'NONE',  ( -120.5222358249351799, -23.48783264082477018, -1.443836473390085695 ) ) ;
#78459 = CARTESIAN_POINT ( 'NONE',  ( -17.13258802378025791, -14.77425600068537115, 11.49999999999999645 ) ) ;
#78460 = ORIENTED_EDGE ( 'NONE', *, *, #76885, .F. ) ;
#78461 = EDGE_CURVE ( 'NONE', #7384, #92914, #10443, .T. ) ;
#78462 = CARTESIAN_POINT ( 'NONE',  ( -83.58953762381672448, -23.47596703998600276, 11.44779298504227683 ) ) ;
#78463 = CARTESIAN_POINT ( 'NONE',  ( 15.32643653063177958, 2.682774720514426559, -27.14485409495429380 ) ) ;
#78464 = CARTESIAN_POINT ( 'NONE',  ( -74.52287095715007581, -24.64965694238408034, 8.947790433994200043 ) ) ;
#78465 = CARTESIAN_POINT ( 'NONE',  ( 14.76069831378246455, -3.399792337529337516, -27.38466329193519755 ) ) ;
#78466 = CARTESIAN_POINT ( 'NONE',  ( -49.52287095715006160, -29.50248528299804818, 1.056150453629033370 ) ) ;
#78467 = AXIS2_PLACEMENT_3D ( 'NONE', #45953, #6876, #100194 ) ;
#78468 = DIRECTION ( 'NONE',  ( 0.9161084732596779245, -5.365801633547218220E-16, -0.4009304992412300317 ) ) ;
#78469 = ORIENTED_EDGE ( 'NONE', *, *, #49228, .F. ) ;
#78470 = CARTESIAN_POINT ( 'NONE',  ( 13.31140876108729998, -18.89465134148960956, 11.49999999999999645 ) ) ;
#78471 = CARTESIAN_POINT ( 'NONE',  ( 20.53691900564983186, 10.01969956684014207, 11.49999999999998934 ) ) ;
#78472 = CARTESIAN_POINT ( 'NONE',  ( -74.54209746499468281, -24.51314013834315375, 0.6176544820404125113 ) ) ;
#78473 = CARTESIAN_POINT ( 'NONE',  ( -96.55228966665733026, -24.15543982623907482, -0.2315651400026596807 ) ) ;
#78474 = CARTESIAN_POINT ( 'NONE',  ( -82.60435760244244818, -23.48786465467241058, 11.44779295918254647 ) ) ;
#78475 = CARTESIAN_POINT ( 'NONE',  ( -1.649324495273077451, -22.40575143947253167, 11.49999999999999645 ) ) ;
#78476 = ORIENTED_EDGE ( 'NONE', *, *, #32591, .F. ) ;
#78477 = CARTESIAN_POINT ( 'NONE',  ( -43.51356542795910798, -23.73766607897671221, -1.055555164236442689 ) ) ;
#78478 = CARTESIAN_POINT ( 'NONE',  ( 21.83198049998918577, 2.282343850347359648, 11.49999999999998934 ) ) ;
#78480 = EDGE_CURVE ( 'NONE', #52307, #77573, #28590, .T. ) ;
#78479 = APPROVAL ( #68858, 'UNKNOWN' ) ;
#78481 = PLANE ( 'NONE',  #21875 ) ;
#78482 = CARTESIAN_POINT ( 'NONE',  ( -34.48363162486440103, -24.51419770103156637, 9.386484678747176957 ) ) ;
#78483 = CARTESIAN_POINT ( 'NONE',  ( -2.899999999999996803, 33.29999999999999716, 2.100000000000000089 ) ) ;
#78484 = VERTEX_POINT ( 'NONE', #49171 ) ;
#78485 = CARTESIAN_POINT ( 'NONE',  ( -48.50690933534888671, -23.96169478059713143, 10.65365249895718236 ) ) ;
#78486 = DIRECTION ( 'NONE',  ( 0.000000000000000000, 0.000000000000000000, -1.000000000000000000 ) ) ;
#78487 = ORIENTED_EDGE ( 'NONE', *, *, #1202, .T. ) ;
#78488 = CARTESIAN_POINT ( 'NONE',  ( -16.05948562299510485, -12.68841425896798469, -1.500000000000002220 ) ) ;
#78489 = ORIENTED_EDGE ( 'NONE', *, *, #61931, .T. ) ;
#78490 = ORIENTED_EDGE ( 'NONE', *, *, #95002, .T. ) ;
#78491 = EDGE_LOOP ( 'NONE', ( #63460, #75622, #39255, #4549 ) ) ;
#78492 = ORIENTED_EDGE ( 'NONE', *, *, #59545, .T. ) ;
#78493 = CARTESIAN_POINT ( 'NONE',  ( -5.126879528927636542, -22.49243673399587351, 11.49999999999998934 ) ) ;
#78494 = CARTESIAN_POINT ( 'NONE',  ( -50.22074830152320146, -25.12160478917137141, 2.838478583573862846 ) ) ;
#78495 = CARTESIAN_POINT ( 'NONE',  ( -12.33117494125061242, 16.09929768045241261, -1.500000000000002220 ) ) ;
#78496 = VERTEX_POINT ( 'NONE', #81096 ) ;
#78497 = CARTESIAN_POINT ( 'NONE',  ( 29.71896661235086157, 4.666145129001815661, 27.69970538640514235 ) ) ;
#78498 = CARTESIAN_POINT ( 'NONE',  ( -37.52287095715008292, -23.48783264083359512, -1.443836473376374885 ) ) ;
#78499 = CARTESIAN_POINT ( 'NONE',  ( -37.62287095715005592, -29.50247984919015209, -1.443849546365060466 ) ) ;
#78500 = CARTESIAN_POINT ( 'NONE',  ( -98.52287095715006160, -23.47596703998600631, 11.44779298504228215 ) ) ;
#78502 = ORIENTED_EDGE ( 'NONE', *, *, #80056, .T. ) ;
#78501 = CARTESIAN_POINT ( 'NONE',  ( 21.22668844964908885, 3.412186807495566132, 11.49999999999999645 ) ) ;
#78503 = CARTESIAN_POINT ( 'NONE',  ( -89.58953762381671027, -24.64965694238407323, 8.947790433994651238 ) ) ;
#78504 = DIRECTION ( 'NONE',  ( -0.000000000000000000, 1.000000000000000000, -0.000000000000000000 ) ) ;
#78505 = ORIENTED_EDGE ( 'NONE', *, *, #27924, .T. ) ;
#78506 = CARTESIAN_POINT ( 'NONE',  ( 20.74337371777590278, 0.4424840333690017724, -1.500000000000002220 ) ) ;
#78507 = ORIENTED_EDGE ( 'NONE', *, *, #31541, .F. ) ;
#78509 = ORIENTED_EDGE ( 'NONE', *, *, #32587, .F. ) ;
#78508 = CARTESIAN_POINT ( 'NONE',  ( -125.5892687586139260, -24.73486907724918638, 1.287355809206972346 ) ) ;
#78510 = CARTESIAN_POINT ( 'NONE',  ( -111.5222191119067645, -23.48786465467241769, 11.44779295918254114 ) ) ;
#78511 = FACE_OUTER_BOUND ( 'NONE', #73275, .T. ) ;
#78512 = ORIENTED_EDGE ( 'NONE', *, *, #35220, .T. ) ;
#78513 = ORIENTED_EDGE ( 'NONE', *, *, #79093, .T. ) ;
#78514 = PLANE ( 'NONE',  #98018 ) ;
#78515 = CARTESIAN_POINT ( 'NONE',  ( -83.62287095715005592, -29.50248528299804818, 1.056150453629038477 ) ) ;
#78516 = CARTESIAN_POINT ( 'NONE',  ( -28.42914491461137061, -24.71144043923981215, 1.770770211163098296 ) ) ;
#78517 = CARTESIAN_POINT ( 'NONE',  ( -17.76638496452178018, -13.01238552544781335, 11.49999999999999645 ) ) ;
#78518 = FACE_BOUND ( 'NONE', #60676, .T. ) ;
#78519 = CARTESIAN_POINT ( 'NONE',  ( 2.010693963185784749, 22.50221635003889276, 11.49999999999998934 ) ) ;
#78520 = CARTESIAN_POINT ( 'NONE',  ( 17.27681320446407298, 11.92757687370068886, -1.500000000000002220 ) ) ;
#78521 = LINE ( 'NONE', #30863, #96166 ) ;
#78523 = ORIENTED_EDGE ( 'NONE', *, *, #90534, .F. ) ;
#78522 = CARTESIAN_POINT ( 'NONE',  ( -70.62287095715005592, -24.99132157543083821, 2.256160258750667502 ) ) ;
#78524 = ADVANCED_FACE ( 'NONE', ( #34426 ), #88716, .F. ) ;
#78525 = ORIENTED_EDGE ( 'NONE', *, *, #36387, .T. ) ;
#78526 = EDGE_CURVE ( 'NONE', #2943, #66070, #24837, .T. ) ;
#78527 = CARTESIAN_POINT ( 'NONE',  ( -59.62287095715007723, -23.47596703998600276, 11.44779298504227683 ) ) ;
#78528 = AXIS2_PLACEMENT_3D ( 'NONE', #89954, #82339, #43789 ) ;
#78529 = CARTESIAN_POINT ( 'NONE',  ( -114.5228709571500758, -23.47593901973090524, -1.443836447538996204 ) ) ;
#78530 = ORIENTED_EDGE ( 'NONE', *, *, #1879, .F. ) ;
#78531 = CARTESIAN_POINT ( 'NONE',  ( 19.19679251752027227, 8.867671107084703408, -1.500000000000002220 ) ) ;
#78532 = DIRECTION ( 'NONE',  ( 0.000000000000000000, -0.9999999999976377785, -2.173523156925979128E-06 ) ) ;
#78533 = CARTESIAN_POINT ( 'NONE',  ( -50.91781549829847364, -25.03148729399882200, 7.505037586422455220 ) ) ;
#78534 = CARTESIAN_POINT ( 'NONE',  ( -121.5888804960365377, -24.51314013834316441, 0.6176544820404217262 ) ) ;
#78535 = CYLINDRICAL_SURFACE ( 'NONE', #94533, 21.89999999999999858 ) ;
#78536 = LINE ( 'NONE', #46113, #24342 ) ;
#78537 = CARTESIAN_POINT ( 'NONE',  ( 8.998109643811913472, -20.30750954041392120, -1.500000000000002220 ) ) ;
#78538 = CARTESIAN_POINT ( 'NONE',  ( -49.44333826525905806, -25.03220847003835559, 7.288210503460494039 ) ) ;
#78539 = EDGE_CURVE ( 'NONE', #12627, #12501, #50652, .T. ) ;
#78540 = AXIS2_PLACEMENT_3D ( 'NONE', #50204, #20732, #28350 ) ;
#78541 = ORIENTED_EDGE ( 'NONE', *, *, #84842, .T. ) ;
#78542 = DIRECTION ( 'NONE',  ( 0.000000000000000000, 1.000000000000000000, 0.000000000000000000 ) ) ;
#78543 = CARTESIAN_POINT ( 'NONE',  ( -37.60092958079493997, -23.96119346886880663, -0.6495511937831990323 ) ) ;
#78544 = FACE_BOUND ( 'NONE', #2920, .T. ) ;
#78545 = CARTESIAN_POINT ( 'NONE',  ( -100.6266800081263284, -24.73486907724917572, 1.287355809206965240 ) ) ;
#78546 = CARTESIAN_POINT ( 'NONE',  ( -100.6000550215268845, -25.11144175452923477, 2.838473218577969082 ) ) ;
#78547 = CARTESIAN_POINT ( 'NONE',  ( 17.91360334016800593, 7.682165803940314674, 11.49999999999998934 ) ) ;
#78548 = CARTESIAN_POINT ( 'NONE',  ( -20.93543047832761417, 4.563121699532205255, 11.49999999999998934 ) ) ;
#78549 = CARTESIAN_POINT ( 'NONE',  ( -89.52287095715006160, -29.50248528299804818, 1.056150453629040253 ) ) ;
#78550 = DIRECTION ( 'NONE',  ( -1.000000000000000000, -0.000000000000000000, -0.000000000000000000 ) ) ;
#78551 = FACE_OUTER_BOUND ( 'NONE', #45501, .T. ) ;
#78552 = CARTESIAN_POINT ( 'NONE',  ( -101.0406423489954477, -25.18440054762538693, 3.494480559635227301 ) ) ;
#78553 = CARTESIAN_POINT ( 'NONE',  ( 20.46598465274837864, -9.837531852206524263, -1.500000000000002220 ) ) ;
#78554 = CARTESIAN_POINT ( 'NONE',  ( -106.5562042904834215, -23.47593901973091235, -1.443836447538999312 ) ) ;
#78555 = CARTESIAN_POINT ( 'NONE',  ( 15.10352928271630724, 2.682774720514426559, -27.29968155418892195 ) ) ;
#78556 = CARTESIAN_POINT ( 'NONE',  ( -9.893332137849947472, -17.22304987741864579, 11.49999999999999645 ) ) ;
#78557 = CARTESIAN_POINT ( 'NONE',  ( -123.5209511861243072, -23.96169478059714564, 10.65365249895717170 ) ) ;
#78558 = CARTESIAN_POINT ( 'NONE',  ( -60.95156673781919920, -25.20074414427590526, 3.409327697718777195 ) ) ;
#78559 = DIRECTION ( 'NONE',  ( 0.000000000000000000, 0.000000000000000000, 1.000000000000000000 ) ) ;
#78560 = ORIENTED_EDGE ( 'NONE', *, *, #41424, .F. ) ;
#78561 = CARTESIAN_POINT ( 'NONE',  ( -49.27764846858840997, -25.25176233969420636, 6.145204990682164414 ) ) ;
#78562 = CARTESIAN_POINT ( 'NONE',  ( -6.377963355984652694, -5.876774720514411854, 19.53740760792478426 ) ) ;
#78563 = CARTESIAN_POINT ( 'NONE',  ( -0.02075734969026423599, -6.475225279485573360, -0.08597719988137648983 ) ) ;
#78564 = CARTESIAN_POINT ( 'NONE',  ( -14.16021466491576675, 16.42052772630311352, -1.500000000000002220 ) ) ;
#78565 = CARTESIAN_POINT ( 'NONE',  ( -115.5228709571500758, -25.00182538069145721, 7.747789668545101094 ) ) ;
#78566 = CARTESIAN_POINT ( 'NONE',  ( 4.731349760756693890, 18.90081699332259646, -1.500000000000002220 ) ) ;
#78567 = CARTESIAN_POINT ( 'NONE',  ( -55.63149466436955493, -24.73531770709094957, 8.716586749053510275 ) ) ;
#78568 = EDGE_CURVE ( 'NONE', #62952, #92846, #24996, .T. ) ;
#78569 = ORIENTED_EDGE ( 'NONE', *, *, #69765, .T. ) ;
#78570 = AXIS2_PLACEMENT_3D ( 'NONE', #36291, #20544, #90073 ) ;
#78571 = CARTESIAN_POINT ( 'NONE',  ( 2.554409723529738052, 20.22502395925995700, 11.49999999999999645 ) ) ;
#78572 = CARTESIAN_POINT ( 'NONE',  ( -84.62287095715005592, -29.50247984919015209, -1.443849546365053582 ) ) ;
#78573 = EDGE_CURVE ( 'NONE', #66070, #56729, #89713, .T. ) ;
#78574 = CARTESIAN_POINT ( 'NONE',  ( -107.6228709571500701, -29.50250786944525672, 11.44777988621622988 ) ) ;
#78575 = VERTEX_POINT ( 'NONE', #96323 ) ;
#78576 = DIRECTION ( 'NONE',  ( -1.000000000000000000, -0.000000000000000000, -0.000000000000000000 ) ) ;
#78577 = LINE ( 'NONE', #72498, #67189 ) ;
#78578 = CARTESIAN_POINT ( 'NONE',  ( -39.42702772597635175, -25.27985508946863291, 5.331662265757392660 ) ) ;
#78579 = CARTESIAN_POINT ( 'NONE',  ( -40.58885790174546315, -24.52399227489126687, 9.353111116836521077 ) ) ;
#78580 = CARTESIAN_POINT ( 'NONE',  ( -0.4686347352592966087, -6.376774720514411854, 19.46274624311237034 ) ) ;
#78581 = CARTESIAN_POINT ( 'NONE',  ( 10.48293302797296356, 17.13603372422173976, -1.500000000000002220 ) ) ;
#78582 = CARTESIAN_POINT ( 'NONE',  ( 23.57151214508650128, 3.870844576848782668E-15, 0.000000000000000000 ) ) ;
#78583 = ORIENTED_EDGE ( 'NONE', *, *, #50981, .F. ) ;
#78584 = CARTESIAN_POINT ( 'NONE',  ( -66.63133170827177310, -24.35071581493543036, 9.817618358456028815 ) ) ;
#78585 = CARTESIAN_POINT ( 'NONE',  ( -3.094460115123966570, -22.75893099265358188, 11.49999999999999645 ) ) ;
#78586 = CARTESIAN_POINT ( 'NONE',  ( 11.07647423179810531, -19.82844882884714366, -1.500000000000002220 ) ) ;
#78587 = ORIENTED_EDGE ( 'NONE', *, *, #64503, .T. ) ;
#78588 = CARTESIAN_POINT ( 'NONE',  ( 3.675000000000002487, 14.49999999999999822, 24.00000000000000000 ) ) ;
#78589 = CARTESIAN_POINT ( 'NONE',  ( -91.62287095715005592, -23.48786465467241769, 11.44779295918254114 ) ) ;
#78590 = CARTESIAN_POINT ( 'NONE',  ( -38.49109438492880741, -24.35071581493542325, 9.817618358456030592 ) ) ;
#78591 = FACE_OUTER_BOUND ( 'NONE', #9971, .T. ) ;
#78592 = VECTOR ( 'NONE', #41440, 1000.000000000000114 ) ;
#78593 = CC_DESIGN_PERSON_AND_ORGANIZATION_ASSIGNMENT ( #30774, #16535, ( #14113 ) ) ;
#78594 = CARTESIAN_POINT ( 'NONE',  ( -128.5898162796150075, -24.15620529776629510, 10.23563542870659404 ) ) ;
#78595 = CARTESIAN_POINT ( 'NONE',  ( -26.19597845478084608, -24.90840837394421570, 3.802218847965264992 ) ) ;
#78596 = DIRECTION ( 'NONE',  ( 1.000000000000000000, 0.000000000000000000, 0.000000000000000000 ) ) ;
#78597 = CARTESIAN_POINT ( 'NONE',  ( -98.92944106970213625, -25.25460656324785447, 5.790834282400935784 ) ) ;
#78598 = ORIENTED_EDGE ( 'NONE', *, *, #77992, .T. ) ;
#78599 = CARTESIAN_POINT ( 'NONE',  ( -13.40315722217803973, 15.35114911505495172, 11.49999999999998934 ) ) ;
#78600 = ORIENTED_EDGE ( 'NONE', *, *, #71737, .F. ) ;
#78601 = CARTESIAN_POINT ( 'NONE',  ( -22.63010559926462051, 4.001702944626347680, -1.500000000000002220 ) ) ;
#78602 = CARTESIAN_POINT ( 'NONE',  ( -7.282824509310913186, -5.876774720514415407, 19.84584863393302356 ) ) ;
#78603 = VECTOR ( 'NONE', #98744, 1000.000000000000114 ) ;
#78605 = ORIENTED_EDGE ( 'NONE', *, *, #3766, .F. ) ;
#78604 = EDGE_CURVE ( 'NONE', #91590, #94426, #42555, .T. ) ;
#78606 = CARTESIAN_POINT ( 'NONE',  ( 19.24418710706453339, 0.000000000000000000, 2.346898003627108320 ) ) ;
#78607 = CARTESIAN_POINT ( 'NONE',  ( -35.52287095715008292, -25.00182538069144655, 7.747789668545105535 ) ) ;
#78608 = AXIS2_PLACEMENT_3D ( 'NONE', #98206, #5869, #68773 ) ;
#78609 = B_SPLINE_CURVE_WITH_KNOTS ( 'NONE', 3,
 ( #42912, #81959, #74347, #2857 ),
 .UNSPECIFIED., .F., .F.,
 ( 4, 4 ),
 ( 0.000000000000000000, 9.999999999998897304E-05 ),
 .UNSPECIFIED. ) ;
#78610 = FACE_OUTER_BOUND ( 'NONE', #66045, .T. ) ;
#78612 = VERTEX_POINT ( 'NONE', #12070 ) ;
#78611 = CARTESIAN_POINT ( 'NONE',  ( -3.453506354162970915, -21.03206338698385736, 11.49999999999999645 ) ) ;
#78613 = ORIENTED_EDGE ( 'NONE', *, *, #12988, .F. ) ;
#78614 = CARTESIAN_POINT ( 'NONE',  ( 7.688942331755139747, 20.87172568467934752, 11.49999999999998934 ) ) ;
#78615 = CARTESIAN_POINT ( 'NONE',  ( 10.45329875151443488, -17.81600612866554556, 11.49999999999998934 ) ) ;
#78616 = ORIENTED_EDGE ( 'NONE', *, *, #9337, .T. ) ;
#78617 = CARTESIAN_POINT ( 'NONE',  ( -4.886549725601808447, -6.376774720514410077, 19.15251819062245175 ) ) ;
#78618 = CARTESIAN_POINT ( 'NONE',  ( -95.54720254560318438, -24.63419186844610920, 9.035850630976922204 ) ) ;
#78619 = VERTEX_POINT ( 'NONE', #57288 ) ;
#78620 = CARTESIAN_POINT ( 'NONE',  ( -115.5228709571500616, -23.48786465467241769, 11.44779295918253759 ) ) ;
#78621 = VERTEX_POINT ( 'NONE', #4970 ) ;
#78622 = CARTESIAN_POINT ( 'NONE',  ( -49.58953762381672448, -23.48783264082478084, -1.443836473390070596 ) ) ;
#78623 = CARTESIAN_POINT ( 'NONE',  ( -71.25210310630363608, -25.21189915732672659, 6.509906768301197744 ) ) ;
#78624 = CARTESIAN_POINT ( 'NONE',  ( 4.135342931496230001, -20.44547621892628797, -1.500000000000002220 ) ) ;
#78625 = EDGE_CURVE ( 'NONE', #16766, #86042, #78179, .T. ) ;
#78626 = CARTESIAN_POINT ( 'NONE',  ( 0.003323472525107682655, -21.86402403546210493, 11.49999999999999645 ) ) ;
#78627 = CARTESIAN_POINT ( 'NONE',  ( 26.14999174255633463, -4.132774720517320866, -11.56127575336603286 ) ) ;
#78628 = DIRECTION ( 'NONE',  ( 0.000000000000000000, 0.9999999999976377785, 2.173523156925979128E-06 ) ) ;
#78629 = CARTESIAN_POINT ( 'NONE',  ( 20.52096793114426276, -9.243637136814692568, 11.49999999999998934 ) ) ;
#78630 = CARTESIAN_POINT ( 'NONE',  ( -118.6249400182559413, -24.35071581493543746, 9.817618358456019934 ) ) ;
#78631 = DIRECTION ( 'NONE',  ( -0.06916465693916189206, 0.000000000000000000, 0.9976052577199502336 ) ) ;
#78632 = CARTESIAN_POINT ( 'NONE',  ( -59.62287095715007723, -23.47596703998600276, 11.44779298504227683 ) ) ;
#78633 = ORIENTED_EDGE ( 'NONE', *, *, #24680, .T. ) ;
#78634 = AXIS2_PLACEMENT_3D ( 'NONE', #87465, #46404, #77336 ) ;
#78635 = EDGE_CURVE ( 'NONE', #58197, #73050, #96351, .T. ) ;
#78636 = ORIENTED_EDGE ( 'NONE', *, *, #34577, .F. ) ;
#78637 = ORIENTED_EDGE ( 'NONE', *, *, #61307, .F. ) ;
#78638 = EDGE_CURVE ( 'NONE', #13348, #63463, #56289, .T. ) ;
#78639 = EDGE_LOOP ( 'NONE', ( #88983, #26260, #28121, #71056 ) ) ;
#78640 = CARTESIAN_POINT ( 'NONE',  ( 15.12546962493697933, 15.13007008128210096, -1.500000000000002220 ) ) ;
#78641 = CARTESIAN_POINT ( 'NONE',  ( -9.622923231576368863, -20.19340101508991125, 11.49999999999999645 ) ) ;
#78642 = ORIENTED_EDGE ( 'NONE', *, *, #88660, .T. ) ;
#78643 = CARTESIAN_POINT ( 'NONE',  ( 19.40125262130244366, -8.172613994405130811, -1.500000000000002220 ) ) ;
#78644 = CARTESIAN_POINT ( 'NONE',  ( -30.48447787840913392, -24.66679253312401698, 8.908675929220798650 ) ) ;
#78645 = CARTESIAN_POINT ( 'NONE',  ( 2.927915493035635031, 19.71835975189664936, -1.500000000000002220 ) ) ;
#78646 = CARTESIAN_POINT ( 'NONE',  ( -50.62611156557186121, -24.92592662359560762, 8.075495903017996469 ) ) ;
#78647 = CARTESIAN_POINT ( 'NONE',  ( -61.62287095715004881, -23.48783264082478439, -1.443836473390069042 ) ) ;
#78648 = CARTESIAN_POINT ( 'NONE',  ( -10.13730173486854369, -19.54584281717935568, -1.500000000000002220 ) ) ;
#78649 = CARTESIAN_POINT ( 'NONE',  ( -83.52287095715009002, -24.33832256527049509, 0.1851278514138626485 ) ) ;
#78650 = ORIENTED_EDGE ( 'NONE', *, *, #80131, .T. ) ;
#78651 = CARTESIAN_POINT ( 'NONE',  ( -102.5228709571500758, -24.64898659630367916, 1.056161002820829697 ) ) ;
#78652 = EDGE_CURVE ( 'NONE', #57426, #59325, #75461, .T. ) ;
#78653 = CARTESIAN_POINT ( 'NONE',  ( 282.9764569301858046, 5.965225279485572685, 20.79159422840526616 ) ) ;
#78654 = CARTESIAN_POINT ( 'NONE',  ( -16.21995886604411297, 13.06735728859114509, 11.49999999999999645 ) ) ;
#78655 = DIRECTION ( 'NONE',  ( -1.000000000000000000, -3.491481338843132961E-15, -2.352173255807796056E-16 ) ) ;
#78656 = PLANE ( 'NONE',  #23006 ) ;
#78657 = DIRECTION ( 'NONE',  ( -0.000000000000000000, 1.000000000000000000, -0.000000000000000000 ) ) ;
#78658 = CARTESIAN_POINT ( 'NONE',  ( -18.01091527469349529, -11.40912366963296698, -1.500000000000002220 ) ) ;
#78659 = DIRECTION ( 'NONE',  ( -3.773278334453079030E-23, 0.9999999999976377785, 2.173523156925979128E-06 ) ) ;
#78660 = B_SPLINE_CURVE_WITH_KNOTS ( 'NONE', 3,
 ( #62057, #53948, #7756, #46831, #15358, #23974, #45826, #61062, #39201, #77747, #15861, #99585, #16868, #63066 ),
 .UNSPECIFIED., .F., .F.,
 ( 4, 2, 2, 2, 2, 2, 4 ),
 ( 1.915770205925381696E-16, 0.0001882564892122831591, 0.0003765129784243747397, 0.0007530259568485313379, 0.001129538935272687882, 0.001317795424484765991, 0.001506051913696843884 ),
 .UNSPECIFIED. ) ;
#78661 = CARTESIAN_POINT ( 'NONE',  ( -66.62287095715009855, -23.94994826722565762, -0.6494450866342729167 ) ) ;
#78662 = CARTESIAN_POINT ( 'NONE',  ( -71.62287095715005592, -24.65952944569304606, 1.056160979905699016 ) ) ;
#78663 = LINE ( 'NONE', #40130, #62170 ) ;
#78664 = CARTESIAN_POINT ( 'NONE',  ( -21.23328875057882570, -7.520457577684837247, -1.500000000000002220 ) ) ;
#78665 = VECTOR ( 'NONE', #67790, 1000.000000000000114 ) ;
#78666 = DIRECTION ( 'NONE',  ( 0.000000000000000000, -1.000000000000000000, 0.000000000000000000 ) ) ;
#78667 = ORIENTED_EDGE ( 'NONE', *, *, #53059, .T. ) ;
#78668 = CARTESIAN_POINT ( 'NONE',  ( -78.94303308397306296, -25.26642230834568537, 5.977536689587218177 ) ) ;
#78669 = CARTESIAN_POINT ( 'NONE',  ( 7.160000000000000142, -10.77121780415746599, 1.154761385154455366 ) ) ;
#78670 = CARTESIAN_POINT ( 'NONE',  ( 6.681059570357060551, -18.48443787736713873, 11.49999999999999645 ) ) ;
#78671 = CARTESIAN_POINT ( 'NONE',  ( -93.62287095715005592, -23.48786465467241769, 11.44779295918254114 ) ) ;
#78672 = AXIS2_PLACEMENT_3D ( 'NONE', #50231, #97395, #43116 ) ;
#78673 = CARTESIAN_POINT ( 'NONE',  ( -28.47875734969025885, -5.965225279485572685, -0.08597719988137300651 ) ) ;
#78674 = ORIENTED_EDGE ( 'NONE', *, *, #10960, .T. ) ;
#78675 = AXIS2_PLACEMENT_3D ( 'NONE', #60785, #91701, #22185 ) ;
#78676 = CARTESIAN_POINT ( 'NONE',  ( -111.5228709571500616, -23.47593901973090524, -1.443836447538996204 ) ) ;
#78677 = CARTESIAN_POINT ( 'NONE',  ( -88.88918693012689687, -25.27880950044345454, 5.947789066509454159 ) ) ;
#78678 = CARTESIAN_POINT ( 'NONE',  ( -124.5216656005884062, -23.73791477778912551, 11.05961554403169878 ) ) ;
#78679 = AXIS2_PLACEMENT_3D ( 'NONE', #99916, #60897, #69991 ) ;
#78680 = DIRECTION ( 'NONE',  ( -3.773278334453079618E-23, 0.9999999999976377785, 2.173523156925979975E-06 ) ) ;
#78681 = CARTESIAN_POINT ( 'NONE',  ( -3.970774856468506364, -19.35638658347046714, -1.500000000000002220 ) ) ;
#78682 = ORIENTED_EDGE ( 'NONE', *, *, #34618, .T. ) ;
#78683 = CARTESIAN_POINT ( 'NONE',  ( -14.42758394406654610, -14.16023863206117994, 11.49999999999999645 ) ) ;
#78684 = CARTESIAN_POINT ( 'NONE',  ( 7.822518687475809251, 6.376774720514094774, -28.18023264526767591 ) ) ;
#78685 = EDGE_CURVE ( 'NONE', #88761, #13521, #36915, .T. ) ;
#78686 = COORDINATED_UNIVERSAL_TIME_OFFSET ( 0, 0, .AHEAD. ) ;
#78687 = ORIENTED_EDGE ( 'NONE', *, *, #29252, .F. ) ;
#78688 = FACE_OUTER_BOUND ( 'NONE', #14207, .T. ) ;
#78689 = CARTESIAN_POINT ( 'NONE',  ( -41.58953762381673158, -23.47596703998600276, 11.44779298504227505 ) ) ;
#78690 = PLANE ( 'NONE',  #75201 ) ;
#78691 = CARTESIAN_POINT ( 'NONE',  ( 5.641025641025643189, -6.376774720514420736, 20.78665865384615330 ) ) ;
#78692 = CARTESIAN_POINT ( 'NONE',  ( -41.58953762381673869, -24.66019654487199020, 8.947790411086133489 ) ) ;
#78693 = CARTESIAN_POINT ( 'NONE',  ( -41.32836283488544638, -2.803225279485573207, 39.26872235229541985 ) ) ;
#78694 = CARTESIAN_POINT ( 'NONE',  ( 7.431233518514567926, -18.57414813805618081, 11.49999999999998934 ) ) ;
#78695 = CARTESIAN_POINT ( 'NONE',  ( -79.52287095715006160, -29.50248528299804818, 1.056150453629038477 ) ) ;
#78696 = CARTESIAN_POINT ( 'NONE',  ( -89.81226385320383088, -25.27367468601175204, 3.993462154588550916 ) ) ;
#78697 = ORIENTED_EDGE ( 'NONE', *, *, #29367, .T. ) ;
#78698 = CARTESIAN_POINT ( 'NONE',  ( -79.51716134780556899, -23.73791477778911840, 11.05961554403170943 ) ) ;
#78699 = B_SPLINE_CURVE_WITH_KNOTS ( 'NONE', 3,
 ( #70841, #17041, #48008, #71342, #77425, #16033 ),
 .UNSPECIFIED., .F., .F.,
 ( 4, 2, 4 ),
 ( 0.000000000000000000, 0.001380901958385382473, 0.002761803916770764946 ),
 .UNSPECIFIED. ) ;
#78700 = CARTESIAN_POINT ( 'NONE',  ( -73.58953762381673869, -23.47596703998600276, 11.44779298504227683 ) ) ;
#78701 = LINE ( 'NONE', #37662, #81803 ) ;
#78702 = CARTESIAN_POINT ( 'NONE',  ( -9.543201319291914093E-14, -5.876774720514426953, 18.21871304725679508 ) ) ;
#78703 = PLANE ( 'NONE',  #95051 ) ;
#78704 = CARTESIAN_POINT ( 'NONE',  ( -83.50991238427990027, -24.15543982623907127, -0.2315651400026649820 ) ) ;
#78705 = EDGE_CURVE ( 'NONE', #65522, #15238, #20683, .T. ) ;
#78706 = DIRECTION ( 'NONE',  ( 0.000000000000000000, -0.9999999999976377785, -2.173523156925979128E-06 ) ) ;
#78707 = CARTESIAN_POINT ( 'NONE',  ( -84.55620429048340725, -24.64898659630528854, 1.056161002820828143 ) ) ;
#78708 = EDGE_LOOP ( 'NONE', ( #15966, #81058, #17945, #82102 ) ) ;
#78709 = EDGE_CURVE ( 'NONE', #64573, #42081, #29800, .T. ) ;
#78710 = CARTESIAN_POINT ( 'NONE',  ( 2.303441031721801480, -20.17751241584783628, -1.500000000000002220 ) ) ;
#78711 = CARTESIAN_POINT ( 'NONE',  ( -115.2228709571500644, -23.47593901973090524, -1.443836447538996426 ) ) ;
#78712 = PLANE ( 'NONE',  #40349 ) ;
#78713 = ADVANCED_FACE ( 'NONE', ( #6966, #82592 ), #84083, .F. ) ;
#78714 = CARTESIAN_POINT ( 'NONE',  ( -107.5228709571500758, -23.48786465467241769, 11.44779295918253936 ) ) ;
#78715 = EDGE_CURVE ( 'NONE', #62896, #88543, #44030, .T. ) ;
#78716 = AXIS2_PLACEMENT_3D ( 'NONE', #31791, #70860, #84070 ) ;
#78717 = ORIENTED_EDGE ( 'NONE', *, *, #53363, .F. ) ;
#78718 = CARTESIAN_POINT ( 'NONE',  ( -86.52287095715003318, -23.73934037231757088, 11.05740245334329330 ) ) ;
#78719 = CARTESIAN_POINT ( 'NONE',  ( -15.35229381799144299, -13.07563953244551591, -1.500000000000002220 ) ) ;
#78720 = CARTESIAN_POINT ( 'NONE',  ( -12.37649675270136918, 17.12833386298736471, 11.49999999999999645 ) ) ;
#78721 = EDGE_CURVE ( 'NONE', #37238, #29179, #87722, .T. ) ;
#78722 = CARTESIAN_POINT ( 'NONE',  ( 21.58644828898399481, -4.983269013152989757, 11.49999999999998934 ) ) ;
#78723 = CARTESIAN_POINT ( 'NONE',  ( -20.56140336115741718, 0.6910293267889283664, -1.500000000000002220 ) ) ;
#78724 = VECTOR ( 'NONE', #41562, 1000.000000000000000 ) ;
#78725 = CARTESIAN_POINT ( 'NONE',  ( -42.62287095715004881, -29.50250786944525672, 11.44777988621624232 ) ) ;
#78726 = EDGE_LOOP ( 'NONE', ( #3381, #24579, #32831, #38709 ) ) ;
#78727 = LINE ( 'NONE', #64060, #24951 ) ;
#78728 = ORIENTED_EDGE ( 'NONE', *, *, #52057, .F. ) ;
#78729 = DIRECTION ( 'NONE',  ( 0.000000000000000000, 2.173523156925980399E-06, -0.9999999999976378895 ) ) ;
#78730 = FACE_OUTER_BOUND ( 'NONE', #19919, .T. ) ;
#78731 = ORIENTED_EDGE ( 'NONE', *, *, #5353, .F. ) ;
#78732 = VECTOR ( 'NONE', #57477, 1000.000000000000000 ) ;
#78733 = B_SPLINE_CURVE_WITH_KNOTS ( 'NONE', 3,
 ( #70868, #341, #15561, #85574 ),
 .UNSPECIFIED., .F., .F.,
 ( 4, 4 ),
 ( 0.07881234897532776729, 0.07981309601609325177 ),
 .UNSPECIFIED. ) ;
#78734 = ORIENTED_EDGE ( 'NONE', *, *, #62971, .F. ) ;
#78735 = AXIS2_PLACEMENT_3D ( 'NONE', #38753, #95930, #199 ) ;
#78736 = ORIENTED_EDGE ( 'NONE', *, *, #50792, .T. ) ;
#78737 = CARTESIAN_POINT ( 'NONE',  ( -81.62287095715005592, -24.50321055353803956, 9.387540953477527594 ) ) ;
#78738 = CARTESIAN_POINT ( 'NONE',  ( -127.6228709571501412, -24.35013146730205236, 9.818937971375101270 ) ) ;
#78739 = CARTESIAN_POINT ( 'NONE',  ( 6.058092820189922456, -6.376774720514413630, 19.77091638250125882 ) ) ;
#78740 = CARTESIAN_POINT ( 'NONE',  ( -14.56105648253378781, -14.73650127990469016, -1.500000000000002220 ) ) ;
#78741 = EDGE_CURVE ( 'NONE', #93091, #76257, #75962, .T. ) ;
#78742 = AXIS2_PLACEMENT_3D ( 'NONE', #94419, #1078, #64005 ) ;
#78743 = CARTESIAN_POINT ( 'NONE',  ( 12.10466045530642631, 18.00204671274030233, 11.49999999999999645 ) ) ;
#78744 = ORIENTED_EDGE ( 'NONE', *, *, #74730, .F. ) ;
#78745 = DIRECTION ( 'NONE',  ( 1.000000000000000000, 0.000000000000000000, 0.000000000000000000 ) ) ;
#78746 = CARTESIAN_POINT ( 'NONE',  ( -102.6228709571500559, -29.50250786944525672, 11.44777988621623166 ) ) ;
#78747 = CARTESIAN_POINT ( 'NONE',  ( 8.126467401150291536, 20.86698325809501497, -1.500000000000002220 ) ) ;
#78748 = AXIS2_PLACEMENT_3D ( 'NONE', #75351, #98691, #83466 ) ;
#78749 = CARTESIAN_POINT ( 'NONE',  ( -66.92287095715005307, -23.47596703998600276, 11.44779298504227860 ) ) ;
#78750 = DIRECTION ( 'NONE',  ( -0.000000000000000000, 1.000000000000000000, -1.084202172485504434E-16 ) ) ;
#78751 = EDGE_LOOP ( 'NONE', ( #7736, #87267, #62164, #29599 ) ) ;
#78752 = CARTESIAN_POINT ( 'NONE',  ( 32.84232313084854837, -4.840274619473185602, -11.71291885348858663 ) ) ;
#78753 = CARTESIAN_POINT ( 'NONE',  ( -52.62287095715005592, -24.64965695001467694, 8.947790433994185832 ) ) ;
#78754 = VERTEX_POINT ( 'NONE', #5467 ) ;
#78755 = ORIENTED_EDGE ( 'NONE', *, *, #68448, .T. ) ;
#78757 = EDGE_CURVE ( 'NONE', #18993, #66329, #93826, .T. ) ;
#78756 = CARTESIAN_POINT ( 'NONE',  ( -87.62287095715001328, -23.48786465467241769, 11.44779295918254114 ) ) ;
#78758 = VERTEX_POINT ( 'NONE', #98298 ) ;
#78759 = DIRECTION ( 'NONE',  ( 0.000000000000000000, 1.000000000000000000, 0.000000000000000000 ) ) ;
#78760 = CARTESIAN_POINT ( 'NONE',  ( -13.45780860896912934, -16.40347334334247265, -1.500000000000002220 ) ) ;
#78761 = EDGE_CURVE ( 'NONE', #46787, #79347, #98808, .T. ) ;
#78762 = VERTEX_POINT ( 'NONE', #7454 ) ;
#78763 = DIRECTION ( 'NONE',  ( -3.773278334453079030E-23, 0.9999999999976377785, 2.173523156925979128E-06 ) ) ;
#78764 = CARTESIAN_POINT ( 'NONE',  ( 8.287826148123016878, -20.17477452812186201, -1.500000000000002220 ) ) ;
#78765 = CARTESIAN_POINT ( 'NONE',  ( -52.56778115561136389, -23.48786465467241058, 11.44779295918255357 ) ) ;
#78766 = CARTESIAN_POINT ( 'NONE',  ( 0.000000000000000000, -16.94322527948557422, 0.000000000000000000 ) ) ;
#78767 = CARTESIAN_POINT ( 'NONE',  ( 0.7051282051282027341, -6.376774720514408301, 19.19230769230768985 ) ) ;
#78768 = CARTESIAN_POINT ( 'NONE',  ( 21.06710269851327766, -5.618397932909799941, -1.500000000000002220 ) ) ;
#78769 = CARTESIAN_POINT ( 'NONE',  ( -1.122631020312409245, -6.376774720514411854, 19.41635569784906679 ) ) ;
#78770 = VERTEX_POINT ( 'NONE', #14064 ) ;
#78771 = CARTESIAN_POINT ( 'NONE',  ( -41.62287095715006302, -24.64898659630367561, 1.056161002820819261 ) ) ;
#78772 = CARTESIAN_POINT ( 'NONE',  ( -48.91945971812886995, -25.12782585385058098, 6.515678671521449417 ) ) ;
#78774 = VERTEX_POINT ( 'NONE', #21182 ) ;
#78773 = EDGE_CURVE ( 'NONE', #44074, #70398, #21209, .T. ) ;
#78776 = CIRCLE ( 'NONE', #62580, 27.94799999999999685 ) ;
#78775 = CARTESIAN_POINT ( 'NONE',  ( -129.6235879299834153, -24.35071581493544457, 9.817618358456021710 ) ) ;
#78777 = EDGE_CURVE ( 'NONE', #2769, #81670, #3095, .T. ) ;
#78778 = EDGE_LOOP ( 'NONE', ( #2508, #28836, #78490, #32354, #82389, #68886 ) ) ;
#78779 = EDGE_CURVE ( 'NONE', #88839, #19118, #42987, .T. ) ;
#78780 = ORIENTED_EDGE ( 'NONE', *, *, #76913, .F. ) ;
#78781 = CARTESIAN_POINT ( 'NONE',  ( 10.86264265030973952, 0.3587747205144257157, -28.64597719988137570 ) ) ;
#78782 = DIRECTION ( 'NONE',  ( 3.491481338843133355E-15, -1.000000000000000000, 2.352173255807804438E-16 ) ) ;
#78783 = CARTESIAN_POINT ( 'NONE',  ( -15.86343167427570577, 14.10970434637795634, 11.49999999999998934 ) ) ;
#78784 = CARTESIAN_POINT ( 'NONE',  ( -6.660000000000001030, -10.97586050609889163, -0.8902240841051124454 ) ) ;
#78785 = CARTESIAN_POINT ( 'NONE',  ( -30.59128290392954597, -24.93418366566757882, 8.369064737642425200 ) ) ;
#78786 = CARTESIAN_POINT ( 'NONE',  ( -44.55620429048338593, -23.48786465467240347, 11.44779295918255180 ) ) ;
#78787 = CARTESIAN_POINT ( 'NONE',  ( -8.160000000000000142, -9.074990544709798712, -0.7360493640965781736 ) ) ;
#78788 = CARTESIAN_POINT ( 'NONE',  ( 15.46825748771582631, 11.69065726450791409, 11.49999999999998934 ) ) ;
#78789 = CARTESIAN_POINT ( 'NONE',  ( -45.58893347773089744, -24.52300882791528380, 0.6510814631126234930 ) ) ;
#78790 = ORIENTED_EDGE ( 'NONE', *, *, #79662, .F. ) ;
#78791 = CARTESIAN_POINT ( 'NONE',  ( -4.042178566331402045, 19.10766070095605684, 11.49999999999999645 ) ) ;
#78792 = CARTESIAN_POINT ( 'NONE',  ( -5.486124437288584232, -5.876774720514415407, 19.74568812963598319 ) ) ;
#78793 = DIRECTION ( 'NONE',  ( -0.000000000000000000, 1.000000000000000000, -0.000000000000000000 ) ) ;
#78794 = ORIENTED_EDGE ( 'NONE', *, *, #72055, .F. ) ;
#78795 = CARTESIAN_POINT ( 'NONE',  ( 4.885870204371583370, -5.876774720514419847, 20.85936027411790405 ) ) ;
#78796 = CARTESIAN_POINT ( 'NONE',  ( -89.63470083817112766, -23.96119346886881019, -0.6495511937831908167 ) ) ;
#78797 = AXIS2_PLACEMENT_3D ( 'NONE', #56646, #42428, #17057 ) ;
#78798 = CARTESIAN_POINT ( 'NONE',  ( -30.57287095715004099, -23.47593903913510260, -1.434903445928520149 ) ) ;
#78799 = CARTESIAN_POINT ( 'NONE',  ( -101.0975906728528884, -25.21813695808114630, 3.546416755389510289 ) ) ;
#78800 = CARTESIAN_POINT ( 'NONE',  ( -19.61143073682725202, -1.510137823221562092, -1.500000000000002220 ) ) ;
#78801 = ORIENTED_EDGE ( 'NONE', *, *, #13972, .F. ) ;
#78802 = CARTESIAN_POINT ( 'NONE',  ( 20.55510029441247610, -6.647428040031946317, 11.49999999999998934 ) ) ;
#78803 = CARTESIAN_POINT ( 'NONE',  ( 4.784292611718076849, 5.356774720514425603, -25.54547254883186014 ) ) ;
#78804 = CARTESIAN_POINT ( 'NONE',  ( 22.94779996701378266, 2.684060219229261968, -1.500000000000002220 ) ) ;
#78805 = VECTOR ( 'NONE', #70117, 1000.000000000000000 ) ;
#78806 = APPROVAL_ROLE ( '' ) ;
#78807 = CARTESIAN_POINT ( 'NONE',  ( 3.671066620544169101, -6.376774720514424288, 21.47597918715562670 ) ) ;
#78808 = CARTESIAN_POINT ( 'NONE',  ( -115.5228709571500474, -23.47593901973090524, -1.443836447538996204 ) ) ;
#78809 = CARTESIAN_POINT ( 'NONE',  ( -97.55239203327073483, -24.15620529776628800, 10.23563542870660115 ) ) ;
#78810 = DIRECTION ( 'NONE',  ( 0.000000000000000000, -1.000000000000000000, 0.000000000000000000 ) ) ;
#78811 = AXIS2_PLACEMENT_3D ( 'NONE', #90355, #67530, #27958 ) ;
#78813 = DIRECTION ( 'NONE',  ( 0.000000000000000000, 0.9999999999976377785, 2.173523156925979975E-06 ) ) ;
#78812 = AXIS2_PLACEMENT_3D ( 'NONE', #71787, #58074, #47949 ) ;
#78814 = CARTESIAN_POINT ( 'NONE',  ( -129.5219952696967312, -24.15543982623907482, -0.2315651400026527140 ) ) ;
#78815 = B_SPLINE_CURVE_WITH_KNOTS ( 'NONE', 3,
 ( #9379, #86505, #47957, #78878, #32716, #63700 ),
 .UNSPECIFIED., .F., .F.,
 ( 4, 2, 4 ),
 ( 0.000000000000000000, 0.001380764517854768218, 0.002761529035709536437 ),
 .UNSPECIFIED. ) ;
#78816 = CARTESIAN_POINT ( 'NONE',  ( -114.5180505893580829, -24.15620529776629510, 10.23563542870659404 ) ) ;
#78817 = CARTESIAN_POINT ( 'NONE',  ( -4.359361796094493258, -19.42695174060331809, -1.500000000000002220 ) ) ;
#78818 = CARTESIAN_POINT ( 'NONE',  ( -75.48965661426149154, -25.00182538069146787, 7.747789668545045139 ) ) ;
#78819 = CARTESIAN_POINT ( 'NONE',  ( 19.22361159462649027, -4.937694622890139939, -1.500000000000002220 ) ) ;
#78820 = ORIENTED_EDGE ( 'NONE', *, *, #34931, .T. ) ;
#78821 = AXIS2_PLACEMENT_3D ( 'NONE', #20067, #43425, #52522 ) ;
#78822 = CARTESIAN_POINT ( 'NONE',  ( -56.64375047002581454, -23.96119346886880663, -0.6495511937832126881 ) ) ;
#78823 = DIRECTION ( 'NONE',  ( -3.773278334453079618E-23, 0.9999999999976377785, 2.173523156925979975E-06 ) ) ;
#78824 = DIRECTION ( 'NONE',  ( 0.5473052603538087757, -5.646564643389147554E-15, 0.8369330630277725946 ) ) ;
#78825 = CARTESIAN_POINT ( 'NONE',  ( 20.64725891757762355, 2.036748910689437864, 11.49999999999999645 ) ) ;
#78826 = PLANE ( 'NONE',  #80733 ) ;
#78827 = PLANE ( 'NONE',  #63600 ) ;
#78828 = CARTESIAN_POINT ( 'NONE',  ( 21.64774270073068863, 7.000884456547583845, 11.49999999999999645 ) ) ;
#78830 = ADVANCED_FACE ( 'NONE', ( #8962 ), #31308, .T. ) ;
#78829 = ORIENTED_EDGE ( 'NONE', *, *, #55333, .T. ) ;
#78831 = CARTESIAN_POINT ( 'NONE',  ( -83.62287095715007013, -23.48786465467241769, 11.44779295918254469 ) ) ;
#78833 = EDGE_CURVE ( 'NONE', #61303, #63682, #25181, .T. ) ;
#78832 = CARTESIAN_POINT ( 'NONE',  ( -38.52287095715007581, -24.34917612407050314, 0.1852690917482237298 ) ) ;
#78834 = ORIENTED_EDGE ( 'NONE', *, *, #17185, .F. ) ;
#78835 = CARTESIAN_POINT ( 'NONE',  ( -17.27845874757997535, -10.49745931960568335, -1.500000000000002220 ) ) ;
#78836 = CARTESIAN_POINT ( 'NONE',  ( 30.53060340732035982, 4.594240983522013266, 19.84760796525321780 ) ) ;
#78837 = CARTESIAN_POINT ( 'NONE',  ( 22.81105451610979173, 500000.0000000000582, -18.46691820600746681 ) ) ;
#78838 = VECTOR ( 'NONE', #1405, 1000.000000000000000 ) ;
#78839 = EDGE_CURVE ( 'NONE', #92960, #87632, #70826, .T. ) ;
#78840 = ADVANCED_FACE ( 'NONE', ( #93692 ), #1379, .T. ) ;
#78841 = ORIENTED_EDGE ( 'NONE', *, *, #29755, .F. ) ;
#78842 = CARTESIAN_POINT ( 'NONE',  ( -0.1426030150137709562, -21.20389190742572083, 11.50200000000000422 ) ) ;
#78843 = CARTESIAN_POINT ( 'NONE',  ( 10.67403711042701353, -20.27515232684288549, 11.49999999999998934 ) ) ;
#78844 = CARTESIAN_POINT ( 'NONE',  ( -30.50620355861343214, -23.47596700323886409, 11.43088626683780618 ) ) ;
#78845 = CARTESIAN_POINT ( 'NONE',  ( -17.55682386033230102, 9.526633247210019917, -1.500000000000002220 ) ) ;
#78846 = DIRECTION ( 'NONE',  ( 0.000000000000000000, 0.000000000000000000, -1.000000000000000000 ) ) ;
#78847 = CARTESIAN_POINT ( 'NONE',  ( 5.724939850241691275, 20.19279902153374096, 11.49999999999999645 ) ) ;
#78848 = EDGE_CURVE ( 'NONE', #52932, #21474, #18689, .T. ) ;
#78849 = CIRCLE ( 'NONE', #75662, 3.349999999999998757 ) ;
#78850 = FACE_OUTER_BOUND ( 'NONE', #87038, .T. ) ;
#78851 = DIRECTION ( 'NONE',  ( -0.5656310827093756766, 0.8246584009594636333, 1.161164194647626880E-16 ) ) ;
#78852 = CARTESIAN_POINT ( 'NONE',  ( 4.500060333422437608, -21.59917750860068963, -1.500000000000002220 ) ) ;
#78853 = CARTESIAN_POINT ( 'NONE',  ( -4.621320343559618848, 12.50000000000004974, 2.100000000000000089 ) ) ;
#78854 = VERTEX_POINT ( 'NONE', #87596 ) ;
#78855 = CARTESIAN_POINT ( 'NONE',  ( 22.02124265030973760, 6.143225279485574397, 16.20402280011862217 ) ) ;
#78856 = PLANE ( 'NONE',  #3915 ) ;
#78857 = CARTESIAN_POINT ( 'NONE',  ( -40.01839366089613748, -25.29500187561385260, 5.509688069775453556 ) ) ;
#78858 = EDGE_LOOP ( 'NONE', ( #38957, #39848, #89988, #35804, #89759, #81851, #35093, #95039, #67053, #51934, #68315, #70655 ) ) ;
#78859 = CARTESIAN_POINT ( 'NONE',  ( -92.92287095715005307, -23.47596703998600631, 11.44779298504227860 ) ) ;
#78860 = ORIENTED_EDGE ( 'NONE', *, *, #27030, .T. ) ;
#78861 = VERTEX_POINT ( 'NONE', #9965 ) ;
#78862 = LINE ( 'NONE', #63172, #46935 ) ;
#78863 = PLANE ( 'NONE',  #56801 ) ;
#78864 = CARTESIAN_POINT ( 'NONE',  ( -100.5228709571500616, -23.47596703998600631, 11.44779298504228215 ) ) ;
#78865 = CARTESIAN_POINT ( 'NONE',  ( -20.18818894172909140, 3.697778396234267184, -1.500000000000002220 ) ) ;
#78866 = EDGE_CURVE ( 'NONE', #11910, #74791, #95703, .T. ) ;
#78867 = ORIENTED_EDGE ( 'NONE', *, *, #64465, .T. ) ;
#78868 = CARTESIAN_POINT ( 'NONE',  ( -100.1362965613156319, -25.30290612096174030, 5.258114224706423201 ) ) ;
#78869 = CARTESIAN_POINT ( 'NONE',  ( -44.64704124524567419, -23.96119346886879597, -0.6495511937832129101 ) ) ;
#78870 = DIRECTION ( 'NONE',  ( 0.000000000000000000, 1.000000000000000000, 0.000000000000000000 ) ) ;
#78871 = CARTESIAN_POINT ( 'NONE',  ( -22.23078454666273274, -1.437644496696519170, 11.49999999999998934 ) ) ;
#78872 = VECTOR ( 'NONE', #42666, 1000.000000000000000 ) ;
#78873 = CARTESIAN_POINT ( 'NONE',  ( -55.52287095715007581, -24.63345952396254290, 9.038047939301506517 ) ) ;
#78874 = CARTESIAN_POINT ( 'NONE',  ( 16.36243866176394945, 0.000000000000000000, 0.000000000000000000 ) ) ;
#78875 = EDGE_CURVE ( 'NONE', #94218, #99569, #74421, .T. ) ;
#78876 = VERTEX_POINT ( 'NONE', #34808 ) ;
#78877 = DIRECTION ( 'NONE',  ( -0.000000000000000000, -0.000000000000000000, -1.000000000000000000 ) ) ;
#78878 = CARTESIAN_POINT ( 'NONE',  ( -124.6228709571499706, -24.33832256527049154, 0.1851278514138684494 ) ) ;
#78879 = CARTESIAN_POINT ( 'NONE',  ( 16.93201058511109380, 12.15574511561022852, 11.49999999999998934 ) ) ;
#78880 = ORIENTED_EDGE ( 'NONE', *, *, #19402, .T. ) ;
#78883 = ORIENTED_EDGE ( 'NONE', *, *, #20660, .F. ) ;
#78882 = EDGE_CURVE ( 'NONE', #12709, #77171, #72103, .T. ) ;
#78881 = DIRECTION ( 'NONE',  ( -0.000000000000000000, 1.000000000000000000, -0.000000000000000000 ) ) ;
#78884 = AXIS2_PLACEMENT_3D ( 'NONE', #69507, #61903, #54295 ) ;
#78885 = ORIENTED_EDGE ( 'NONE', *, *, #82572, .F. ) ;
#78886 = DIRECTION ( 'NONE',  ( 1.420947339892994047E-14, 0.000000000000000000, -1.000000000000000000 ) ) ;
#78887 = CARTESIAN_POINT ( 'NONE',  ( 20.99820426035194032, -0.1900765340283884497, -1.500000000000002220 ) ) ;
#78888 = VERTEX_POINT ( 'NONE', #96696 ) ;
#78889 = VECTOR ( 'NONE', #56217, 1000.000000000000000 ) ;
#78890 = CARTESIAN_POINT ( 'NONE',  ( -118.5228709571500758, -24.33927499327856125, 9.819080762295802955 ) ) ;
#78891 = DIRECTION ( 'NONE',  ( 0.000000000000000000, 0.9999999999976377785, 2.173523156925979128E-06 ) ) ;
#78892 = CARTESIAN_POINT ( 'NONE',  ( 6.190876379677949792, -3.316774720513832708, -27.38145114071290465 ) ) ;
#78893 = AXIS2_PLACEMENT_3D ( 'NONE', #86644, #406, #31357 ) ;
#78894 = CARTESIAN_POINT ( 'NONE',  ( -86.58836611889687163, -24.35071581493543391, 9.817618358456027039 ) ) ;
#78895 = CARTESIAN_POINT ( 'NONE',  ( -59.64909978345416164, -23.73766607897669445, -1.055555164236460675 ) ) ;
#78896 = CARTESIAN_POINT ( 'NONE',  ( -109.7567236225155511, -25.29789953159075466, 5.668539300329492825 ) ) ;
#78897 = CARTESIAN_POINT ( 'NONE',  ( -63.58953762381673869, -24.64898659630528499, 1.056161002820821704 ) ) ;
#78899 = EDGE_LOOP ( 'NONE', ( #51435, #44497, #32579, #86509 ) ) ;
#78898 = CARTESIAN_POINT ( 'NONE',  ( -21.98633505697190671, -3.258044352128648846, 11.49999999999999645 ) ) ;
#78900 = B_SPLINE_CURVE_WITH_KNOTS ( 'NONE', 3,
 ( #27001, #72682, #42741, #41231, #2675, #88404 ),
 .UNSPECIFIED., .F., .F.,
 ( 4, 2, 4 ),
 ( 1.570755371633816901E-05, 0.001396183895866086886, 0.002776660238015835579 ),
 .UNSPECIFIED. ) ;
#78901 = LINE ( 'NONE', #17516, #38897 ) ;
#78902 = CARTESIAN_POINT ( 'NONE',  ( -54.62287095715005592, -24.64898659630528854, 1.056161002820821038 ) ) ;
#78903 = EDGE_LOOP ( 'NONE', ( #19289, #85929, #70594, #37856 ) ) ;
#78904 = CARTESIAN_POINT ( 'NONE',  ( 14.05383982582471170, -17.77673030755399708, 11.49999999999998934 ) ) ;
#78905 = B_SPLINE_CURVE_WITH_KNOTS ( 'NONE', 3,
 ( #21657, #52631, #68854, #1351 ),
 .UNSPECIFIED., .F., .F.,
 ( 4, 4 ),
 ( 0.6409576921988818787, 0.6499641234709975235 ),
 .UNSPECIFIED. ) ;
#78906 = B_SPLINE_CURVE_WITH_KNOTS ( 'NONE', 3,
 ( #71800, #70294, #94621, #57085, #25102, #71295 ),
 .UNSPECIFIED., .F., .F.,
 ( 4, 2, 4 ),
 ( 6.384118695832212569E-06, 0.001386860460836989405, 0.002767336802978146663 ),
 .UNSPECIFIED. ) ;
#78907 = B_SPLINE_CURVE_WITH_KNOTS ( 'NONE', 3,
 ( #83666, #67459, #6048, #45127 ),
 .UNSPECIFIED., .F., .F.,
 ( 4, 4 ),
 ( 0.7110077132042242898, 0.7200141444763397125 ),
 .UNSPECIFIED. ) ;
#78908 = EDGE_CURVE ( 'NONE', #22695, #3935, #19946, .T. ) ;
#78910 = ORIENTED_EDGE ( 'NONE', *, *, #14033, .T. ) ;
#78909 = CARTESIAN_POINT ( 'NONE',  ( -17.66201745896767505, -5.965225279485572685, -23.06272557202527906 ) ) ;
#78911 = EDGE_LOOP ( 'NONE', ( #67424, #94220, #72439, #1383 ) ) ;
#78912 = CARTESIAN_POINT ( 'NONE',  ( -19.69812919673063689, -5.965225279485592225, -22.00173861453435720 ) ) ;
#78913 = ADVANCED_FACE ( 'NONE', ( #58153 ), #80977, .F. ) ;
#78914 = CARTESIAN_POINT ( 'NONE',  ( 20.11291949428234105, -1.170665973999911902, -1.500000000000002220 ) ) ;
#78915 = CARTESIAN_POINT ( 'NONE',  ( -8.978253834636468866, -5.876774720514426953, 18.51871304725684553 ) ) ;
#78916 = ORIENTED_EDGE ( 'NONE', *, *, #11038, .T. ) ;
#78917 = PLANE ( 'NONE',  #6595 ) ;
#78918 = CARTESIAN_POINT ( 'NONE',  ( 21.53444271425275858, 6.169869319618734416, -1.500000000000002220 ) ) ;
#78919 = ORIENTED_EDGE ( 'NONE', *, *, #32947, .F. ) ;
#78920 = ORIENTED_EDGE ( 'NONE', *, *, #66367, .T. ) ;
#78921 = DIRECTION ( 'NONE',  ( -0.000000000000000000, 1.000000000000000000, -0.000000000000000000 ) ) ;
#78922 = CARTESIAN_POINT ( 'NONE',  ( -94.54933745284346003, -24.35071581493543036, 9.817618358456030592 ) ) ;
#78923 = DIRECTION ( 'NONE',  ( 0.000000000000000000, 0.000000000000000000, 1.000000000000000000 ) ) ;
#78924 = CIRCLE ( 'NONE', #25476, 3.060000000000000053 ) ;
#78925 = CARTESIAN_POINT ( 'NONE',  ( -124.5228709571500190, -24.66019654487200441, 8.947790411086112172 ) ) ;
#78926 = CYLINDRICAL_SURFACE ( 'NONE', #55272, 0.8160000000000007248 ) ;
#78927 = CARTESIAN_POINT ( 'NONE',  ( -15.85469643196389278, -11.46343829903102396, 11.49999999999998934 ) ) ;
#78928 = DIRECTION ( 'NONE',  ( 3.773278334444167608E-23, -1.000000000000000000, 0.000000000000000000 ) ) ;
#78929 = EDGE_LOOP ( 'NONE', ( #86712, #93603, #93610, #57326 ) ) ;
#78930 = CARTESIAN_POINT ( 'NONE',  ( -5.607854029519995898, -20.77141283803394955, -1.500000000000002220 ) ) ;
#78931 = AXIS2_PLACEMENT_3D ( 'NONE', #80683, #58361, #26401 ) ;
#78932 = CARTESIAN_POINT ( 'NONE',  ( -62.52287095715003318, -24.66019654487199730, 8.947790411086124607 ) ) ;
#78933 = CARTESIAN_POINT ( 'NONE',  ( 30.45304879119406039, -1.682774720514426114, -10.07140455160086390 ) ) ;
#78934 = CARTESIAN_POINT ( 'NONE',  ( -100.7575127936760566, -25.12643199199673560, 2.865359487688054152 ) ) ;
#78935 = CARTESIAN_POINT ( 'NONE',  ( -107.5562042904834072, -23.47596703998600631, 11.44779298504227683 ) ) ;
#78936 = CARTESIAN_POINT ( 'NONE',  ( -3.987988226355533072, 22.59150145119509290, -1.500000000000002220 ) ) ;
#78937 = B_SPLINE_CURVE_WITH_KNOTS ( 'NONE', 3,
 ( #84518, #38344, #69298, #100216 ),
 .UNSPECIFIED., .F., .F.,
 ( 4, 4 ),
 ( 6.656022119059916131E-09, 0.002563024260995911199 ),
 .UNSPECIFIED. ) ;
#78938 = CALENDAR_DATE ( 2026, 9, 10 ) ;
#78939 = CARTESIAN_POINT ( 'NONE',  ( -10.34999999999999254, -1.301042606982604926E-15, 4.499999999999999112 ) ) ;
#78940 = CARTESIAN_POINT ( 'NONE',  ( -2.373828433815573735, -5.876774720514410966, 19.48240003225459915 ) ) ;
#78941 = CARTESIAN_POINT ( 'NONE',  ( -1.723993941171178879, -19.98520929721398431, 11.49999999999999645 ) ) ;
#78942 = CARTESIAN_POINT ( 'NONE',  ( -79.79643364552497076, -25.26612395677430456, 4.606720527762783846 ) ) ;
#78943 = CARTESIAN_POINT ( 'NONE',  ( 8.160000000000000142, 0.000000000000000000, 0.000000000000000000 ) ) ;
#78944 = B_SPLINE_CURVE_WITH_KNOTS ( 'NONE', 3,
 ( #25543, #56010, #26551, #56511 ),
 .UNSPECIFIED., .F., .F.,
 ( 4, 4 ),
 ( 0.000000000000000000, 9.999999999998898659E-05 ),
 .UNSPECIFIED. ) ;
#78945 = CARTESIAN_POINT ( 'NONE',  ( 4.931982383686722926, -5.876774720514412742, 19.38944687450761961 ) ) ;
#78946 = DIRECTION ( 'NONE',  ( -3.773278334453079618E-23, 0.9999999999976377785, 2.173523156925978705E-06 ) ) ;
#78947 = CARTESIAN_POINT ( 'NONE',  ( -85.62287095715011276, -24.51163499207176244, 0.6490370598554221493 ) ) ;
#78948 = CARTESIAN_POINT ( 'NONE',  ( 6.829227106855087825, -20.66181959361685827, -1.500000000000002220 ) ) ;
#78949 = CARTESIAN_POINT ( 'NONE',  ( -27.25988310792305214, 0.3587747205144265483, 30.32664379231667695 ) ) ;
#78950 = CARTESIAN_POINT ( 'NONE',  ( 18.19143915067776263, 7.407926943018095400, -1.500000000000002220 ) ) ;
#78951 = VECTOR ( 'NONE', #87284, 1000.000000000000114 ) ;
#78952 = CARTESIAN_POINT ( 'NONE',  ( -61.59189125704997281, -25.08279362854488781, 7.371166896404004909 ) ) ;
#78953 = CARTESIAN_POINT ( 'NONE',  ( -109.3951644950792996, -25.31698007842469877, 4.495754895749054292 ) ) ;
#78954 = ITEM_DEFINED_TRANSFORMATION ( 'NONE', 'NONE', #65020,  #37391 ) ;
#78955 = CARTESIAN_POINT ( 'NONE',  ( -91.51495999646013502, -23.96169478059713498, 10.65365249895718058 ) ) ;
#78956 = CARTESIAN_POINT ( 'NONE',  ( 2.591664760199015927, -5.876774720514418071, 20.15921530338947321 ) ) ;
#78957 = CARTESIAN_POINT ( 'NONE',  ( 15.43701773751798001, -13.56989305476470875, 11.49999999999999645 ) ) ;
#78958 = CARTESIAN_POINT ( 'NONE',  ( 4.016587897052070311, -6.376774720514426065, 21.44459449800855921 ) ) ;
#78959 = VECTOR ( 'NONE', #29336, 1000.000000000000114 ) ;
#78960 = CARTESIAN_POINT ( 'NONE',  ( 33.74607884027702909, -5.965225279485572685, -4.999864028243830916 ) ) ;
#78961 = CARTESIAN_POINT ( 'NONE',  ( -3.174168706971715270, 22.36591850054903929, 11.49999999999999645 ) ) ;
#78962 = ORIENTED_EDGE ( 'NONE', *, *, #43698, .F. ) ;
#78963 = CARTESIAN_POINT ( 'NONE',  ( -46.62287095715004170, -24.51283580621364067, 0.6167428607019801445 ) ) ;
#78964 = CARTESIAN_POINT ( 'NONE',  ( -60.52287095715006160, -24.99132157543083821, 2.256160258750667502 ) ) ;
#78966 = EDGE_CURVE ( 'NONE', #50183, #55194, #81484, .T. ) ;
#78965 = CARTESIAN_POINT ( 'NONE',  ( -125.5887522299914139, -25.00182538069147498, 7.747789668545045139 ) ) ;
#78967 = CARTESIAN_POINT ( 'NONE',  ( -62.62287095715004881, -23.48783264082478794, -1.443836473390068820 ) ) ;
#78968 = VECTOR ( 'NONE', #99378, 1000.000000000000000 ) ;
#78969 = EDGE_CURVE ( 'NONE', #55307, #54376, #97776, .T. ) ;
#78970 = DIRECTION ( 'NONE',  ( -1.000000000000000000, -0.000000000000000000, -0.000000000000000000 ) ) ;
#78971 = EDGE_CURVE ( 'NONE', #89924, #85031, #5408, .T. ) ;
#78972 = CARTESIAN_POINT ( 'NONE',  ( 9.450000000000002842, -2.000000000000001332, 24.00000000000000000 ) ) ;
#78973 = EDGE_CURVE ( 'NONE', #50260, #56810, #25514, .T. ) ;
#78974 = ORIENTED_EDGE ( 'NONE', *, *, #46423, .F. ) ;
#78975 = CARTESIAN_POINT ( 'NONE',  ( -79.64180909446726275, -25.31596281824522165, 5.241605647354496966 ) ) ;
#78976 = CARTESIAN_POINT ( 'NONE',  ( 22.79674358141071977, 1.614764915196592598, 11.49999999999998934 ) ) ;
#78977 = CARTESIAN_POINT ( 'NONE',  ( 4.281720980632043094, -5.876774720514408301, 18.71132571341777151 ) ) ;
#78978 = CARTESIAN_POINT ( 'NONE',  ( -96.54562372648371138, -24.65952944569305316, 1.056160979905706121 ) ) ;
#78979 = CARTESIAN_POINT ( 'NONE',  ( -63.59779687502174994, -23.96169478059713143, 10.65365249895718236 ) ) ;
#78980 = CARTESIAN_POINT ( 'NONE',  ( 16.82713599508461400, -14.87465808564757808, 11.49999999999999645 ) ) ;
#78981 = ORIENTED_EDGE ( 'NONE', *, *, #47135, .F. ) ;
#78982 = CARTESIAN_POINT ( 'NONE',  ( -70.62287095715002749, -24.83620972994591369, 8.398175272781363887 ) ) ;
#78983 = CARTESIAN_POINT ( 'NONE',  ( 6.821863743248424150, 20.85434273413645911, 11.49999999999998934 ) ) ;
#78984 = CARTESIAN_POINT ( 'NONE',  ( -125.0508430453642319, -25.34741532608440906, 3.801652799235191615 ) ) ;
#78985 = CARTESIAN_POINT ( 'NONE',  ( -34.60965091549643802, -23.73791477778911485, 11.05961554403171299 ) ) ;
#78986 = CARTESIAN_POINT ( 'NONE',  ( -121.5228709571500616, -23.47596703998600631, 11.44779298504227860 ) ) ;
#78987 = ORIENTED_EDGE ( 'NONE', *, *, #16772, .F. ) ;
#78988 = ADVANCED_FACE ( 'NONE', ( #40242 ), #25001, .T. ) ;
#78989 = DIRECTION ( 'NONE',  ( -1.226388327005079762E-16, 0.000000000000000000, 1.000000000000000000 ) ) ;
#78990 = CARTESIAN_POINT ( 'NONE',  ( 31.13513474936814163, -4.540774720514427543, 3.331262582247520143 ) ) ;
#78991 = VERTEX_POINT ( 'NONE', #78781 ) ;
#78992 = CARTESIAN_POINT ( 'NONE',  ( -15.03541999946025243, -13.88573836563254460, 11.49999999999998934 ) ) ;
#78993 =( BOUNDED_CURVE ( )  B_SPLINE_CURVE ( 3, ( #26284, #89680, #58732, #65375 ),
 .UNSPECIFIED., .F., .F. ) 
 B_SPLINE_CURVE_WITH_KNOTS ( ( 4, 4 ),
 ( 1.570796326794896558, 1.674609638881183304 ),
 .UNSPECIFIED. ) 
 CURVE ( )  GEOMETRIC_REPRESENTATION_ITEM ( )  RATIONAL_B_SPLINE_CURVE ( ( 1.000000000000000000, 0.9991021013140741758, 0.9991021013140741758, 1.000000000000000000 ) ) 
 REPRESENTATION_ITEM ( '' )  );
#78994 = VERTEX_POINT ( 'NONE', #77774 ) ;
#78995 = VERTEX_POINT ( 'NONE', #55983 ) ;
#78996 = ORIENTED_EDGE ( 'NONE', *, *, #30315, .F. ) ;
#78997 = VERTEX_POINT ( 'NONE', #23486 ) ;
#78998 = CARTESIAN_POINT ( 'NONE',  ( 15.98122378838116120, 16.67787885001082770, 11.49999999999998934 ) ) ;
#78999 = CARTESIAN_POINT ( 'NONE',  ( -39.43364804524359357, -25.30977039686255026, 4.487062071701387822 ) ) ;
#79000 = CARTESIAN_POINT ( 'NONE',  ( -19.38859340154505873, -6.080128201517944753, -1.500000000000002220 ) ) ;
#79001 = ORIENTED_EDGE ( 'NONE', *, *, #54479, .F. ) ;
#79002 = AXIS2_PLACEMENT_3D ( 'NONE', #18635, #34377, #17645 ) ;
#79003 = CARTESIAN_POINT ( 'NONE',  ( -101.7776484685884100, -25.27307239909451653, 3.986250617436227550 ) ) ;
#79004 = DIRECTION ( 'NONE',  ( -3.773278334453079618E-23, 0.9999999999976377785, 2.173523156925979975E-06 ) ) ;
#79005 = CARTESIAN_POINT ( 'NONE',  ( -93.62287095715005592, -24.64965695001468404, 8.947790433994180503 ) ) ;
#79006 = CARTESIAN_POINT ( 'NONE',  ( 4.372949846226492632, -5.876774720514405637, 18.80635842184136308 ) ) ;
#79008 = VERTEX_POINT ( 'NONE', #40738 ) ;
#79007 = CARTESIAN_POINT ( 'NONE',  ( 7.367719877546908158, -20.20905560389912026, 11.49999999999999645 ) ) ;
#79009 = CARTESIAN_POINT ( 'NONE',  ( -75.54717685357564960, -24.40034930558991277, 0.3402023900116102895 ) ) ;
#79010 = CARTESIAN_POINT ( 'NONE',  ( -112.5562042904834072, -24.64898659630529210, 1.056161002820830142 ) ) ;
#79011 = EDGE_LOOP ( 'NONE', ( #34075, #34363, #92264, #74818 ) ) ;
#79012 = VECTOR ( 'NONE', #17809, 1000.000000000000114 ) ;
#79013 = CARTESIAN_POINT ( 'NONE',  ( -5.954758479537505700, 19.85987847461844424, 11.49999999999998934 ) ) ;
#79014 = VERTEX_POINT ( 'NONE', #54467 ) ;
#79016 = ORIENTED_EDGE ( 'NONE', *, *, #11412, .T. ) ;
#79015 = CARTESIAN_POINT ( 'NONE',  ( -125.5540159630755284, -25.00158670708911046, 2.256160236439218369 ) ) ;
#79017 = B_SPLINE_SURFACE_WITH_KNOTS ( 'NONE', 3, 3, ( 
 ( #28730, #97735, #65328, #66314 ),
 ( #43464, #74886, #97241, #11999 ),
 ( #82505, #57694, #72917, #19607 ),
 ( #34847, #74401, #65816, #81020 ),
 ( #50081, #3415, #11008, #96248 ),
 ( #42968, #11499, #51572, #27732 ),
 ( #19109, #26732, #88639, #81525 ),
 ( #43952, #96740, #5389, #42478 ),
 ( #12499, #90127, #34350, #20605 ),
 ( #35841, #4895, #18608, #58192 ) ),
 .UNSPECIFIED., .F., .F., .F.,
 ( 4, 3, 3, 4 ),
 ( 4, 4 ),
 ( 0.0004766839783816634356, 0.1491231665100169745, 0.2234464077758346323, 0.2977696490416522623 ),
 ( 0.2495241339546893922, 0.2506855492118910123 ),
 .UNSPECIFIED. ) ;
#79018 = CARTESIAN_POINT ( 'NONE',  ( -75.62287095715004170, -24.91570333823099759, 8.075032458375554612 ) ) ;
#79019 = PLANE ( 'NONE',  #29197 ) ;
#79020 = ORIENTED_EDGE ( 'NONE', *, *, #30701, .T. ) ;
#79021 = ORIENTED_EDGE ( 'NONE', *, *, #75310, .F. ) ;
#79022 = CARTESIAN_POINT ( 'NONE',  ( 9.402885806365684829, -5.965225279485572685, 29.04108526060719342 ) ) ;
#79023 = CARTESIAN_POINT ( 'NONE',  ( -42.57642875886570977, -24.66019654487198665, 8.947790411086131712 ) ) ;
#79024 = CARTESIAN_POINT ( 'NONE',  ( -27.89246614958421944, -24.63140169414405278, 1.634486445453936954 ) ) ;
#79026 = ORIENTED_EDGE ( 'NONE', *, *, #46736, .T. ) ;
#79025 = CARTESIAN_POINT ( 'NONE',  ( -12.30081598482267680, 18.28176383447183895, 11.49999999999999645 ) ) ;
#79027 = CARTESIAN_POINT ( 'NONE',  ( -103.6358262473195708, -23.48783264082477018, -1.443836473390091246 ) ) ;
#79028 = CARTESIAN_POINT ( 'NONE',  ( 7.090404290683943067, 21.45231405096426514, 11.49999999999998934 ) ) ;
#79029 = ADVANCED_FACE ( 'NONE', ( #24003 ), #48865, .F. ) ;
#79030 = CIRCLE ( 'NONE', #62839, 15.00000000000000178 ) ;
#79031 = CARTESIAN_POINT ( 'NONE',  ( 12.86141378215833342, 16.59024694808438127, 11.49999999999998934 ) ) ;
#79033 = ORIENTED_EDGE ( 'NONE', *, *, #85996, .T. ) ;
#79032 = CARTESIAN_POINT ( 'NONE',  ( -70.62287095715011276, -24.82558206586143257, 1.605769216559449708 ) ) ;
#79034 = ORIENTED_EDGE ( 'NONE', *, *, #78044, .F. ) ;
#79035 = CARTESIAN_POINT ( 'NONE',  ( 282.9764569301858046, 6.376774720514426953, 20.79159422840526616 ) ) ;
#79036 = ADVANCED_FACE ( 'NONE', ( #87409 ), #1181, .T. ) ;
#79037 = VECTOR ( 'NONE', #50949, 1000.000000000000114 ) ;
#79038 = EDGE_CURVE ( 'NONE', #58867, #32620, #51411, .T. ) ;
#79039 = CARTESIAN_POINT ( 'NONE',  ( 8.971512145086506962, -0.9738200612200849093, -3.736985260579222867 ) ) ;
#79040 = ORIENTED_EDGE ( 'NONE', *, *, #83781, .T. ) ;
#79041 = CARTESIAN_POINT ( 'NONE',  ( 12.34367313097222763, -17.18290682204727915, -1.500000000000002220 ) ) ;
#79042 = CARTESIAN_POINT ( 'NONE',  ( -10.59832330691884295, 5.965225279485572685, -27.05373799718300987 ) ) ;
#79043 = CARTESIAN_POINT ( 'NONE',  ( -61.66078443741151460, -25.31249728293746770, 5.276660823416809087 ) ) ;
#79044 = CARTESIAN_POINT ( 'NONE',  ( -104.6228709571500559, -24.64965695001468404, 8.947790433994178727 ) ) ;
#79045 = VECTOR ( 'NONE', #8677, 1000.000000000000000 ) ;
#79046 = CARTESIAN_POINT ( 'NONE',  ( -125.6228709571499706, -24.91544648472619983, 1.928969306349219259 ) ) ;
#79047 = CARTESIAN_POINT ( 'NONE',  ( 32.50838937279093699, 1.477225279485574028, -10.74666623472941573 ) ) ;
#79048 = CARTESIAN_POINT ( 'NONE',  ( 22.02009960291501045, 3.200778107580485532, -1.500000000000002220 ) ) ;
#79049 = B_SPLINE_CURVE_WITH_KNOTS ( 'NONE', 3,
 ( #73732, #35181, #94191, #86086, #93190, #25182, #62777, #32805, #55660, #86586, #77954, #23676, #24183, #2365 ),
 .UNSPECIFIED., .F., .F.,
 ( 4, 2, 2, 2, 2, 2, 4 ),
 ( 0.000000000000000000, 0.0002304994410172846522, 0.0004609988820345693045, 0.0009219977640691386089, 0.001382996646103707913, 0.001613496087120987795, 0.001843995528138267460 ),
 .UNSPECIFIED. ) ;
#79050 = CARTESIAN_POINT ( 'NONE',  ( -114.5904446279929232, -24.15543982623908192, -0.2315651400026444429 ) ) ;
#79051 = VERTEX_POINT ( 'NONE', #85402 ) ;
#79052 = CARTESIAN_POINT ( 'NONE',  ( -5.544977400725785266, -6.376774720514411854, 19.92818918856636401 ) ) ;
#79053 = CARTESIAN_POINT ( 'NONE',  ( -37.53883053087279364, -24.34968618360933590, 0.1864209137778856384 ) ) ;
#79054 = CARTESIAN_POINT ( 'NONE',  ( 0.1334620785917004226, -8.769264156269324317, 8.401340300369719094E-17 ) ) ;
#79055 = CARTESIAN_POINT ( 'NONE',  ( -41.72911611951712985, -25.22311787329266153, 3.586264385156655354 ) ) ;
#79056 = CARTESIAN_POINT ( 'NONE',  ( -7.160000000000000142, -10.77121780415746599, 1.154761385154455366 ) ) ;
#79057 = CARTESIAN_POINT ( 'NONE',  ( 6.171429453590791425, 18.48145409631445446, 11.49999999999998934 ) ) ;
#79058 = CARTESIAN_POINT ( 'NONE',  ( 19.34736296927903254, -9.154118057783460216, -1.500000000000002220 ) ) ;
#79059 = CARTESIAN_POINT ( 'NONE',  ( -85.52287095715009002, -23.84081130425357742, 10.88220057483159842 ) ) ;
#79060 = CARTESIAN_POINT ( 'NONE',  ( -60.57606894313024526, -25.00182538069856619, 7.747789668514392325 ) ) ;
#79061 = CARTESIAN_POINT ( 'NONE',  ( -78.52287095715004739, -23.48783264082476308, -1.443836473390091468 ) ) ;
#79062 = CARTESIAN_POINT ( 'NONE',  ( -100.7282901814618583, -25.18440018975361028, 3.329830012351928215 ) ) ;
#79063 = B_SPLINE_CURVE_WITH_KNOTS ( 'NONE', 3,
 ( #31501, #9166, #18287, #54857, #1572, #10676 ),
 .UNSPECIFIED., .F., .F.,
 ( 4, 2, 4 ),
 ( 1.570887131794333942E-05, 0.001396322306279758904, 0.002776935741241574537 ),
 .UNSPECIFIED. ) ;
#79064 = CARTESIAN_POINT ( 'NONE',  ( -22.19569011343799048, 5.130922947863589378, -1.500000000000002220 ) ) ;
#79065 = CARTESIAN_POINT ( 'NONE',  ( -103.6228709571500701, -23.48783264082478794, -1.443836473390062158 ) ) ;
#79066 = CARTESIAN_POINT ( 'NONE',  ( -80.52287095715007581, -24.51163499207174823, 0.6490370598554294768 ) ) ;
#79067 = CARTESIAN_POINT ( 'NONE',  ( 4.164567180745167185, 19.39263604865329071, 11.49999999999999645 ) ) ;
#79068 = CARTESIAN_POINT ( 'NONE',  ( -123.5895113708369593, -24.35071581493544812, 9.817618358456018157 ) ) ;
#79069 = CARTESIAN_POINT ( 'NONE',  ( 8.097539468418187170, -0.7382521156407163554, 3.736985260579222867 ) ) ;
#79070 = DIRECTION ( 'NONE',  ( 3.496357139254347770E-15, -0.9940716917543757081, -0.1087265912856345967 ) ) ;
#79071 = VERTEX_POINT ( 'NONE', #56488 ) ;
#79072 = CARTESIAN_POINT ( 'NONE',  ( 14.52511747680497933, -6.475225279485573360, -27.86035006098926559 ) ) ;
#79073 = CARTESIAN_POINT ( 'NONE',  ( -6.033988668995577065, -6.376774720514413630, 19.86422795159478483 ) ) ;
#79074 = CARTESIAN_POINT ( 'NONE',  ( -51.04701396381788925, -25.10935790734607664, 2.986906079344115561 ) ) ;
#79075 = CARTESIAN_POINT ( 'NONE',  ( -21.36891742734480104, 3.643610035731704055, -1.500000000000002220 ) ) ;
#79076 = DIRECTION ( 'NONE',  ( 0.000000000000000000, 0.9999999999976377785, 2.173523156925979128E-06 ) ) ;
#79077 = CARTESIAN_POINT ( 'NONE',  ( -8.858824863812619910, -17.32749669425128047, -1.500000000000002220 ) ) ;
#79078 = DIRECTION ( 'NONE',  ( 0.000000000000000000, 1.000000000000000000, 0.000000000000000000 ) ) ;
#79079 = EDGE_CURVE ( 'NONE', #19180, #99338, #6658, .T. ) ;
#79080 = ORIENTED_EDGE ( 'NONE', *, *, #90013, .F. ) ;
#79081 = CARTESIAN_POINT ( 'NONE',  ( -7.038884989605349141, -19.10714869031923513, 11.49999999999999645 ) ) ;
#79082 = CARTESIAN_POINT ( 'NONE',  ( -99.12380231474227799, -25.27434709648489886, 4.001575133896465353 ) ) ;
#79083 = CARTESIAN_POINT ( 'NONE',  ( 27.53860345374808105, -5.356774720496559894, -0.3523920347288979071 ) ) ;
#79084 = ORIENTED_EDGE ( 'NONE', *, *, #53363, .T. ) ;
#79085 = CARTESIAN_POINT ( 'NONE',  ( -78.94547585321313932, -25.25799298595097042, 6.082296582953498287 ) ) ;
#79086 = CARTESIAN_POINT ( 'NONE',  ( 33.29716795723528833, 4.396921096972350007, -11.57973373708315989 ) ) ;
#79087 = CARTESIAN_POINT ( 'NONE',  ( -39.14714599385568761, -25.27985388593766203, 4.777938703530348441 ) ) ;
#79088 = ADVANCED_FACE ( 'NONE', ( #32622 ), #17401, .F. ) ;
#79089 = DIRECTION ( 'NONE',  ( -3.773278334453080206E-23, 0.9999999999976377785, 2.173523156925979975E-06 ) ) ;
#79090 = CARTESIAN_POINT ( 'NONE',  ( -7.160000000000000142, 10.80195425911416507, -0.9450485415980990345 ) ) ;
#79091 = CARTESIAN_POINT ( 'NONE',  ( 19.93115673323400117, -2.579441489355707606, 11.49999999999998934 ) ) ;
#79092 = FACE_OUTER_BOUND ( 'NONE', #95604, .T. ) ;
#79094 = ORIENTED_EDGE ( 'NONE', *, *, #23556, .F. ) ;
#79093 = EDGE_CURVE ( 'NONE', #16766, #43974, #71697, .T. ) ;
#79095 = PLANE ( 'NONE',  #4180 ) ;
#79096 = VECTOR ( 'NONE', #54007, 1000.000000000000114 ) ;
#79097 = EDGE_CURVE ( 'NONE', #35546, #40078, #33124, .T. ) ;
#79098 = CARTESIAN_POINT ( 'NONE',  ( -22.87025945403008365, 2.249016246415321163, 11.49999999999999645 ) ) ;
#79099 = CARTESIAN_POINT ( 'NONE',  ( 19.62911079104473444, -11.51699945595908758, -1.500000000000002220 ) ) ;
#79100 = VERTEX_POINT ( 'NONE', #19392 ) ;
#79101 = CARTESIAN_POINT ( 'NONE',  ( -30.47287095715007155, -24.04948693798736059, 10.44728643021711179 ) ) ;
#79102 = EDGE_CURVE ( 'NONE', #35820, #11836, #1817, .T. ) ;
#79103 = DIRECTION ( 'NONE',  ( 0.000000000000000000, 0.000000000000000000, 1.000000000000000000 ) ) ;
#79104 = CARTESIAN_POINT ( 'NONE',  ( -90.58935238007963164, -24.52300882791528380, 0.6510814631126311536 ) ) ;
#79105 = B_SPLINE_CURVE_WITH_KNOTS ( 'NONE', 3,
 ( #52479, #91030, #82417, #66229, #89046, #51481 ),
 .UNSPECIFIED., .F., .F.,
 ( 4, 2, 4 ),
 ( 0.000000000000000000, 0.001380901958385378570, 0.002761803916770757140 ),
 .UNSPECIFIED. ) ;
#79106 = EDGE_CURVE ( 'NONE', #50305, #8499, #61130, .T. ) ;
#79107 = CARTESIAN_POINT ( 'NONE',  ( -30.57287095715007652, -24.39156613236284343, 9.691265933976838554 ) ) ;
#79108 = AXIS2_PLACEMENT_3D ( 'NONE', #25360, #47713, #78628 ) ;
#79109 = CARTESIAN_POINT ( 'NONE',  ( -69.55395755889061604, -23.96169478059712787, 10.65365249895718414 ) ) ;
#79110 = DIRECTION ( 'NONE',  ( 0.000000000000000000, -0.9999999999976377785, -2.173523156925979975E-06 ) ) ;
#79111 = CARTESIAN_POINT ( 'NONE',  ( -122.5540053569840921, -24.51314013834316086, 0.6176544820404212821 ) ) ;
#79112 = DIRECTION ( 'NONE',  ( -3.773278334453080206E-23, 0.9999999999976377785, 2.173523156925979975E-06 ) ) ;
#79113 = ORIENTED_EDGE ( 'NONE', *, *, #18962, .T. ) ;
#79114 = AXIS2_PLACEMENT_3D ( 'NONE', #72367, #59506, #12310 ) ;
#79115 = CARTESIAN_POINT ( 'NONE',  ( -17.41452279269062586, 10.58001483151439004, 11.49999999999998934 ) ) ;
#79116 = VERTEX_POINT ( 'NONE', #2689 ) ;
#79117 = VERTEX_POINT ( 'NONE', #42755 ) ;
#79118 = EDGE_CURVE ( 'NONE', #76771, #20796, #69570, .T. ) ;
#79119 = CARTESIAN_POINT ( 'NONE',  ( 5.527175565732886042, -22.34193536506064603, 11.49999999999998934 ) ) ;
#79120 = DIRECTION ( 'NONE',  ( 1.000000000000000000, 0.000000000000000000, -0.000000000000000000 ) ) ;
#79121 = ORIENTED_EDGE ( 'NONE', *, *, #61127, .F. ) ;
#79122 = CARTESIAN_POINT ( 'NONE',  ( -8.160000000000000142, -10.15233964170348457, 0.003711184059992174607 ) ) ;
#79123 = CARTESIAN_POINT ( 'NONE',  ( -118.6228709571500701, -24.65952944569305316, 1.056160979905706565 ) ) ;
#79124 = CARTESIAN_POINT ( 'NONE',  ( -95.56281893974220054, -23.48783264082477729, -1.443836473390088804 ) ) ;
#79125 = LINE ( 'NONE', #72037, #23704 ) ;
#79126 = VECTOR ( 'NONE', #7830, 1000.000000000000114 ) ;
#79128 = ORIENTED_EDGE ( 'NONE', *, *, #21402, .F. ) ;
#79127 = CARTESIAN_POINT ( 'NONE',  ( -17.77299844720193533, 11.79293508692305537, 11.49999999999999645 ) ) ;
#79129 = ORIENTED_EDGE ( 'NONE', *, *, #55862, .T. ) ;
#79130 = CARTESIAN_POINT ( 'NONE',  ( -17.21897301287555848, -14.04741862099043104, -1.500000000000002220 ) ) ;
#79131 = CARTESIAN_POINT ( 'NONE',  ( -14.43086120294938368, -14.79396848081076854, 11.49999999999998934 ) ) ;
#79132 = ORIENTED_EDGE ( 'NONE', *, *, #45299, .T. ) ;
#79133 = CARTESIAN_POINT ( 'NONE',  ( -5.877732331298974877, -5.876774720514411854, 19.69174559449349005 ) ) ;
#79134 = B_SPLINE_CURVE_WITH_KNOTS ( 'NONE', 3,
 ( #5258, #36216, #67676, #67180, #98596, #5756 ),
 .UNSPECIFIED., .F., .F.,
 ( 4, 2, 4 ),
 ( 1.570755371634415583E-05, 0.001396183895866091439, 0.002776660238015839048 ),
 .UNSPECIFIED. ) ;
#79135 = CARTESIAN_POINT ( 'NONE',  ( -95.55370924776086383, -24.15602025860896163, 10.28564288303535967 ) ) ;
#79136 = ORIENTED_EDGE ( 'NONE', *, *, #66629, .F. ) ;
#79137 = CARTESIAN_POINT ( 'NONE',  ( -28.62287095715004526, -24.50732993938405357, 8.947790418389013567 ) ) ;
#79138 = ORIENTED_EDGE ( 'NONE', *, *, #90702, .F. ) ;
#79139 = CARTESIAN_POINT ( 'NONE',  ( -91.52287095715006160, -29.50250786944525672, 11.44777988621623344 ) ) ;
#79140 = CARTESIAN_POINT ( 'NONE',  ( 16.07097863352054290, 13.35096362007907622, -1.500000000000002220 ) ) ;
#79142 = EDGE_CURVE ( 'NONE', #50701, #51171, #34635, .T. ) ;
#79141 = CARTESIAN_POINT ( 'NONE',  ( 9.711643268838683341, -19.58466107313252635, 11.49999999999999645 ) ) ;
#79143 = B_SPLINE_CURVE_WITH_KNOTS ( 'NONE', 3,
 ( #1335, #93156, #55629, #71345, #16035, #62746 ),
 .UNSPECIFIED., .F., .F.,
 ( 4, 2, 4 ),
 ( 1.570755371634190273E-05, 0.001396183895866087536, 0.002776660238015833410 ),
 .UNSPECIFIED. ) ;
#79144 = CARTESIAN_POINT ( 'NONE',  ( -27.47736343186643637, -24.89280002061735431, 7.597050255658339246 ) ) ;
#79145 = CARTESIAN_POINT ( 'NONE',  ( 15.29947330337542688, 3.316774720514426456, -27.16854002387010070 ) ) ;
#79146 = CARTESIAN_POINT ( 'NONE',  ( 5.133194422563156500, 21.89913303424002677, 11.49999999999998934 ) ) ;
#79147 = PLANE ( 'NONE',  #74098 ) ;
#79148 = EDGE_CURVE ( 'NONE', #86751, #82984, #35135, .T. ) ;
#79149 = CYLINDRICAL_SURFACE ( 'NONE', #92341, 1.500000000000000666 ) ;
#79150 = CARTESIAN_POINT ( 'NONE',  ( -59.55620429048340014, -23.47596703998600276, 11.44779298504227505 ) ) ;
#79151 = VERTEX_POINT ( 'NONE', #27522 ) ;
#79152 = ORIENTED_EDGE ( 'NONE', *, *, #46684, .T. ) ;
#79153 = ORIENTED_EDGE ( 'NONE', *, *, #5776, .F. ) ;
#79154 = CARTESIAN_POINT ( 'NONE',  ( -73.62287095715005592, -29.50250786944525672, 11.44777988621623699 ) ) ;
#79155 = ORIENTED_EDGE ( 'NONE', *, *, #80056, .F. ) ;
#79156 = CARTESIAN_POINT ( 'NONE',  ( 19.34736296927903254, -9.154118057783460216, -1.500000000000002220 ) ) ;
#79158 = EDGE_CURVE ( 'NONE', #26363, #30845, #96026, .T. ) ;
#79157 = CARTESIAN_POINT ( 'NONE',  ( -13.97600220251353953, -17.46790257487896270, 11.49999999999999645 ) ) ;
#79159 = ORIENTED_EDGE ( 'NONE', *, *, #9232, .F. ) ;
#79160 = FACE_BOUND ( 'NONE', #38463, .T. ) ;
#79161 = CARTESIAN_POINT ( 'NONE',  ( 20.56459456670464547, 4.482388377596099538, 11.49999999999998934 ) ) ;
#79162 = CARTESIAN_POINT ( 'NONE',  ( -30.49547139261239082, -24.38102096386331752, 9.702671485061733492 ) ) ;
#79163 = CARTESIAN_POINT ( 'NONE',  ( 4.608267332293128682, -19.41724391825443874, -1.500000000000002220 ) ) ;
#79164 = CARTESIAN_POINT ( 'NONE',  ( -117.6228709571500701, -23.73907113216991860, -1.053371485793220153 ) ) ;
#79165 = CARTESIAN_POINT ( 'NONE',  ( -61.55620429048339304, -23.48783264082478084, -1.443836473390068376 ) ) ;
#79166 = CARTESIAN_POINT ( 'NONE',  ( -22.07534667767119174, -0.2742745133902674826, -1.500000000000002220 ) ) ;
#79167 = ORIENTED_EDGE ( 'NONE', *, *, #95316, .T. ) ;
#79168 = CARTESIAN_POINT ( 'NONE',  ( -116.5208660521144424, -23.73766607897671577, -1.055555164236427812 ) ) ;
#79169 = EDGE_CURVE ( 'NONE', #92450, #78121, #89414, .T. ) ;
#79170 = CARTESIAN_POINT ( 'NONE',  ( -32.52287095715006160, -29.50250243563736774, 8.947779886222150481 ) ) ;
#79171 = CARTESIAN_POINT ( 'NONE',  ( -17.86878485216894319, -10.78119150571587781, 11.49999999999999645 ) ) ;
#79172 = VECTOR ( 'NONE', #52380, 1000.000000000000000 ) ;
#79173 = CARTESIAN_POINT ( 'NONE',  ( 29.57907552664497786, -3.519868637853082571, 29.21818156430573765 ) ) ;
#79174 = DIRECTION ( 'NONE',  ( 0.000000000000000000, 0.000000000000000000, 1.000000000000000000 ) ) ;
#79175 = CARTESIAN_POINT ( 'NONE',  ( -82.52287095715001897, -23.48783264083388289, -1.443836473375923690 ) ) ;
#79176 = B_SPLINE_CURVE_WITH_KNOTS ( 'NONE', 3,
 ( #100188, #6378, #77366, #53066 ),
 .UNSPECIFIED., .F., .F.,
 ( 4, 4 ),
 ( 0.000000000000000000, 9.999999999998900014E-05 ),
 .UNSPECIFIED. ) ;
#79177 = CARTESIAN_POINT ( 'NONE',  ( -21.15786647118399699, 2.672229404501205163, -1.500000000000002220 ) ) ;
#79178 = CARTESIAN_POINT ( 'NONE',  ( -81.52287095715007581, -24.33832256527047733, 0.1851278514138612330 ) ) ;
#79179 = DIRECTION ( 'NONE',  ( -3.773278334453079618E-23, 0.9999999999976377785, 2.173523156925979975E-06 ) ) ;
#79180 = CARTESIAN_POINT ( 'NONE',  ( -111.9545732713065291, -25.06732945298220372, 7.447791367849804445 ) ) ;
#79181 = FACE_OUTER_BOUND ( 'NONE', #57006, .T. ) ;
#79182 = CC_DESIGN_DATE_AND_TIME_ASSIGNMENT ( #100132, #61626, ( #34420 ) ) ;
#79183 = CARTESIAN_POINT ( 'NONE',  ( -20.69567741759225399, -9.018594580484563750, -1.500000000000002220 ) ) ;
#79184 = CARTESIAN_POINT ( 'NONE',  ( -51.52287095715005449, -24.66019654487199375, 8.947790411086119278 ) ) ;
#79185 = VERTEX_POINT ( 'NONE', #89911 ) ;
#79186 = B_SPLINE_CURVE_WITH_KNOTS ( 'NONE', 3,
 ( #14140, #7039, #37991, #92269, #46111, #88545, #3818, #54730, #38986, #69936, #70951, #55735, #23250, #1440 ),
 .UNSPECIFIED., .F., .F.,
 ( 4, 2, 2, 2, 2, 2, 4 ),
 ( 0.000000000000000000, 0.0001585405595148470887, 0.0003170811190296941775, 0.0006341622380593686225, 0.0009512433570890431759, 0.001109783916603885061, 0.001268324476118726837 ),
 .UNSPECIFIED. ) ;
#79187 = CARTESIAN_POINT ( 'NONE',  ( -78.94508464886243360, -25.27411879719900867, 5.881884475350567243 ) ) ;
#79188 = CARTESIAN_POINT ( 'NONE',  ( -31.59415779167720117, -24.15620529776627379, 10.23563542870661536 ) ) ;
#79189 = CARTESIAN_POINT ( 'NONE',  ( 0.7808950796103379943, -19.64173473864696717, 11.49999999999999645 ) ) ;
#79190 = LINE ( 'NONE', #9686, #37459 ) ;
#79191 = AXIS2_PLACEMENT_3D ( 'NONE', #69245, #39786, #15945 ) ;
#79192 = CARTESIAN_POINT ( 'NONE',  ( 14.79186724892429439, -4.799335165223686417, -27.67512533972776723 ) ) ;
#79193 = EDGE_LOOP ( 'NONE', ( #62712, #81279, #84613, #1395 ) ) ;
#79194 = CARTESIAN_POINT ( 'NONE',  ( -99.51646351673205970, -23.96119346886881374, -0.6495511937831867089 ) ) ;
#79195 = DIRECTION ( 'NONE',  ( -3.773278334453079030E-23, 0.9999999999976377785, 2.173523156925979128E-06 ) ) ;
#79196 = CARTESIAN_POINT ( 'NONE',  ( -105.5228709571500474, -23.85229601348996198, 10.88205029486208097 ) ) ;
#79197 = CARTESIAN_POINT ( 'NONE',  ( 29.73860345376319358, 14.82721238576592704, -4.021109907510727943 ) ) ;
#79198 = CARTESIAN_POINT ( 'NONE',  ( 19.74453702311487646, -0.1846442961375113490, 11.49999999999998934 ) ) ;
#79199 = B_SPLINE_CURVE_WITH_KNOTS ( 'NONE', 3,
 ( #87027, #63210, #94133, #17517 ),
 .UNSPECIFIED., .F., .F.,
 ( 4, 4 ),
 ( 0.000000000000000000, 9.999999999998897304E-05 ),
 .UNSPECIFIED. ) ;
#79200 = EDGE_LOOP ( 'NONE', ( #37979, #22315, #23380, #97305 ) ) ;
#79201 = CARTESIAN_POINT ( 'NONE',  ( -10.81679630089563915, -17.07601267366916886, 11.49999999999999645 ) ) ;
#79202 = CARTESIAN_POINT ( 'NONE',  ( -7.641025641025641413, -5.876774720514418071, 20.36458333333334636 ) ) ;
#79203 = AXIS2_PLACEMENT_3D ( 'NONE', #63248, #54134, #31275 ) ;
#79204 = ORIENTED_EDGE ( 'NONE', *, *, #87572, .F. ) ;
#79205 = CARTESIAN_POINT ( 'NONE',  ( -67.52287095715003318, -23.73934037231757088, 11.05740245334328797 ) ) ;
#79206 = PLANE ( 'NONE',  #89597 ) ;
#79207 = CARTESIAN_POINT ( 'NONE',  ( -51.51908035862399515, -25.26093919477311900, 6.045684827221686319 ) ) ;
#79208 = CARTESIAN_POINT ( 'NONE',  ( -125.5228709571500616, -29.50250243563736774, 8.947779886222132717 ) ) ;
#79209 = DIRECTION ( 'NONE',  ( -0.000000000000000000, 1.000000000000000000, -0.000000000000000000 ) ) ;
#79210 = CARTESIAN_POINT ( 'NONE',  ( -96.52287095715009002, -23.73907113216990084, -1.053371485793247686 ) ) ;
#79212 = EDGE_CURVE ( 'NONE', #51268, #803, #23526, .T. ) ;
#79211 = CARTESIAN_POINT ( 'NONE',  ( 5.980626343040887249, -19.09133569553460319, -1.500000000000002220 ) ) ;
#79213 = CARTESIAN_POINT ( 'NONE',  ( -99.38436720317001516, -25.10935138625626450, 3.296897716455177818 ) ) ;
#79214 = CARTESIAN_POINT ( 'NONE',  ( -116.5914120462304737, -23.96169478059714208, 10.65365249895717348 ) ) ;
#79215 = ORIENTED_EDGE ( 'NONE', *, *, #71662, .F. ) ;
#79216 = CARTESIAN_POINT ( 'NONE',  ( 0.000000000000000000, -4.132774720514426292, 0.000000000000000000 ) ) ;
#79217 = EDGE_CURVE ( 'NONE', #1547, #57623, #81798, .T. ) ;
#79218 = DIRECTION ( 'NONE',  ( 1.000000000000000000, -7.960204194457801640E-17, 0.000000000000000000 ) ) ;
#79219 = CARTESIAN_POINT ( 'NONE',  ( 1.949999999999999956, 0.1924999999999999489, 0.1925000000000000044 ) ) ;
#79220 = EDGE_CURVE ( 'NONE', #55689, #13751, #88421, .T. ) ;
#79221 = CARTESIAN_POINT ( 'NONE',  ( -0.02075734969026423599, -3.316774720514426456, -28.03397719988137382 ) ) ;
#79222 = CARTESIAN_POINT ( 'NONE',  ( -83.63279703061509451, -24.15543982623906771, -0.2315651400026649265 ) ) ;
#79223 = CARTESIAN_POINT ( 'NONE',  ( -3.108787716482549701, -5.876774720514418071, 20.32624910079993086 ) ) ;
#79224 = CARTESIAN_POINT ( 'NONE',  ( -49.72423105612087113, -25.21524731596653623, 3.522669676481375411 ) ) ;
#79225 = EDGE_LOOP ( 'NONE', ( #47202, #41933, #80038, #8408 ) ) ;
#79226 = VECTOR ( 'NONE', #53168, 1000.000000000000000 ) ;
#79227 = CIRCLE ( 'NONE', #32304, 1.149999999999998135 ) ;
#79228 = CARTESIAN_POINT ( 'NONE',  ( 0.7445296356392017145, -20.29553345556499622, -1.500000000000002220 ) ) ;
#79229 = EDGE_CURVE ( 'NONE', #78754, #53473, #18401, .T. ) ;
#79230 = CARTESIAN_POINT ( 'NONE',  ( 31.68813401132594976, 4.191046033661508297, 29.35543347196376729 ) ) ;
#79231 = CARTESIAN_POINT ( 'NONE',  ( -34.62373370718334797, -24.65952944569304606, 1.056160979905694353 ) ) ;
#79232 = VECTOR ( 'NONE', #91122, 1000.000000000000000 ) ;
#79233 = CARTESIAN_POINT ( 'NONE',  ( -107.5228709571500900, -23.73934037231758154, 11.05740245334328442 ) ) ;
#79234 = EDGE_LOOP ( 'NONE', ( #66133, #67694, #3052, #51917 ) ) ;
#79235 = CARTESIAN_POINT ( 'NONE',  ( 0.9317375178030620209, -7.299023693294228288, -9.000000000000000000 ) ) ;
#79236 = CARTESIAN_POINT ( 'NONE',  ( -10.65520286329281596, -18.28862552182625123, 11.49999999999999645 ) ) ;
#79237 = AXIS2_PLACEMENT_3D ( 'NONE', #23027, #14432, #100144 ) ;
#79238 = CARTESIAN_POINT ( 'NONE',  ( 0.7503028313155074569, 22.12739137992853955, -1.500000000000002220 ) ) ;
#79239 = CARTESIAN_POINT ( 'NONE',  ( 13.18781518674367348, -15.76626393773247337, -1.500000000000002220 ) ) ;
#79240 = ORIENTED_EDGE ( 'NONE', *, *, #32737, .F. ) ;
#79241 = CARTESIAN_POINT ( 'NONE',  ( -24.55517127435777169, 5.965225279485592225, -15.44180958690142802 ) ) ;
#79242 = ORIENTED_EDGE ( 'NONE', *, *, #10773, .T. ) ;
#79243 = CARTESIAN_POINT ( 'NONE',  ( -54.55346411107571214, -23.96119346886879953, -0.6495511937832153526 ) ) ;
#79244 = CARTESIAN_POINT ( 'NONE',  ( -110.6228709571500133, -24.52323809116983355, 9.355190652339425483 ) ) ;
#79245 = EDGE_LOOP ( 'NONE', ( #2147, #75872, #43840, #39728, #91351 ) ) ;
#79246 = VERTEX_POINT ( 'NONE', #80301 ) ;
#79247 = AXIS2_PLACEMENT_3D ( 'NONE', #57041, #42812, #79349 ) ;
#79248 = EDGE_LOOP ( 'NONE', ( #81623, #14973, #94095, #72000 ) ) ;
#79249 = CARTESIAN_POINT ( 'NONE',  ( -31.62287095715005236, -23.47596703998600276, 11.44779298504227505 ) ) ;
#79250 = CARTESIAN_POINT ( 'NONE',  ( 7.155337544004596317, -5.876774720514417183, 20.64714842558261765 ) ) ;
#79251 = CARTESIAN_POINT ( 'NONE',  ( 5.400898774349120579, -5.876774720514417183, 20.36357656736558042 ) ) ;
#79252 = CARTESIAN_POINT ( 'NONE',  ( -13.01863806243235899, 16.06808769575019014, -1.500000000000002220 ) ) ;
#79253 = ADVANCED_FACE ( 'NONE', ( #10793 ), #73201, .F. ) ;
#79254 = CARTESIAN_POINT ( 'NONE',  ( 14.58690015069645263, 15.99052346098381250, 11.49999999999999645 ) ) ;
#79255 = VERTEX_POINT ( 'NONE', #3689 ) ;
#79256 = CARTESIAN_POINT ( 'NONE',  ( -98.93771941505393386, -25.28237778386645473, 5.756362269627500972 ) ) ;
#79257 = CARTESIAN_POINT ( 'NONE',  ( -111.5960075431523251, -25.22279775002481017, 3.583730144309231758 ) ) ;
#79258 = CARTESIAN_POINT ( 'NONE',  ( 11.21425909587273928, 19.38466839394011387, 11.49999999999998934 ) ) ;
#79259 = CARTESIAN_POINT ( 'NONE',  ( -66.62287095715005592, -23.47596703998600276, 11.44779298504227683 ) ) ;
#79260 = CARTESIAN_POINT ( 'NONE',  ( -120.6228709571500843, -24.51254535404255819, 9.355368623467654743 ) ) ;
#79262 = ORIENTED_EDGE ( 'NONE', *, *, #20090, .F. ) ;
#79261 = EDGE_CURVE ( 'NONE', #20357, #80236, #77985, .T. ) ;
#79263 = DIRECTION ( 'NONE',  ( 0.000000000000000000, 0.000000000000000000, -1.000000000000000000 ) ) ;
#79264 = CARTESIAN_POINT ( 'NONE',  ( -35.63363566931067083, -24.73531770709095667, 8.716586749053508498 ) ) ;
#79265 = EDGE_LOOP ( 'NONE', ( #72875, #17132, #90710, #7292 ) ) ;
#79266 = ORIENTED_EDGE ( 'NONE', *, *, #48085, .T. ) ;
#79267 = EDGE_CURVE ( 'NONE', #79731, #63566, #19626, .T. ) ;
#79268 = CARTESIAN_POINT ( 'NONE',  ( 11.62916340711181284, 0.3587747205144265483, 28.75961759920349792 ) ) ;
#79269 = B_SPLINE_CURVE_WITH_KNOTS ( 'NONE', 3,
 ( #33298, #79478, #43791, #2875, #82341, #35679 ),
 .UNSPECIFIED., .F., .F.,
 ( 4, 2, 4 ),
 ( 6.384118678607784034E-06, 0.001386860460828371732, 0.002767336802978135387 ),
 .UNSPECIFIED. ) ;
#79270 = ORIENTED_EDGE ( 'NONE', *, *, #70970, .T. ) ;
#79271 = AXIS2_PLACEMENT_3D ( 'NONE', #61501, #8207, #39146 ) ;
#79272 = EDGE_CURVE ( 'NONE', #95881, #87149, #12018, .T. ) ;
#79273 = FACE_OUTER_BOUND ( 'NONE', #26411, .T. ) ;
#79274 = CARTESIAN_POINT ( 'NONE',  ( 0.06830352742921809439, -21.21198074455918814, -1.500000000000002220 ) ) ;
#79275 = ORIENTED_EDGE ( 'NONE', *, *, #13338, .T. ) ;
#79276 = CARTESIAN_POINT ( 'NONE',  ( -50.52684846233325544, -24.92564183028979130, 1.928384488918255535 ) ) ;
#79277 = CARTESIAN_POINT ( 'NONE',  ( -11.04117723084791614, -18.81814233335528286, -1.500000000000002220 ) ) ;
#79278 = FACE_OUTER_BOUND ( 'NONE', #95367, .T. ) ;
#79279 = FACE_OUTER_BOUND ( 'NONE', #87627, .T. ) ;
#79280 = CARTESIAN_POINT ( 'NONE',  ( -55.62287095715004170, -24.99132157543083821, 2.256160258750667502 ) ) ;
#79281 = CARTESIAN_POINT ( 'NONE',  ( -1.606994170628035068, 21.82944698466814870, -1.500000000000002220 ) ) ;
#79282 = CARTESIAN_POINT ( 'NONE',  ( -30.57287095715005520, -25.22658899513668729, 6.410055712259026706 ) ) ;
#79283 = ORIENTED_EDGE ( 'NONE', *, *, #2836, .F. ) ;
#79284 = CARTESIAN_POINT ( 'NONE',  ( 25.13432252085998186, 4.913094919796972881, -10.17719671683694571 ) ) ;
#79285 = CARTESIAN_POINT ( 'NONE',  ( 7.749999999999998224, 25.69999999999999574, 2.100000000000000089 ) ) ;
#79286 = ORIENTED_EDGE ( 'NONE', *, *, #58949, .T. ) ;
#79287 = VERTEX_POINT ( 'NONE', #44978 ) ;
#79288 = B_SPLINE_CURVE_WITH_KNOTS ( 'NONE', 3,
 ( #57753, #58737, #90182, #66370, #34904, #65381 ),
 .UNSPECIFIED., .F., .F.,
 ( 4, 2, 4 ),
 ( 0.000000000000000000, 0.001380764517854768869, 0.002761529035709537738 ),
 .UNSPECIFIED. ) ;
#79289 = ORIENTED_EDGE ( 'NONE', *, *, #52750, .T. ) ;
#79290 = CARTESIAN_POINT ( 'NONE',  ( -69.52287095715006160, -29.50250243563736774, 8.947779886222143375 ) ) ;
#79291 = CARTESIAN_POINT ( 'NONE',  ( 282.9764569301858046, -4.540774720514427543, 20.79159422840526616 ) ) ;
#79292 = CARTESIAN_POINT ( 'NONE',  ( -21.21068194950259311, 0.7780057951688260642, -1.500000000000002220 ) ) ;
#79293 = CARTESIAN_POINT ( 'NONE',  ( -44.62287095715004881, -23.48783264082478084, -1.443836473390072150 ) ) ;
#79294 = CARTESIAN_POINT ( 'NONE',  ( -130.5728709571500588, -24.75991027412950274, 1.063373454495737391 ) ) ;
#79295 = EDGE_CURVE ( 'NONE', #20122, #15617, #27256, .T. ) ;
#79296 = CYLINDRICAL_SURFACE ( 'NONE', #4876, 129.7684398600581517 ) ;
#79297 = CYLINDRICAL_SURFACE ( 'NONE', #39499, 2.500000000000000444 ) ;
#79298 = EDGE_CURVE ( 'NONE', #16500, #90746, #85363, .T. ) ;
#79299 = CARTESIAN_POINT ( 'NONE',  ( 19.02374887324148389, -3.781047496429098764, -1.500000000000002220 ) ) ;
#79300 = CARTESIAN_POINT ( 'NONE',  ( -45.58195093673430165, -24.73486907724917572, 1.287355809206967017 ) ) ;
#79301 = ORIENTED_EDGE ( 'NONE', *, *, #99934, .T. ) ;
#79302 = CARTESIAN_POINT ( 'NONE',  ( -11.52932745282126703, -15.74164922852205173, 11.49999999999999645 ) ) ;
#79303 = CARTESIAN_POINT ( 'NONE',  ( -99.57255944844885676, -25.31502864763020355, 4.874549032268092219 ) ) ;
#79304 = AXIS2_PLACEMENT_3D ( 'NONE', #75607, #91348, #59921 ) ;
#79305 = LINE ( 'NONE', #17416, #38270 ) ;
#79306 = ORIENTED_EDGE ( 'NONE', *, *, #16129, .T. ) ;
#79307 = CARTESIAN_POINT ( 'NONE',  ( -93.62287095715001328, -24.33832256526969218, 0.1851278514119904517 ) ) ;
#79308 = EDGE_CURVE ( 'NONE', #94249, #67214, #28244, .T. ) ;
#79309 = CARTESIAN_POINT ( 'NONE',  ( -89.60221604899453496, -23.48783264082478084, -1.443836473390068154 ) ) ;
#79310 = AXIS2_PLACEMENT_3D ( 'NONE', #17494, #57578, #71793 ) ;
#79311 = EDGE_CURVE ( 'NONE', #54685, #60837, #78098, .T. ) ;
#79312 = LINE ( 'NONE', #50381, #79591 ) ;
#79313 = CARTESIAN_POINT ( 'NONE',  ( -81.52676753278062449, -25.03155964481168638, 7.119670603759651328 ) ) ;
#79314 = CARTESIAN_POINT ( 'NONE',  ( -19.15281226579456231, 4.489446101945751444, 11.49999999999998934 ) ) ;
#79315 = VECTOR ( 'NONE', #58178, 1000.000000000000114 ) ;
#79316 = ORIENTED_EDGE ( 'NONE', *, *, #60765, .T. ) ;
#79317 = VECTOR ( 'NONE', #21812, 1000.000000000000114 ) ;
#79318 = DIRECTION ( 'NONE',  ( -0.000000000000000000, -1.000000000000000000, -0.000000000000000000 ) ) ;
#79319 = CARTESIAN_POINT ( 'NONE',  ( 10.19088217375349892, 20.72639945755932800, -1.500000000000002220 ) ) ;
#79320 = VECTOR ( 'NONE', #35122, 1000.000000000000000 ) ;
#79321 = APPROVAL_DATE_TIME ( #32648, #28322 ) ;
#79322 = CARTESIAN_POINT ( 'NONE',  ( 3.448102555317568374, -5.876774720514423400, 21.39871091031772110 ) ) ;
#79323 = CARTESIAN_POINT ( 'NONE',  ( -90.52287095715001897, -24.82576562948886334, 8.398263436605496679 ) ) ;
#79324 = CARTESIAN_POINT ( 'NONE',  ( -109.6313485239119672, -25.13840250613601413, 2.992668966235024541 ) ) ;
#79325 = CARTESIAN_POINT ( 'NONE',  ( -97.63858573790135154, -23.48786465467241413, 11.44779295918254469 ) ) ;
#79326 = DIRECTION ( 'NONE',  ( 0.000000000000000000, 0.000000000000000000, 1.000000000000000000 ) ) ;
#79327 = CARTESIAN_POINT ( 'NONE',  ( 11.62916340711181284, -5.965225279485572685, 28.75961759920349792 ) ) ;
#79328 = PLANE ( 'NONE',  #82977 ) ;
#79329 = CARTESIAN_POINT ( 'NONE',  ( -99.60745734687597519, -25.31566092335526008, 4.898549720458867718 ) ) ;
#79331 = EDGE_CURVE ( 'NONE', #28943, #95426, #81603, .T. ) ;
#79330 = CARTESIAN_POINT ( 'NONE',  ( -8.676013072486071565, -17.92234406281952275, 11.49999999999998934 ) ) ;
#79332 = CARTESIAN_POINT ( 'NONE',  ( -126.6228709571500559, -29.50250243563736774, 8.947779886222132717 ) ) ;
#79333 = CARTESIAN_POINT ( 'NONE',  ( 19.84127317031322946, -0.4231496731191971561, -1.500000000000002220 ) ) ;
#79334 = ORIENTED_EDGE ( 'NONE', *, *, #20269, .F. ) ;
#79335 = PLANE ( 'NONE',  #47535 ) ;
#79336 = LINE ( 'NONE', #86455, #82429 ) ;
#79337 = CARTESIAN_POINT ( 'NONE',  ( -7.641025641025640525, -6.376774720514417183, 20.36458333333334281 ) ) ;
#79338 = CARTESIAN_POINT ( 'NONE',  ( -20.76960556195881225, -0.3855258213679747525, 11.49999999999999645 ) ) ;
#79339 = DIRECTION ( 'NONE',  ( -3.773278334444167608E-23, 1.000000000000000000, 0.000000000000000000 ) ) ;
#79340 = ADVANCED_FACE ( 'NONE', ( #4914 ), #34865, .F. ) ;
#79341 = CARTESIAN_POINT ( 'NONE',  ( -106.5572847460906729, -23.73766607897671221, -1.055555164236449572 ) ) ;
#79342 = CARTESIAN_POINT ( 'NONE',  ( 12.47407908559008760, -19.03963781694049473, 11.49999999999999645 ) ) ;
#79343 = VERTEX_POINT ( 'NONE', #3928 ) ;
#79344 = CARTESIAN_POINT ( 'NONE',  ( -69.49426968199877308, -24.65952944569304606, 1.056160979905704567 ) ) ;
#79345 = EDGE_CURVE ( 'NONE', #39568, #31671, #68420, .T. ) ;
#79346 = CARTESIAN_POINT ( 'NONE',  ( -100.5228709571500616, -25.00158670708909625, 2.256160236439166411 ) ) ;
#79347 = VERTEX_POINT ( 'NONE', #28746 ) ;
#79348 = CARTESIAN_POINT ( 'NONE',  ( -18.67835518149133378, -7.740158416121700746, 11.49999999999998934 ) ) ;
#79349 = DIRECTION ( 'NONE',  ( 0.000000000000000000, 0.000000000000000000, -1.000000000000000000 ) ) ;
#79350 = EDGE_CURVE ( 'NONE', #49218, #59202, #5407, .T. ) ;
#79351 = LINE ( 'NONE', #56541, #12337 ) ;
#79352 = EDGE_CURVE ( 'NONE', #87739, #93213, #65836, .T. ) ;
#79353 = ORIENTED_EDGE ( 'NONE', *, *, #35818, .F. ) ;
#79354 = CYLINDRICAL_SURFACE ( 'NONE', #48475, 1.325999999999969647 ) ;
#79355 = CARTESIAN_POINT ( 'NONE',  ( 13.91401389203221406, -6.376774720514426953, 158.0376437107427137 ) ) ;
#79356 = CARTESIAN_POINT ( 'NONE',  ( -16.75416981316412190, 10.96944243606782443, -1.500000000000002220 ) ) ;
#79357 = CARTESIAN_POINT ( 'NONE',  ( -41.05437879045549465, -25.05917046252012170, 7.488404917370821146 ) ) ;
#79358 = CARTESIAN_POINT ( 'NONE',  ( -16.25153318171239647, -13.25006309444557751, 11.49999999999999645 ) ) ;
#79359 = DIRECTION ( 'NONE',  ( -3.773278334453080206E-23, 0.9999999999976377785, 2.173523156925979975E-06 ) ) ;
#79360 = B_SPLINE_CURVE_WITH_KNOTS ( 'NONE', 3,
 ( #69637, #60036, #98568, #6722 ),
 .UNSPECIFIED., .F., .F.,
 ( 4, 4 ),
 ( 0.3507504623196067151, 0.3597568935917223043 ),
 .UNSPECIFIED. ) ;
#79361 = CYLINDRICAL_SURFACE ( 'NONE', #74055, 1.306876713926001798 ) ;
#79362 = CARTESIAN_POINT ( 'NONE',  ( 11.67614657018352453, 18.69773523334854914, -1.500000000000002220 ) ) ;
#79363 = AXIS2_PLACEMENT_3D ( 'NONE', #33064, #54400, #47289 ) ;
#79364 = DIRECTION ( 'NONE',  ( -1.000000000000000000, 0.000000000000000000, 0.000000000000000000 ) ) ;
#79365 = ORIENTED_EDGE ( 'NONE', *, *, #46571, .F. ) ;
#79366 = CARTESIAN_POINT ( 'NONE',  ( -53.52287095715006870, -24.64898659630367916, 1.056161002820821038 ) ) ;
#79367 = CARTESIAN_POINT ( 'NONE',  ( 27.53860345374771867, 1.477225279485574028, -9.482392034746242260 ) ) ;
#79368 = CARTESIAN_POINT ( 'NONE',  ( -72.56475442579929336, -23.48783264082477018, -1.443836473390095021 ) ) ;
#79369 = ORIENTED_EDGE ( 'NONE', *, *, #37308, .T. ) ;
#79370 = FACE_OUTER_BOUND ( 'NONE', #96537, .T. ) ;
#79371 = VERTEX_POINT ( 'NONE', #73925 ) ;
#79372 = VECTOR ( 'NONE', #11991, 1000.000000000000000 ) ;
#79373 = EDGE_LOOP ( 'NONE', ( #85991, #100010, #27847, #79535 ) ) ;
#79374 = DIRECTION ( 'NONE',  ( 1.000000000000000000, -7.960204194457801640E-17, 0.000000000000000000 ) ) ;
#79375 = CARTESIAN_POINT ( 'NONE',  ( -8.499999999999987566, 18.74999999999999645, 0.000000000000000000 ) ) ;
#79376 = FACE_OUTER_BOUND ( 'NONE', #35692, .T. ) ;
#79377 = CARTESIAN_POINT ( 'NONE',  ( -19.23287947355762384, -7.152392467615741545, -1.500000000000002220 ) ) ;
#79378 = ORIENTED_EDGE ( 'NONE', *, *, #45221, .F. ) ;
#79379 = CARTESIAN_POINT ( 'NONE',  ( -110.5562042904833930, -24.99156044556202971, 7.747789690856172307 ) ) ;
#79380 = VECTOR ( 'NONE', #40852, 1000.000000000000000 ) ;
#79381 = CARTESIAN_POINT ( 'NONE',  ( 0.000000000000000000, -5.876774720514426953, 0.000000000000000000 ) ) ;
#79382 = CARTESIAN_POINT ( 'NONE',  ( -46.62287095715004881, -23.47596703998600276, 11.44779298504227505 ) ) ;
#79383 = CARTESIAN_POINT ( 'NONE',  ( 13.23790625878087468, -17.95846084735695314, 11.49999999999998934 ) ) ;
#79384 = CARTESIAN_POINT ( 'NONE',  ( -71.30457154551150722, -25.25559839591754496, 6.209207386190694677 ) ) ;
#79386 = EDGE_CURVE ( 'NONE', #79408, #55323, #97154, .T. ) ;
#79385 = CARTESIAN_POINT ( 'NONE',  ( -1.363607173041644582, -5.876774720514419847, 20.50445910983877340 ) ) ;
#79387 = EDGE_LOOP ( 'NONE', ( #100222, #4150, #63689, #43209 ) ) ;
#79388 = DIRECTION ( 'NONE',  ( 0.000000000000000000, 0.000000000000000000, -1.000000000000000000 ) ) ;
#79389 = VECTOR ( 'NONE', #17860, 1000.000000000000000 ) ;
#79390 = DIRECTION ( 'NONE',  ( -0.000000000000000000, 1.000000000000000000, -0.000000000000000000 ) ) ;
#79391 = VECTOR ( 'NONE', #85220, 1000.000000000000000 ) ;
#79392 = CARTESIAN_POINT ( 'NONE',  ( -5.376107494350208960, -20.15860285114975525, -1.500000000000002220 ) ) ;
#79393 = ORIENTED_EDGE ( 'NONE', *, *, #66531, .T. ) ;
#79395 = ORIENTED_EDGE ( 'NONE', *, *, #70885, .F. ) ;
#79394 = CARTESIAN_POINT ( 'NONE',  ( -79.52287095715009002, -23.96177878511310055, 10.65340807706329862 ) ) ;
#79396 = ORIENTED_EDGE ( 'NONE', *, *, #50409, .F. ) ;
#79397 = CARTESIAN_POINT ( 'NONE',  ( -69.79804103094413392, -25.03149351086992525, 7.463049324080706093 ) ) ;
#79398 = CARTESIAN_POINT ( 'NONE',  ( 8.881738082190086203, 19.07353979602852689, -1.500000000000002220 ) ) ;
#79399 = ORIENTED_EDGE ( 'NONE', *, *, #90567, .T. ) ;
#79400 = CARTESIAN_POINT ( 'NONE',  ( 8.159999999999996589, 9.922339117699207733, -0.8680921884585347525 ) ) ;
#79401 = CARTESIAN_POINT ( 'NONE',  ( -114.6228709571500559, -29.50250786944525672, 11.44777988621622988 ) ) ;
#79402 = CARTESIAN_POINT ( 'NONE',  ( -120.5166134144556764, -24.92592662359561473, 8.075495903018000021 ) ) ;
#79403 = CARTESIAN_POINT ( 'NONE',  ( -86.63935476550661008, -23.73791477778911840, 11.05961554403170766 ) ) ;
#79404 = CARTESIAN_POINT ( 'NONE',  ( -59.49371803394627278, -24.51314013834316441, 0.6176544820404136216 ) ) ;
#79405 = CARTESIAN_POINT ( 'NONE',  ( -46.62287095715004881, -29.50248528299804818, 1.056150453629033370 ) ) ;
#79406 = CARTESIAN_POINT ( 'NONE',  ( -73.62287095715005592, -29.50248528299804818, 1.056150453629036701 ) ) ;
#79408 = VERTEX_POINT ( 'NONE', #52581 ) ;
#79407 = CARTESIAN_POINT ( 'NONE',  ( -21.91529987491217923, -3.391794311424265018, 11.49999999999999645 ) ) ;
#79409 = CARTESIAN_POINT ( 'NONE',  ( -109.5228709571500616, -23.47593901973090524, -1.443836447538996426 ) ) ;
#79410 = DIRECTION ( 'NONE',  ( -3.773278334453079618E-23, 0.9999999999976377785, 2.173523156925979975E-06 ) ) ;
#79411 = ORIENTED_EDGE ( 'NONE', *, *, #18664, .T. ) ;
#79412 = CARTESIAN_POINT ( 'NONE',  ( -0.4833002549469566644, -22.66139224067150337, -1.500000000000002220 ) ) ;
#79414 = ORIENTED_EDGE ( 'NONE', *, *, #7945, .T. ) ;
#79413 = CARTESIAN_POINT ( 'NONE',  ( 27.53860345374808105, 1.477225279485574028, 0.000000000000000000 ) ) ;
#79415 = ORIENTED_EDGE ( 'NONE', *, *, #96285, .F. ) ;
#79416 = FACE_OUTER_BOUND ( 'NONE', #32765, .T. ) ;
#79417 = EDGE_CURVE ( 'NONE', #74266, #90387, #55127, .T. ) ;
#79418 = CARTESIAN_POINT ( 'NONE',  ( 18.82035724208558491, -7.196742317222773799, -1.500000000000002220 ) ) ;
#79419 = CARTESIAN_POINT ( 'NONE',  ( 27.86270917940689174, 0.3587747205144265483, 29.49402280011862487 ) ) ;
#79420 = ORIENTED_EDGE ( 'NONE', *, *, #5096, .T. ) ;
#79421 = CARTESIAN_POINT ( 'NONE',  ( -130.5728709571500019, -24.56483619690598275, 0.5169519342574478982 ) ) ;
#79422 = CARTESIAN_POINT ( 'NONE',  ( 6.968497804723354783, -21.30229754059623559, -1.500000000000002220 ) ) ;
#79423 = B_SPLINE_CURVE_WITH_KNOTS ( 'NONE', 3,
 ( #33685, #87973, #80858, #3744 ),
 .UNSPECIFIED., .F., .F.,
 ( 4, 4 ),
 ( 0.2399572720920363500, 0.2489637033641517727 ),
 .UNSPECIFIED. ) ;
#79424 = ORIENTED_EDGE ( 'NONE', *, *, #55304, .T. ) ;
#79425 = ORIENTED_EDGE ( 'NONE', *, *, #5346, .F. ) ;
#79426 = CARTESIAN_POINT ( 'NONE',  ( -112.6245366205870795, -24.51419770103158413, 9.386484678747166299 ) ) ;
#79427 = CARTESIAN_POINT ( 'NONE',  ( -4.312370003044874167, -5.876774720514408301, 19.42522865122897358 ) ) ;
#79428 = CARTESIAN_POINT ( 'NONE',  ( -96.62287095715005592, -23.47596703998600631, 11.44779298504227860 ) ) ;
#79429 = EDGE_CURVE ( 'NONE', #62532, #39894, #58711, .T. ) ;
#79430 = EDGE_CURVE ( 'NONE', #97480, #97261, #53595, .T. ) ;
#79431 = CARTESIAN_POINT ( 'NONE',  ( 31.25756411700558601, 5.804570343751186634, -1.813502816810933949 ) ) ;
#79432 = EDGE_CURVE ( 'NONE', #44866, #56695, #93620, .T. ) ;
#79433 = CARTESIAN_POINT ( 'NONE',  ( -130.5728709571500019, -23.78062553189673167, -0.9709657327914282821 ) ) ;
#79434 = CARTESIAN_POINT ( 'NONE',  ( -18.58057592369839384, -6.135153870360039896, -1.500000000000002220 ) ) ;
#79435 = CARTESIAN_POINT ( 'NONE',  ( -59.62287095715004170, -24.65952944569304606, 1.056160979905694131 ) ) ;
#79437 = EDGE_CURVE ( 'NONE', #39077, #31334, #15006, .T. ) ;
#79436 = ORIENTED_EDGE ( 'NONE', *, *, #57614, .F. ) ;
#79438 = CARTESIAN_POINT ( 'NONE',  ( 5.543860000110784725, 20.76261553274053284, -1.500000000000002220 ) ) ;
#79439 = CARTESIAN_POINT ( 'NONE',  ( -102.6228709571500417, -23.48786465467241769, 11.44779295918253936 ) ) ;
#79440 = DIRECTION ( 'NONE',  ( -0.000000000000000000, 1.000000000000000000, -0.000000000000000000 ) ) ;
#79441 = LINE ( 'NONE', #25659, #14998 ) ;
#79442 = AXIS2_PLACEMENT_3D ( 'NONE', #7236, #69143, #68656 ) ;
#79443 = CARTESIAN_POINT ( 'NONE',  ( -77.62287095715007013, -24.66019654487199730, 8.947790411086128159 ) ) ;
#79444 = CARTESIAN_POINT ( 'NONE',  ( -14.16064136294604303, -18.02537036913223290, -1.500000000000002220 ) ) ;
#79445 = B_SPLINE_CURVE_WITH_KNOTS ( 'NONE', 3,
 ( #37234, #62075, #84894, #22479, #75283, #21983, #15375, #68185, #7773, #52463, #91504, #45845, #77269, #67701 ),
 .UNSPECIFIED., .F., .F.,
 ( 4, 2, 2, 2, 2, 2, 4 ),
 ( 0.000000000000000000, 0.0002247388865718425940, 0.0004494777731436851880, 0.0008989555462873846875, 0.001348433319431084241, 0.001573172206002952395, 0.001797911092574820549 ),
 .UNSPECIFIED. ) ;
#79446 = CALENDAR_DATE ( 2026, 9, 10 ) ;
#79447 = CARTESIAN_POINT ( 'NONE',  ( -39.62287095715004881, -23.48783264082477373, -1.443836473390072594 ) ) ;
#79448 = CARTESIAN_POINT ( 'NONE',  ( -53.64457316383079899, -23.96119346886879953, -0.6495511937832126881 ) ) ;
#79449 = CARTESIAN_POINT ( 'NONE',  ( -16.19606052442943067, -11.93128464602566474, 11.49999999999999645 ) ) ;
#79450 = CARTESIAN_POINT ( 'NONE',  ( 5.097264368844747651, 3.299463065352477908, -27.56135813788838718 ) ) ;
#79451 = CARTESIAN_POINT ( 'NONE',  ( -113.6228709571500559, -24.64965695001469115, 8.947790433994176951 ) ) ;
#79452 = CARTESIAN_POINT ( 'NONE',  ( -99.52287095715009002, -23.96127896942179092, -0.6493128930930167630 ) ) ;
#79453 = CARTESIAN_POINT ( 'NONE',  ( -89.52287095715006160, -29.50250243563736774, 8.947779886222139822 ) ) ;
#79454 = CARTESIAN_POINT ( 'NONE',  ( -109.5228709571500616, -23.47593901973090524, -1.443836447538996426 ) ) ;
#79456 = EDGE_CURVE ( 'NONE', #92987, #60621, #62705, .T. ) ;
#79455 = CARTESIAN_POINT ( 'NONE',  ( -12.90690225449951001, 15.05119527412115055, 11.49999999999998934 ) ) ;
#79457 = CARTESIAN_POINT ( 'NONE',  ( 0.2638585030419089428, -21.76204025362994798, 11.49999999999998934 ) ) ;
#79458 = DIRECTION ( 'NONE',  ( 0.000000000000000000, -1.000000000000000000, 0.000000000000000000 ) ) ;
#79459 = CARTESIAN_POINT ( 'NONE',  ( 9.307004028210867475, 17.29072351678862418, -1.500000000000002220 ) ) ;
#79460 = CARTESIAN_POINT ( 'NONE',  ( 0.02224039135773590858, -0.3828044741864804479, 0.3828044741864790601 ) ) ;
#79461 = EDGE_CURVE ( 'NONE', #27315, #63342, #77393, .T. ) ;
#79462 = VECTOR ( 'NONE', #2947, 1000.000000000000000 ) ;
#79463 = CARTESIAN_POINT ( 'NONE',  ( -54.52287095715006160, -23.96177878511308279, 10.65340807706330217 ) ) ;
#79464 = APPROVAL_ROLE ( '' ) ;
#79465 = VECTOR ( 'NONE', #81125, 1000.000000000000000 ) ;
#79466 = CARTESIAN_POINT ( 'NONE',  ( -115.6228709571500559, -24.62226745350443835, 0.9660975649729570680 ) ) ;
#79467 = CARTESIAN_POINT ( 'NONE',  ( 2.590395174287518643, -6.376774720514415407, 20.05492615153064762 ) ) ;
#79468 = CARTESIAN_POINT ( 'NONE',  ( 20.13950599927006735, 4.067174238878714654, 11.49999999999999645 ) ) ;
#79469 = CARTESIAN_POINT ( 'NONE',  ( 4.595037417369686850, -5.876774720514419847, 20.70846556543617467 ) ) ;
#79470 = EDGE_CURVE ( 'NONE', #53498, #38852, #95004, .T. ) ;
#79471 = CARTESIAN_POINT ( 'NONE',  ( -128.5228709571500758, -24.35013146730205236, 9.818937971375092388 ) ) ;
#79472 = CARTESIAN_POINT ( 'NONE',  ( 5.419076944403256491, 21.93356404788375258, 11.49999999999999645 ) ) ;
#79473 = EDGE_LOOP ( 'NONE', ( #48620, #76727, #59060, #54426 ) ) ;
#79474 =( LENGTH_UNIT ( ) NAMED_UNIT ( * ) SI_UNIT ( .MILLI., .METRE. ) );
#79475 = CARTESIAN_POINT ( 'NONE',  ( -99.93377387090225739, -25.26387419355090103, 4.577608625778666784 ) ) ;
#79476 = CARTESIAN_POINT ( 'NONE',  ( -4.141025641025638748, -6.376774720514427841, 21.75000000000000355 ) ) ;
#79477 = CARTESIAN_POINT ( 'NONE',  ( -50.49617078905069434, -25.31259386660232380, 4.732512649054961607 ) ) ;
#79478 = CARTESIAN_POINT ( 'NONE',  ( -64.52287095715006160, -23.73907113216989728, -1.053371485793254791 ) ) ;
#79479 = CARTESIAN_POINT ( 'NONE',  ( -110.6228709571500843, -23.47596703998600631, 11.44779298504227860 ) ) ;
#79480 = EDGE_CURVE ( 'NONE', #9517, #31838, #85013, .T. ) ;
#79481 = DIRECTION ( 'NONE',  ( -0.1875268396392987258, 0.000000000000000000, -0.9822594791677485837 ) ) ;
#79482 = ADVANCED_FACE ( 'NONE', ( #31737 ), #38844, .T. ) ;
#79483 = B_SPLINE_CURVE_WITH_KNOTS ( 'NONE', 3,
 ( #55391, #47274, #69095, #15808 ),
 .UNSPECIFIED., .F., .F.,
 ( 4, 4 ),
 ( 0.000000000000000000, 9.999999999998900014E-05 ),
 .UNSPECIFIED. ) ;
#79484 = ORIENTED_EDGE ( 'NONE', *, *, #99393, .T. ) ;
#79485 = CARTESIAN_POINT ( 'NONE',  ( -79.57226238056755108, -25.26749951328133648, 5.312439035903004481 ) ) ;
#79486 = CARTESIAN_POINT ( 'NONE',  ( -19.58686714514938387, 11.73587220785771379, -1.500000000000002220 ) ) ;
#79487 = PLANE ( 'NONE',  #30867 ) ;
#79488 = CARTESIAN_POINT ( 'NONE',  ( 21.57151214508649772, 3.625915217019311583E-15, -1.699999999999999956 ) ) ;
#79489 = CARTESIAN_POINT ( 'NONE',  ( -82.54406659160568438, -24.51419770103156281, 9.386484678747185839 ) ) ;
#79490 = CARTESIAN_POINT ( 'NONE',  ( 22.08653571170524543, -4.319401766784854324, 11.49999999999999645 ) ) ;
#79491 = ORIENTED_EDGE ( 'NONE', *, *, #97220, .F. ) ;
#79492 = CARTESIAN_POINT ( 'NONE',  ( -43.62864466859128498, -24.51314013834316086, 0.6176544820404145097 ) ) ;
#79493 = CARTESIAN_POINT ( 'NONE',  ( -21.26704322615652032, -5.532269525099344776, -1.500000000000002220 ) ) ;
#79494 = DIRECTION ( 'NONE',  ( 1.000000000000000000, 3.773278334444166432E-23, 8.201307841325785021E-29 ) ) ;
#79495 = DIRECTION ( 'NONE',  ( 0.000000000000000000, 0.000000000000000000, 1.000000000000000000 ) ) ;
#79496 = CARTESIAN_POINT ( 'NONE',  ( -69.47536397586432599, -25.08820418785056106, 7.294817312633749218 ) ) ;
#79497 = ORIENTED_EDGE ( 'NONE', *, *, #58304, .T. ) ;
#79498 = CARTESIAN_POINT ( 'NONE',  ( -106.6228709571500559, -29.50247984919015209, -1.443849546365048253 ) ) ;
#79499 = CARTESIAN_POINT ( 'NONE',  ( -29.49875734969025842, 5.965225279485572685, 25.61802280011862720 ) ) ;
#79500 = ORIENTED_EDGE ( 'NONE', *, *, #25130, .T. ) ;
#79501 = CARTESIAN_POINT ( 'NONE',  ( 19.18951349294833264, 7.196795126939715459, 11.49999999999998934 ) ) ;
#79502 = ORIENTED_EDGE ( 'NONE', *, *, #51635, .T. ) ;
#79503 = VERTEX_POINT ( 'NONE', #38346 ) ;
#79504 = ORIENTED_EDGE ( 'NONE', *, *, #32957, .F. ) ;
#79505 = ORIENTED_EDGE ( 'NONE', *, *, #50259, .T. ) ;
#79506 = CARTESIAN_POINT ( 'NONE',  ( -84.62287095715001328, -23.73907113216990439, -1.053371485793225704 ) ) ;
#79507 = CARTESIAN_POINT ( 'NONE',  ( 6.977686149863070675, -22.03694335537135984, -1.500000000000002220 ) ) ;
#79508 = CARTESIAN_POINT ( 'NONE',  ( -41.52287095715009002, -23.96177878511308279, 10.65340807706330573 ) ) ;
#79509 = CARTESIAN_POINT ( 'NONE',  ( -9.641467040090685003, 17.89903724589931855, -1.500000000000002220 ) ) ;
#79510 = ORIENTED_EDGE ( 'NONE', *, *, #58426, .F. ) ;
#79511 = DIRECTION ( 'NONE',  ( -0.9496245541219264785, -6.845827386180410961E-16, -0.3133898629642195011 ) ) ;
#79512 = CARTESIAN_POINT ( 'NONE',  ( -92.58855986348115152, -24.34968618360935011, 0.1864209137778965741 ) ) ;
#79513 = CARTESIAN_POINT ( 'NONE',  ( -114.6228709571500701, -23.96177878511308634, 10.65340807706329862 ) ) ;
#79514 = CARTESIAN_POINT ( 'NONE',  ( 4.372949846226492632, -6.376774720514404748, 18.80635842184136308 ) ) ;
#79516 = VERTEX_POINT ( 'NONE', #93123 ) ;
#79515 = CARTESIAN_POINT ( 'NONE',  ( -21.39523464106120088, -1.845724655749456433, 11.49999999999999645 ) ) ;
#79517 = CARTESIAN_POINT ( 'NONE',  ( -9.278253834636473130, -5.876774720514426953, 21.78128695274316229 ) ) ;
#79518 = DIRECTION ( 'NONE',  ( 0.000000000000000000, 0.000000000000000000, -1.000000000000000000 ) ) ;
#79519 = VERTEX_POINT ( 'NONE', #69299 ) ;
#79520 = CARTESIAN_POINT ( 'NONE',  ( -1.268444833121266546, 20.69640364028325052, -1.500000000000002220 ) ) ;
#79521 = VECTOR ( 'NONE', #51085, 1000.000000000000114 ) ;
#79522 = ORIENTED_EDGE ( 'NONE', *, *, #39127, .T. ) ;
#79524 = EDGE_LOOP ( 'NONE', ( #55077, #64526, #43534, #46074 ) ) ;
#79523 = CARTESIAN_POINT ( 'NONE',  ( -125.5909827109052941, -23.85016227208582151, -0.8807180028928047744 ) ) ;
#79525 = PLANE ( 'NONE',  #39028 ) ;
#79526 = CARTESIAN_POINT ( 'NONE',  ( -107.6228709571500559, -24.50216790748098461, 0.6166512839513795807 ) ) ;
#79527 = ORIENTED_EDGE ( 'NONE', *, *, #95286, .F. ) ;
#79528 = ORIENTED_EDGE ( 'NONE', *, *, #36432, .F. ) ;
#79529 = CARTESIAN_POINT ( 'NONE',  ( -40.52287095715006870, -24.92579138211019085, 1.929029949965664015 ) ) ;
#79530 = B_SPLINE_CURVE_WITH_KNOTS ( 'NONE', 3,
 ( #95929, #57395, #88323, #11195 ),
 .UNSPECIFIED., .F., .F.,
 ( 4, 4 ),
 ( 0.4090588724279532462, 0.4100596194687187723 ),
 .UNSPECIFIED. ) ;
#79531 = B_SPLINE_CURVE_WITH_KNOTS ( 'NONE', 3,
 ( #72291, #16985, #15978, #77873, #78873, #39324, #31719, #16478 ),
 .UNSPECIFIED., .F., .F.,
 ( 4, 2, 2, 4 ),
 ( 6.391158118961346620E-06, 0.002007136338672917911, 0.003007508928949897790, 0.004007881519226878103 ),
 .UNSPECIFIED. ) ;
#79532 = PLANE ( 'NONE',  #44882 ) ;
#79533 = CARTESIAN_POINT ( 'NONE',  ( -29.03431458974025148, -24.86372088895192789, 2.176981720316843116 ) ) ;
#79535 = ORIENTED_EDGE ( 'NONE', *, *, #92795, .F. ) ;
#79534 = CARTESIAN_POINT ( 'NONE',  ( -18.24146354680218707, 12.35505607031776165, 11.49999999999999645 ) ) ;
#79536 = CARTESIAN_POINT ( 'NONE',  ( -103.5600735941376485, -23.48783264082477018, -1.443836473390091246 ) ) ;
#79537 = CARTESIAN_POINT ( 'NONE',  ( -19.94007547503736788, -10.58355046294204094, -1.500000000000002220 ) ) ;
#79539 = VERTEX_POINT ( 'NONE', #69802 ) ;
#79538 = PLANE ( 'NONE',  #92791 ) ;
#79540 = AXIS2_PLACEMENT_3D ( 'NONE', #804, #77410, #47486 ) ;
#79541 = EDGE_LOOP ( 'NONE', ( #23998, #34271, #31172, #26255 ) ) ;
#79542 = AXIS2_PLACEMENT_3D ( 'NONE', #86620, #9496, #54191 ) ;
#79543 = CARTESIAN_POINT ( 'NONE',  ( -88.52287095715004739, -23.96177878511308634, 10.65340807706329329 ) ) ;
#79544 = CARTESIAN_POINT ( 'NONE',  ( -128.6228709571500417, -23.48783264082479505, -1.443836473390056829 ) ) ;
#79545 = VERTEX_POINT ( 'NONE', #31232 ) ;
#79546 = CARTESIAN_POINT ( 'NONE',  ( 4.565063516603933280, 20.63981631578574039, 11.49999999999998934 ) ) ;
#79547 = DIRECTION ( 'NONE',  ( 0.000000000000000000, -0.9999999999976377785, -2.173523156925979128E-06 ) ) ;
#79548 = EDGE_CURVE ( 'NONE', #55067, #44101, #30729, .T. ) ;
#79549 = CARTESIAN_POINT ( 'NONE',  ( -51.71530383401179876, -25.03148599924218232, 6.909342695069468299 ) ) ;
#79550 = DIRECTION ( 'NONE',  ( -1.000000000000000000, 0.000000000000000000, -0.000000000000000000 ) ) ;
#79551 = CARTESIAN_POINT ( 'NONE',  ( 0.6000000000000009770, 21.89999999999999858, 0.000000000000000000 ) ) ;
#79552 = CARTESIAN_POINT ( 'NONE',  ( -14.87450875942801254, -16.50811611944624602, -1.500000000000002220 ) ) ;
#79553 = EDGE_CURVE ( 'NONE', #82501, #56235, #7836, .T. ) ;
#79554 = CARTESIAN_POINT ( 'NONE',  ( -114.5568548638380264, -23.73766607897672287, -1.055555164236428700 ) ) ;
#79555 = EDGE_CURVE ( 'NONE', #74261, #61510, #23605, .T. ) ;
#79556 = VERTEX_POINT ( 'NONE', #86020 ) ;
#79557 = DIRECTION ( 'NONE',  ( -3.773278334453079030E-23, 0.9999999999976377785, 2.173523156925979128E-06 ) ) ;
#79558 = LINE ( 'NONE', #33378, #18443 ) ;
#79559 = CARTESIAN_POINT ( 'NONE',  ( -13.55963120218723361, -13.89248740512243430, 11.49999999999999645 ) ) ;
#79560 = EDGE_CURVE ( 'NONE', #39568, #60922, #85514, .T. ) ;
#79561 = EDGE_CURVE ( 'NONE', #56711, #85538, #61702, .T. ) ;
#79562 = CARTESIAN_POINT ( 'NONE',  ( -40.53071971990141975, -25.11095176003700757, 2.835807588750839603 ) ) ;
#79563 = CARTESIAN_POINT ( 'NONE',  ( -33.62287095715003460, -23.95044443724991368, 10.65354141964649948 ) ) ;
#79564 = CARTESIAN_POINT ( 'NONE',  ( -19.44331071757236273, 1.017868325215548708, -1.500000000000002220 ) ) ;
#79565 = CARTESIAN_POINT ( 'NONE',  ( -19.74196057798672399, -8.316236533413031040, -1.500000000000002220 ) ) ;
#79566 = DIRECTION ( 'NONE',  ( -0.4009304992412300317, -6.845827386180410961E-16, -0.9161084732596779245 ) ) ;
#79567 = CARTESIAN_POINT ( 'NONE',  ( -60.53292233517615273, -24.83644354574317603, 8.397322867105112110 ) ) ;
#79568 = CARTESIAN_POINT ( 'NONE',  ( -100.6228709571500701, -24.63345952396256067, 9.038047939301499412 ) ) ;
#79569 = CARTESIAN_POINT ( 'NONE',  ( -101.6228709571500559, -24.64965695001469115, 8.947790433994178727 ) ) ;
#79570 = CARTESIAN_POINT ( 'NONE',  ( 16.28376985728763415, 15.88423345705086298, -1.500000000000002220 ) ) ;
#79571 = DIRECTION ( 'NONE',  ( 1.000000000000000000, 0.000000000000000000, 0.000000000000000000 ) ) ;
#79572 = CARTESIAN_POINT ( 'NONE',  ( -98.62537220214177580, -24.51314013834316086, 0.6176544820404117342 ) ) ;
#79573 = CARTESIAN_POINT ( 'NONE',  ( -98.62287095715005592, -23.48783264082478439, -1.443836473390061936 ) ) ;
#79574 = CARTESIAN_POINT ( 'NONE',  ( 5.644138345009856117, 19.01542066204735448, 11.49999999999999645 ) ) ;
#79575 = CARTESIAN_POINT ( 'NONE',  ( -69.52287095715009002, -23.48783264082477018, -1.443836473390092801 ) ) ;
#79576 = LINE ( 'NONE', #87696, #71696 ) ;
#79577 = CARTESIAN_POINT ( 'NONE',  ( -48.66104112521659886, -23.48783264082477729, -1.443836473390069486 ) ) ;
#79578 = ORIENTED_EDGE ( 'NONE', *, *, #6598, .T. ) ;
#79579 = DIRECTION ( 'NONE',  ( -0.000000000000000000, 0.000000000000000000, -1.000000000000000000 ) ) ;
#79580 = EDGE_CURVE ( 'NONE', #7329, #74994, #70305, .T. ) ;
#79581 = FACE_OUTER_BOUND ( 'NONE', #89782, .T. ) ;
#79582 = CARTESIAN_POINT ( 'NONE',  ( -75.52287095715006160, -24.99132157543084176, 2.256160258750667502 ) ) ;
#79583 = CARTESIAN_POINT ( 'NONE',  ( -17.53059066697263546, 12.75712217820542627, 11.49999999999998934 ) ) ;
#79584 = CARTESIAN_POINT ( 'NONE',  ( -56.54791891829369632, -24.15620529776628445, 10.23563542870660648 ) ) ;
#79585 = CARTESIAN_POINT ( 'NONE',  ( 16.17817332762582794, -10.88531698672339942, -1.500000000000002220 ) ) ;
#79586 = LINE ( 'NONE', #3976, #6964 ) ;
#79587 = ADVANCED_FACE ( 'NONE', ( #99238 ), #39428, .T. ) ;
#79588 = ORIENTED_EDGE ( 'NONE', *, *, #24806, .T. ) ;
#79589 = CARTESIAN_POINT ( 'NONE',  ( -13.80512455850298714, -15.04058748057734896, 11.49999999999999645 ) ) ;
#79590 = DIRECTION ( 'NONE',  ( 0.000000000000000000, -1.000000000000000000, 0.000000000000000000 ) ) ;
#79591 = VECTOR ( 'NONE', #18912, 1000.000000000000114 ) ;
#79592 = FACE_OUTER_BOUND ( 'NONE', #16260, .T. ) ;
#79593 = VERTEX_POINT ( 'NONE', #95138 ) ;
#79594 = CARTESIAN_POINT ( 'NONE',  ( -80.30096212672883382, -25.03465771498776959, 7.554806159496210149 ) ) ;
#79595 = DIRECTION ( 'NONE',  ( 1.000000000000000000, 3.773278334444167608E-23, 8.201307833595939069E-29 ) ) ;
#79596 = CARTESIAN_POINT ( 'NONE',  ( -125.5228709571500616, -24.99156044556120904, 7.747789690856173195 ) ) ;
#79597 = CARTESIAN_POINT ( 'NONE',  ( -49.45828852499023753, -25.31439371758138890, 5.632644884985086975 ) ) ;
#79598 = CARTESIAN_POINT ( 'NONE',  ( -22.05275734969026047, -5.965225279485572685, 31.02402280011862246 ) ) ;
#79599 = CARTESIAN_POINT ( 'NONE',  ( -4.531374827497722357, 4.263680106169587702, -2.677392948487098267E-15 ) ) ;
#79600 = EDGE_LOOP ( 'NONE', ( #808, #25213, #58064, #86753, #63144, #97281 ) ) ;
#79601 = DIRECTION ( 'NONE',  ( 0.000000000000000000, 0.000000000000000000, 1.000000000000000000 ) ) ;
#79602 = ADVANCED_FACE ( 'NONE', ( #3314 ), #70212, .T. ) ;
#79603 = VECTOR ( 'NONE', #18049, 1000.000000000000114 ) ;
#79604 = CARTESIAN_POINT ( 'NONE',  ( 4.748521865011817944, 22.44708532425888592, 11.49999999999999645 ) ) ;
#79605 = CARTESIAN_POINT ( 'NONE',  ( 16.28376985728763415, 15.88423345705086298, 11.49999999999998934 ) ) ;
#79606 = CARTESIAN_POINT ( 'NONE',  ( -110.5886784188881506, -24.63419186844610920, 9.035850630976920428 ) ) ;
#79607 = DIRECTION ( 'NONE',  ( 1.000000000000000000, 0.000000000000000000, 0.000000000000000000 ) ) ;
#79608 = CARTESIAN_POINT ( 'NONE',  ( -90.50427414553793426, -24.63355581998384736, 0.9682620441943978751 ) ) ;
#79609 = CARTESIAN_POINT ( 'NONE',  ( 0.8126045299064900140, -1.450440077808301975, -8.999999999999998224 ) ) ;
#79610 = ADVANCED_FACE ( 'NONE', ( #87530 ), #86518, .F. ) ;
#79611 = CARTESIAN_POINT ( 'NONE',  ( -17.40403014803320758, -13.24600170205644289, 11.49999999999998934 ) ) ;
#79612 = CARTESIAN_POINT ( 'NONE',  ( -69.56521275654560554, -23.48786465467240347, 11.44779295918255002 ) ) ;
#79613 = CARTESIAN_POINT ( 'NONE',  ( -27.53894643728430580, -24.76187901197181773, 2.282776568623821500 ) ) ;
#79614 = CARTESIAN_POINT ( 'NONE',  ( 22.02124265030973760, 6.143225279485574397, 12.85402280011862430 ) ) ;
#79615 = CARTESIAN_POINT ( 'NONE',  ( -98.92944106970213625, -25.31200674615046253, 5.790834157640309066 ) ) ;
#79616 = VERTEX_POINT ( 'NONE', #98617 ) ;
#79617 = CARTESIAN_POINT ( 'NONE',  ( -19.95082702767638239, -4.354873812894156870, 11.49999999999998934 ) ) ;
#79618 = EDGE_LOOP ( 'NONE', ( #18129, #8774, #99933, #95968 ) ) ;
#79619 = EDGE_LOOP ( 'NONE', ( #41717, #10036, #42344, #51199 ) ) ;
#79620 = CARTESIAN_POINT ( 'NONE',  ( -23.02147672596084149, 0.6323230698326208765, -1.500000000000002220 ) ) ;
#79621 = CARTESIAN_POINT ( 'NONE',  ( -1.345681049247692940, -6.376774720514410077, 19.69174559449348294 ) ) ;
#79622 = ORIENTED_EDGE ( 'NONE', *, *, #89286, .T. ) ;
#79623 = CARTESIAN_POINT ( 'NONE',  ( -110.6167769405262362, -25.21876678810425076, 6.586934760171002878 ) ) ;
#79624 = CARTESIAN_POINT ( 'NONE',  ( -32.62287095715004881, -24.65952944569304250, 1.056160979905691688 ) ) ;
#79625 = DIRECTION ( 'NONE',  ( -1.000000000000000000, 3.469446951953611033E-15, 0.000000000000000000 ) ) ;
#79626 = DIRECTION ( 'NONE',  ( -0.000000000000000000, 0.000000000000000000, 1.000000000000000000 ) ) ;
#79628 = ORIENTED_EDGE ( 'NONE', *, *, #70981, .T. ) ;
#79627 = CARTESIAN_POINT ( 'NONE',  ( 13.65650298889772962, 16.33668418983593185, 11.49999999999999645 ) ) ;
#79629 = VERTEX_POINT ( 'NONE', #34740 ) ;
#79630 = CARTESIAN_POINT ( 'NONE',  ( -21.98633505697190671, -3.258044352128648846, -1.500000000000002220 ) ) ;
#79631 = CARTESIAN_POINT ( 'NONE',  ( 3.034461355793923509, -20.43525710956717845, -1.500000000000002220 ) ) ;
#79632 = VERTEX_POINT ( 'NONE', #19004 ) ;
#79633 = DIRECTION ( 'NONE',  ( 1.000000000000000000, 3.773278334444166432E-23, 8.201307841325785021E-29 ) ) ;
#79634 = CARTESIAN_POINT ( 'NONE',  ( -95.62858372876527824, -24.63419186844610920, 9.035850630976922204 ) ) ;
#79635 = ORIENTED_EDGE ( 'NONE', *, *, #93039, .T. ) ;
#79636 = DIRECTION ( 'NONE',  ( -3.773278334453079030E-23, 0.9999999999976377785, 2.173523156925979128E-06 ) ) ;
#79637 = ORIENTED_EDGE ( 'NONE', *, *, #74730, .T. ) ;
#79638 = PLANE ( 'NONE',  #36662 ) ;
#79639 = CARTESIAN_POINT ( 'NONE',  ( 3.138110291115776995, 11.54688212118755075, 0.000000000000000000 ) ) ;
#79640 = CARTESIAN_POINT ( 'NONE',  ( 20.66465755290784401, -3.126920214821775623, -1.500000000000002220 ) ) ;
#79641 = CARTESIAN_POINT ( 'NONE',  ( -16.21501377034323710, -14.60173171477820198, 11.49999999999999645 ) ) ;
#79642 = CARTESIAN_POINT ( 'NONE',  ( -26.56775203954515874, -24.77993665650937061, 6.997625439131231140 ) ) ;
#79643 = CARTESIAN_POINT ( 'NONE',  ( 17.91726403014145319, -0.5000000000000000000, -1.691563534834430227 ) ) ;
#79644 = CARTESIAN_POINT ( 'NONE',  ( 3.433349652534986696, 22.22849440524942111, -1.500000000000002220 ) ) ;
#79645 = CARTESIAN_POINT ( 'NONE',  ( 0.8369575198195864374, -20.89415947959451003, -1.500000000000002220 ) ) ;
#79646 = CARTESIAN_POINT ( 'NONE',  ( -26.33488822642538452, -24.88149058068788122, 6.524121877972378414 ) ) ;
#79647 = CARTESIAN_POINT ( 'NONE',  ( -52.52287095715008292, -24.66019654487198665, 8.947790411086131712 ) ) ;
#79648 = CARTESIAN_POINT ( 'NONE',  ( 4.910384361841649614, -5.876774720514420736, 20.73924463800384643 ) ) ;
#79649 = ORIENTED_EDGE ( 'NONE', *, *, #18749, .F. ) ;
#79650 = VERTEX_POINT ( 'NONE', #35243 ) ;
#79651 = VERTEX_POINT ( 'NONE', #90022 ) ;
#79652 = AXIS2_PLACEMENT_3D ( 'NONE', #90072, #22528, #5329 ) ;
#79653 = CARTESIAN_POINT ( 'NONE',  ( -52.65162834406839920, -23.73766607897671221, -1.055555164236436472 ) ) ;
#79654 = VERTEX_POINT ( 'NONE', #36732 ) ;
#79655 = B_SPLINE_CURVE_WITH_KNOTS ( 'NONE', 3,
 ( #21936, #55811, #71530, #53419, #87236, #71027 ),
 .UNSPECIFIED., .F., .F.,
 ( 4, 2, 4 ),
 ( 0.000000000000000000, 0.001380764517854766700, 0.002761529035709533401 ),
 .UNSPECIFIED. ) ;
#79656 = CARTESIAN_POINT ( 'NONE',  ( -4.378498130703003532, 20.98420022172975763, -1.500000000000002220 ) ) ;
#79657 = CARTESIAN_POINT ( 'NONE',  ( 22.34790896907852442, -0.4833156648990815651, 11.49999999999999645 ) ) ;
#79658 = VERTEX_POINT ( 'NONE', #20992 ) ;
#79659 = CARTESIAN_POINT ( 'NONE',  ( 2.230654205607476737, -2.168404344971008868E-16, 0.1647943925233645579 ) ) ;
#79660 = CARTESIAN_POINT ( 'NONE',  ( 5.245434476726341444, -20.39595507048906242, -1.500000000000002220 ) ) ;
#79661 = CARTESIAN_POINT ( 'NONE',  ( -30.49162772548749700, -24.48101848413686099, 9.440108529385041081 ) ) ;
#79662 = EDGE_CURVE ( 'NONE', #80731, #55399, #28128, .T. ) ;
#79663 = CARTESIAN_POINT ( 'NONE',  ( -16.79965634883036074, 10.71410036745690597, -1.500000000000002220 ) ) ;
#79664 = CARTESIAN_POINT ( 'NONE',  ( -50.57647688411456244, -24.92592662359560762, 8.075495903017996469 ) ) ;
#79665 = CARTESIAN_POINT ( 'NONE',  ( 10.45000000000000462, 1.999999999999998668, 19.19609335255483984 ) ) ;
#79666 = CARTESIAN_POINT ( 'NONE',  ( 17.21905055353458991, -13.78536315820828229, -1.500000000000002220 ) ) ;
#79667 = ORIENTED_EDGE ( 'NONE', *, *, #62556, .F. ) ;
#79668 = FACE_OUTER_BOUND ( 'NONE', #100056, .T. ) ;
#79669 = ADVANCED_FACE ( 'NONE', ( #65713 ), #59085, .F. ) ;
#79670 = CARTESIAN_POINT ( 'NONE',  ( -2.285970405126252825, -6.376774720514408301, 19.14905311829361167 ) ) ;
#79671 = CARTESIAN_POINT ( 'NONE',  ( 19.93353245626563819, -6.116835970281883306, 11.49999999999999645 ) ) ;
#79672 = ADVANCED_FACE ( 'NONE', ( #75282 ), #82400, .T. ) ;
#79673 = CARTESIAN_POINT ( 'NONE',  ( -25.52552615364072253, -24.47148205344575800, 8.290116722409051064 ) ) ;
#79674 = AXIS2_PLACEMENT_3D ( 'NONE', #66129, #67117, #52876 ) ;
#79675 = EDGE_CURVE ( 'NONE', #59182, #4570, #39286, .T. ) ;
#79676 = DIRECTION ( 'NONE',  ( -3.773278334453079618E-23, 0.9999999999976377785, 2.173523156925979975E-06 ) ) ;
#79677 = PRODUCT_DEFINITION_FORMATION_WITH_SPECIFIED_SOURCE ( 'ANY', '', #42576, .NOT_KNOWN. ) ;
#79678 = CARTESIAN_POINT ( 'NONE',  ( 9.940598223437577374, -6.376774720514426953, 17.91871304725684766 ) ) ;
#79679 = CARTESIAN_POINT ( 'NONE',  ( 1.434216325579209750, -21.26356369375713484, -1.500000000000002220 ) ) ;
#79680 = DIRECTION ( 'NONE',  ( -0.000000000000000000, -1.000000000000000000, -0.000000000000000000 ) ) ;
#79681 = ADVANCED_FACE ( 'NONE', ( #66213 ), #51466, .F. ) ;
#79682 = CARTESIAN_POINT ( 'NONE',  ( 1.408343819019456028E-16, -16.94322527948557422, 1.149999999999999911 ) ) ;
#79683 = DIRECTION ( 'NONE',  ( 1.000000000000000000, -0.000000000000000000, 0.000000000000000000 ) ) ;
#79684 = CARTESIAN_POINT ( 'NONE',  ( -68.62287095715005592, -23.48783264082478439, -1.443836473390067265 ) ) ;
#79685 = CARTESIAN_POINT ( 'NONE',  ( -18.09186581907994196, -13.49991075323410250, -1.500000000000002220 ) ) ;
#79686 = CARTESIAN_POINT ( 'NONE',  ( -51.52287095715004739, -23.73934037231757088, 11.05740245334329508 ) ) ;
#79687 = ORIENTED_EDGE ( 'NONE', *, *, #42932, .F. ) ;
#79688 = CARTESIAN_POINT ( 'NONE',  ( -3.737436867076076030, 13.63388347648318444, 0.000000000000000000 ) ) ;
#79689 = CARTESIAN_POINT ( 'NONE',  ( -31.53139797621515328, -24.51419770103156637, 9.386484678747187615 ) ) ;
#79690 = CARTESIAN_POINT ( 'NONE',  ( -0.8432318219891272726, -19.69000482574202238, 11.49999999999999645 ) ) ;
#79691 = CARTESIAN_POINT ( 'NONE',  ( -32.07722060962683486, -25.26313220207395105, 6.450164452698709638 ) ) ;
#79692 = CARTESIAN_POINT ( 'NONE',  ( 14.63527791052759319, -4.349658986764154633, -28.08406249416238154 ) ) ;
#79693 = EDGE_CURVE ( 'NONE', #57281, #33604, #43852, .T. ) ;
#79694 = ORIENTED_EDGE ( 'NONE', *, *, #80711, .F. ) ;
#79695 = PLANE ( 'NONE',  #86267 ) ;
#79696 = CARTESIAN_POINT ( 'NONE',  ( -127.4728709594060092, -25.21147767388033500, 8.000950760261464012 ) ) ;
#79697 = CARTESIAN_POINT ( 'NONE',  ( -61.52287095715008292, -24.51387760970724727, 9.387446482453409402 ) ) ;
#79698 = DIRECTION ( 'NONE',  ( 3.773278334444166432E-23, -1.000000000000000000, 0.000000000000000000 ) ) ;
#79700 = EDGE_CURVE ( 'NONE', #88020, #95160, #22380, .T. ) ;
#79699 = DIRECTION ( 'NONE',  ( -0.000000000000000000, -0.000000000000000000, -1.000000000000000000 ) ) ;
#79701 = CARTESIAN_POINT ( 'NONE',  ( -60.62287095715004881, -23.47593901973091235, -1.443836447539007972 ) ) ;
#79702 = CARTESIAN_POINT ( 'NONE',  ( -15.39140670439391378, -12.39996395878027791, -1.500000000000002220 ) ) ;
#79703 = ORIENTED_EDGE ( 'NONE', *, *, #15418, .T. ) ;
#79704 = CARTESIAN_POINT ( 'NONE',  ( -2.479824388263708990, 20.08073137130260122, 11.49999999999999645 ) ) ;
#79705 = CARTESIAN_POINT ( 'NONE',  ( 6.059061188053544988, -5.876774720514417183, 20.16803580207560742 ) ) ;
#79706 = AXIS2_PLACEMENT_3D ( 'NONE', #96635, #66222, #97632 ) ;
#79707 = B_SPLINE_CURVE_WITH_KNOTS ( 'NONE', 3,
 ( #57286, #11573, #43539, #49660, #51144, #74476 ),
 .UNSPECIFIED., .F., .F.,
 ( 4, 2, 4 ),
 ( 0.000000000000000000, 0.001380901958385382473, 0.002761803916770764946 ),
 .UNSPECIFIED. ) ;
#79708 = VERTEX_POINT ( 'NONE', #27633 ) ;
#79709 = CARTESIAN_POINT ( 'NONE',  ( -40.52287095715006870, -23.47593901973090169, -1.443836447538997092 ) ) ;
#79710 = LINE ( 'NONE', #70102, #73457 ) ;
#79711 = DIRECTION ( 'NONE',  ( 0.000000000000000000, 0.000000000000000000, 1.000000000000000000 ) ) ;
#79712 = CARTESIAN_POINT ( 'NONE',  ( -69.65500006739829075, -25.13901286917058187, 2.995211960630785430 ) ) ;
#79713 = PLANE ( 'NONE',  #52217 ) ;
#79714 = CARTESIAN_POINT ( 'NONE',  ( -57.52287095715005449, -29.50247984919015209, -1.443849546365056913 ) ) ;
#79715 = CARTESIAN_POINT ( 'NONE',  ( -7.547287378330592489, -18.53391252851691462, 11.49999999999998934 ) ) ;
#79716 = EDGE_CURVE ( 'NONE', #27769, #59549, #62317, .T. ) ;
#79717 = CARTESIAN_POINT ( 'NONE',  ( -99.16315266720698673, -25.27533051753978910, 3.707282223935987275 ) ) ;
#79718 = ORIENTED_EDGE ( 'NONE', *, *, #58045, .F. ) ;
#79719 = DIRECTION ( 'NONE',  ( 0.000000000000000000, 0.000000000000000000, -1.000000000000000000 ) ) ;
#79720 = FACE_OUTER_BOUND ( 'NONE', #74052, .T. ) ;
#79721 = DIRECTION ( 'NONE',  ( -3.773278334453079618E-23, 0.9999999999976377785, 2.173523156925979975E-06 ) ) ;
#79722 = VECTOR ( 'NONE', #81222, 1000.000000000000000 ) ;
#79723 = LINE ( 'NONE', #17326, #52903 ) ;
#79724 = CARTESIAN_POINT ( 'NONE',  ( -73.58111945615931404, -24.65952944569304606, 1.056160979905700126 ) ) ;
#79725 = FACE_OUTER_BOUND ( 'NONE', #32968, .T. ) ;
#79726 = ADVANCED_FACE ( 'NONE', ( #81909 ), #84764, .T. ) ;
#79727 = CARTESIAN_POINT ( 'NONE',  ( -99.90536206787731999, -25.32724633150700200, 4.398074151685131383 ) ) ;
#79728 = ORIENTED_EDGE ( 'NONE', *, *, #95002, .F. ) ;
#79729 = B_SPLINE_CURVE_WITH_KNOTS ( 'NONE', 3,
 ( #76596, #60906, #36052, #75595, #21312, #51785 ),
 .UNSPECIFIED., .F., .F.,
 ( 4, 2, 4 ),
 ( 0.004212217532642030179, 0.005885052055372081044, 0.007557886578102131908 ),
 .UNSPECIFIED. ) ;
#79730 = CARTESIAN_POINT ( 'NONE',  ( 17.43904876784772284, 10.37648870149486413, -1.500000000000002220 ) ) ;
#79731 = VERTEX_POINT ( 'NONE', #45352 ) ;
#79732 = ADVANCED_FACE ( 'NONE', ( #52462 ), #60587, .F. ) ;
#79733 = CARTESIAN_POINT ( 'NONE',  ( -0.02075734969026423599, -6.376774720514426953, -0.08597719988137648983 ) ) ;
#79734 = CARTESIAN_POINT ( 'NONE',  ( -127.5561563095140798, -23.73791477778912551, 11.05961554403169167 ) ) ;
#79735 = CARTESIAN_POINT ( 'NONE',  ( -59.54286866093478636, -24.35071581493543391, 9.817618358456035921 ) ) ;
#79736 = DIRECTION ( 'NONE',  ( -1.000000000000000000, 0.000000000000000000, 0.000000000000000000 ) ) ;
#79737 = CIRCLE ( 'NONE', #65232, 91.74549126261076992 ) ;
#79738 = CARTESIAN_POINT ( 'NONE',  ( -30.47287095715006799, -25.25852548890106419, 3.876286009398770993 ) ) ;
#79739 = CARTESIAN_POINT ( 'NONE',  ( -18.51692787870624102, -10.26217664800131502, 11.49999999999999645 ) ) ;
#79740 = CC_DESIGN_APPROVAL ( #77331, ( #16510 ) ) ;
#79741 = CARTESIAN_POINT ( 'NONE',  ( -20.57447749561850969, 8.151157241358404804, 11.49999999999998934 ) ) ;
#79742 = B_SPLINE_CURVE_WITH_KNOTS ( 'NONE', 3,
 ( #66720, #44859, #52468, #83400, #28134, #12393, #37729, #75288 ),
 .UNSPECIFIED., .F., .F.,
 ( 4, 2, 2, 4 ),
 ( -0.001224873891641424777, -0.0002244903592271093630, 0.0007758931731872060512, 0.002776660238015836880 ),
 .UNSPECIFIED. ) ;
#79743 = B_SPLINE_CURVE_WITH_KNOTS ( 'NONE', 3,
 ( #76883, #38343, #29768, #53621 ),
 .UNSPECIFIED., .F., .F.,
 ( 4, 4 ),
 ( 0.000000000000000000, 9.999999999998897304E-05 ),
 .UNSPECIFIED. ) ;
#79745 = CARTESIAN_POINT ( 'NONE',  ( 9.245221688665949955, -18.36014492602614467, 11.49999999999998934 ) ) ;
#79744 = CC_DESIGN_PERSON_AND_ORGANIZATION_ASSIGNMENT ( #71367, #31798, ( #91265 ) ) ;
#79746 = VERTEX_POINT ( 'NONE', #69680 ) ;
#79747 = CARTESIAN_POINT ( 'NONE',  ( -6.660000000000001030, -10.97586050609889519, -0.8902240841051127784 ) ) ;
#79748 = EDGE_LOOP ( 'NONE', ( #47837, #96966, #71302, #86732 ) ) ;
#79749 = CARTESIAN_POINT ( 'NONE',  ( -37.52287095715006870, -23.47596703998600631, 11.44779298504229281 ) ) ;
#79750 = LINE ( 'NONE', #94477, #79389 ) ;
#79751 = ORIENTED_EDGE ( 'NONE', *, *, #25531, .F. ) ;
#79752 = ORIENTED_EDGE ( 'NONE', *, *, #85496, .F. ) ;
#79753 = ORIENTED_EDGE ( 'NONE', *, *, #36061, .F. ) ;
#79754 = CARTESIAN_POINT ( 'NONE',  ( 8.749999999999769074, 18.74999999999999645, 2.100000000000000089 ) ) ;
#79755 = CARTESIAN_POINT ( 'NONE',  ( 6.431189903846153300, -5.876774720514415407, 20.08974358974358765 ) ) ;
#79756 = DIRECTION ( 'NONE',  ( -0.7071067811865434649, 0.7071067811865516806, 0.000000000000000000 ) ) ;
#79757 = CARTESIAN_POINT ( 'NONE',  ( 4.478411676025833010, -20.21887007069289766, -1.500000000000002220 ) ) ;
#79758 = CARTESIAN_POINT ( 'NONE',  ( -15.38093110518717666, 15.28219592669002402, 11.49999999999999645 ) ) ;
#79759 = VERTEX_POINT ( 'NONE', #15374 ) ;
#79760 = CARTESIAN_POINT ( 'NONE',  ( -60.52287095715006870, -23.85229601349281126, 10.88205029485767561 ) ) ;
#79761 = DIRECTION ( 'NONE',  ( -3.773278334453079030E-23, 0.9999999999976377785, 2.173523156925979128E-06 ) ) ;
#79762 = CARTESIAN_POINT ( 'NONE',  ( 22.03792223356247604, -4.036589945906135846, -1.500000000000002220 ) ) ;
#79763 = CARTESIAN_POINT ( 'NONE',  ( -10.21384395349166496, -6.475225279485573360, 29.49402280011861777 ) ) ;
#79764 = LINE ( 'NONE', #11752, #69196 ) ;
#79765 = VERTEX_POINT ( 'NONE', #62074 ) ;
#79766 = FACE_OUTER_BOUND ( 'NONE', #45472, .T. ) ;
#79767 = CARTESIAN_POINT ( 'NONE',  ( 15.29947330337543754, 6.475225279485573360, -27.16854002387008649 ) ) ;
#79768 = B_SPLINE_SURFACE_WITH_KNOTS ( 'NONE', 3, 1, ( 
 ( #28610, #27116 ),
 ( #18497, #49471 ),
 ( #96132, #58084 ),
 ( #89018, #42855 ),
 ( #19493, #43348 ),
 ( #73783, #4282 ) ),
 .UNSPECIFIED., .F., .F., .F.,
 ( 4, 2, 4 ),
 ( 2, 2 ),
 ( 0.000000000000000000, 0.5000000000000000000, 1.000000000000000000 ),
 ( 0.000000000000000000, 1.000000000000000000 ),
 .UNSPECIFIED. ) ;
#79769 = ORIENTED_EDGE ( 'NONE', *, *, #93827, .F. ) ;
#79770 = ORIENTED_EDGE ( 'NONE', *, *, #90605, .T. ) ;
#79771 = DIRECTION ( 'NONE',  ( 0.000000000000000000, 0.000000000000000000, 1.000000000000000000 ) ) ;
#79772 = VERTEX_POINT ( 'NONE', #52963 ) ;
#79773 = AXIS2_PLACEMENT_3D ( 'NONE', #38488, #1937, #23748 ) ;
#79774 = CARTESIAN_POINT ( 'NONE',  ( 5.514125806255895004E-17, -29.50247984919086264, -1.443849221408822103 ) ) ;
#79775 = CARTESIAN_POINT ( 'NONE',  ( 4.782327729912362990, -20.71560727227588927, -1.500000000000002220 ) ) ;
#79776 = ORIENTED_EDGE ( 'NONE', *, *, #61512, .T. ) ;
#79777 = DIRECTION ( 'NONE',  ( -1.000000000000000000, 0.000000000000000000, -0.000000000000000000 ) ) ;
#79778 = CARTESIAN_POINT ( 'NONE',  ( -13.95179422449595208, 16.79422078803934326, -1.500000000000002220 ) ) ;
#79779 = CARTESIAN_POINT ( 'NONE',  ( -103.5856489833065410, -24.66019654487200086, 8.947790411086119278 ) ) ;
#79780 = LINE ( 'NONE', #18389, #22593 ) ;
#79781 = CARTESIAN_POINT ( 'NONE',  ( -109.6228709571500417, -24.65952944569305316, 1.056160979905704345 ) ) ;
#79782 = CARTESIAN_POINT ( 'NONE',  ( 6.672210613628693388, 20.84999943921648935, -1.500000000000002220 ) ) ;
#79783 = CARTESIAN_POINT ( 'NONE',  ( 7.164812103570541879, -6.376774720514422512, 20.85668272347560404 ) ) ;
#79784 = ORIENTED_EDGE ( 'NONE', *, *, #47429, .T. ) ;
#79785 = DIRECTION ( 'NONE',  ( 0.000000000000000000, 1.000000000000000000, 0.000000000000000000 ) ) ;
#79786 = CARTESIAN_POINT ( 'NONE',  ( -48.87380231474225667, -25.26337302231874915, 6.137091984676827039 ) ) ;
#79787 = ORIENTED_EDGE ( 'NONE', *, *, #24568, .T. ) ;
#79788 = ORIENTED_EDGE ( 'NONE', *, *, #35950, .T. ) ;
#79789 = ORIENTED_EDGE ( 'NONE', *, *, #20118, .T. ) ;
#79790 = VECTOR ( 'NONE', #100262, 1000.000000000000114 ) ;
#79791 = EDGE_CURVE ( 'NONE', #52807, #37472, #57469, .T. ) ;
#79792 = CARTESIAN_POINT ( 'NONE',  ( -29.05897231630594035, -25.07799921448866343, 3.365375995075712279 ) ) ;
#79793 = CARTESIAN_POINT ( 'NONE',  ( -80.52287095715006160, -23.47593901973090169, -1.443836447538996648 ) ) ;
#79794 = CARTESIAN_POINT ( 'NONE',  ( -21.21068194950259311, 0.7780057951688260642, 11.49999999999998934 ) ) ;
#79795 = CARTESIAN_POINT ( 'NONE',  ( -91.62287095715004170, -29.50248528299804818, 1.056150453629040253 ) ) ;
#79796 = EDGE_CURVE ( 'NONE', #99590, #10228, #76830, .T. ) ;
#79797 = CARTESIAN_POINT ( 'NONE',  ( -30.64427850938830744, -23.56000036390796382, 11.50200000000000067 ) ) ;
#79798 = PLANE ( 'NONE',  #14569 ) ;
#79799 = CARTESIAN_POINT ( 'NONE',  ( -127.5562042904833930, -24.66019654487200441, 8.947790411086121054 ) ) ;
#79800 = CARTESIAN_POINT ( 'NONE',  ( -16.37229413335033001, -10.43475415037859655, -1.500000000000002220 ) ) ;
#79801 = CARTESIAN_POINT ( 'NONE',  ( -117.6242398451807389, -24.51419770103158768, 9.386484678747164523 ) ) ;
#79802 = EDGE_LOOP ( 'NONE', ( #9769, #86470, #25211, #51541 ) ) ;
#79803 = CARTESIAN_POINT ( 'NONE',  ( 10.93668938013857783, -16.14717738681254033, 11.49999999999999645 ) ) ;
#79804 = CARTESIAN_POINT ( 'NONE',  ( 31.62087157062645204, -4.386438359062696080, 26.73777224682022435 ) ) ;
#79805 = DIRECTION ( 'NONE',  ( 0.000000000000000000, 0.000000000000000000, 1.000000000000000000 ) ) ;
#79806 = ADVANCED_FACE ( 'NONE', ( #6275 ), #77268, .T. ) ;
#79807 = ORIENTED_EDGE ( 'NONE', *, *, #30242, .F. ) ;
#79808 = CARTESIAN_POINT ( 'NONE',  ( 4.465438306463536122, -5.876774720514425177, 21.59631214011467293 ) ) ;
#79809 = CARTESIAN_POINT ( 'NONE',  ( -89.54348968983181578, -24.65952944569304250, 1.056160979905700126 ) ) ;
#79810 = FACE_OUTER_BOUND ( 'NONE', #32869, .T. ) ;
#79811 = VECTOR ( 'NONE', #74094, 1000.000000000000114 ) ;
#79812 = CARTESIAN_POINT ( 'NONE',  ( -81.88534077628074215, -25.24813715446843432, 6.293942979331170307 ) ) ;
#79813 = CARTESIAN_POINT ( 'NONE',  ( -8.025172913017740939, -17.94849717234452768, -1.500000000000002220 ) ) ;
#79815 = ORIENTED_EDGE ( 'NONE', *, *, #30190, .F. ) ;
#79814 = CC_DESIGN_APPROVAL ( #28897, ( #96051 ) ) ;
#79816 = CARTESIAN_POINT ( 'NONE',  ( -8.022773894012710016, -10.23992600125390418, 1.310587897985993511 ) ) ;
#79817 = CARTESIAN_POINT ( 'NONE',  ( -20.32320236877023589, 10.94715076914730290, -1.500000000000002220 ) ) ;
#79818 = VECTOR ( 'NONE', #51763, 1000.000000000000000 ) ;
#79819 = PERSON_AND_ORGANIZATION_ROLE ( 'classification_officer' ) ;
#79820 = CARTESIAN_POINT ( 'NONE',  ( 3.094204744773375815, -6.376774720514422512, 21.02053020447315745 ) ) ;
#79821 = PLANE ( 'NONE',  #34469 ) ;
#79822 = CARTESIAN_POINT ( 'NONE',  ( -115.6228709571501270, -24.15516710230297193, 10.28746687063727094 ) ) ;
#79823 = FACE_OUTER_BOUND ( 'NONE', #36117, .T. ) ;
#79824 = CARTESIAN_POINT ( 'NONE',  ( -29.62287095715004881, -23.39678932012542845, -1.443836140311830940 ) ) ;
#79825 = CARTESIAN_POINT ( 'NONE',  ( 6.403846153846157740, -6.376774720514426065, 21.48076923076922995 ) ) ;
#79826 = FACE_OUTER_BOUND ( 'NONE', #83632, .T. ) ;
#79827 = AXIS2_PLACEMENT_3D ( 'NONE', #3668, #96006, #18875 ) ;
#79828 = FACE_OUTER_BOUND ( 'NONE', #52635, .T. ) ;
#79829 = CARTESIAN_POINT ( 'NONE',  ( -3.169371320753151977, 19.67850563098683736, -1.500000000000002220 ) ) ;
#79830 = CARTESIAN_POINT ( 'NONE',  ( -75.49319773296825531, -24.83644354573578994, 8.397322867130100121 ) ) ;
#79831 = CARTESIAN_POINT ( 'NONE',  ( 19.57267778704439820, -3.578973306870405047, -1.500000000000002220 ) ) ;
#79832 = VERTEX_POINT ( 'NONE', #37233 ) ;
#79833 = CARTESIAN_POINT ( 'NONE',  ( 3.797776442307698286, -5.876774720514427841, 21.83974358974358410 ) ) ;
#79834 = EDGE_CURVE ( 'NONE', #24959, #80860, #13824, .T. ) ;
#79835 = DIRECTION ( 'NONE',  ( 0.000000000000000000, 0.000000000000000000, 1.000000000000000000 ) ) ;
#79836 = DIRECTION ( 'NONE',  ( -3.773278334453079030E-23, 0.9999999999976377785, 2.173523156925979128E-06 ) ) ;
#79837 = CARTESIAN_POINT ( 'NONE',  ( 13.64113475014448440, -6.376774720514426953, -28.24100986136700087 ) ) ;
#79838 = CARTESIAN_POINT ( 'NONE',  ( -6.767879454864726974, -19.68250801024624508, 11.49999999999999645 ) ) ;
#79839 = CARTESIAN_POINT ( 'NONE',  ( -7.138063944469604571, -6.376774720514408301, 19.21974929698718881 ) ) ;
#79840 = EDGE_CURVE ( 'NONE', #45608, #75868, #15878, .T. ) ;
#79841 = CARTESIAN_POINT ( 'NONE',  ( 21.57151214508649772, 3.625915217019311583E-15, -2.299999999999999822 ) ) ;
#79842 = CARTESIAN_POINT ( 'NONE',  ( 19.47892149737544187, 11.75266795981601753, 11.49999999999999645 ) ) ;
#79843 = CIRCLE ( 'NONE', #63647, 24.00000000000000000 ) ;
#79844 = VERTEX_POINT ( 'NONE', #53963 ) ;
#79845 = B_SPLINE_SURFACE_WITH_KNOTS ( 'NONE', 3, 3, ( 
 ( #94070, #24556, #93063, #71247 ),
 ( #38785, #69746, #23544, #1736 ),
 ( #32675, #70242, #55532, #86462 ),
 ( #62641, #63651, #94574, #56033 ),
 ( #54521, #722, #86960, #85455 ),
 ( #15940, #17449, #40791, #48414 ),
 ( #77830, #8337, #39285, #79344 ) ),
 .UNSPECIFIED., .F., .F., .F.,
 ( 4, 3, 4 ),
 ( 4, 4 ),
 ( 0.0004766839783814058292, 0.1029713700210894145, 0.2054660560637974198 ),
 ( 0.6096490815589712398, 0.6109430970810473260 ),
 .UNSPECIFIED. ) ;
#79846 = CARTESIAN_POINT ( 'NONE',  ( -62.62287095715006302, -24.50216790748098816, 0.6166512839513665911 ) ) ;
#79847 = FACE_OUTER_BOUND ( 'NONE', #2297, .T. ) ;
#79848 = ORIENTED_EDGE ( 'NONE', *, *, #6099, .F. ) ;
#79849 = CARTESIAN_POINT ( 'NONE',  ( 19.72175082351460063, -4.362005935662174316, 11.49999999999998934 ) ) ;
#79850 = PLANE ( 'NONE',  #82523 ) ;
#79851 = DIRECTION ( 'NONE',  ( -3.773278334453079030E-23, 0.9999999999976377785, 2.173523156925979128E-06 ) ) ;
#79852 = VECTOR ( 'NONE', #41108, 1000.000000000000000 ) ;
#79853 = LINE ( 'NONE', #88483, #80084 ) ;
#79854 = ORIENTED_EDGE ( 'NONE', *, *, #30963, .T. ) ;
#79855 = CARTESIAN_POINT ( 'NONE',  ( -0.1426030150137701236, -21.20389190742571373, -1.497999999999532594 ) ) ;
#79856 = DIRECTION ( 'NONE',  ( 0.09824042138329590335, -0.9951627101165079203, -3.519298150595267883E-15 ) ) ;
#79857 = CARTESIAN_POINT ( 'NONE',  ( -14.99618758923778117, -13.25627519679515665, -1.500000000000002220 ) ) ;
#79858 = VECTOR ( 'NONE', #83436, 1000.000000000000114 ) ;
#79859 = CARTESIAN_POINT ( 'NONE',  ( 7.003190781191628744, -19.75400906848480176, 11.49999999999999645 ) ) ;
#79860 = CARTESIAN_POINT ( 'NONE',  ( -29.68423682549979148, -25.16578243805031789, 6.412434776996143171 ) ) ;
#79861 = CARTESIAN_POINT ( 'NONE',  ( 22.02124265030973760, -4.543225279485573864, 16.20402280011862217 ) ) ;
#79862 = CARTESIAN_POINT ( 'NONE',  ( 8.687672273659204691, 20.25853876245846408, -1.500000000000002220 ) ) ;
#79863 = EDGE_CURVE ( 'NONE', #75137, #23622, #17552, .T. ) ;
#79864 = CARTESIAN_POINT ( 'NONE',  ( -54.62287095715005592, -24.64965695001467694, 8.947790433994185832 ) ) ;
#79865 = ORIENTED_EDGE ( 'NONE', *, *, #20668, .F. ) ;
#79866 = DIRECTION ( 'NONE',  ( 0.000000000000000000, 1.000000000000000000, 0.000000000000000000 ) ) ;
#79867 = CARTESIAN_POINT ( 'NONE',  ( -49.50841769935764347, -25.18440252003702184, 3.984447925546727109 ) ) ;
#79868 = CARTESIAN_POINT ( 'NONE',  ( -72.54528880141759828, -24.34968618360933590, 0.1864209137778795600 ) ) ;
#79869 = EDGE_LOOP ( 'NONE', ( #67188, #30318, #47920, #74015 ) ) ;
#79870 = DIRECTION ( 'NONE',  ( 0.000000000000000000, 2.173523156925980399E-06, -0.9999999999976378895 ) ) ;
#79871 = VERTEX_POINT ( 'NONE', #31605 ) ;
#79872 = ORIENTED_EDGE ( 'NONE', *, *, #28380, .T. ) ;
#79873 = DIRECTION ( 'NONE',  ( -3.773278334453079030E-23, 0.9999999999976377785, 2.173523156925979128E-06 ) ) ;
#79874 = CARTESIAN_POINT ( 'NONE',  ( -101.2911250451791858, -25.27404695253231282, 3.130826079498485903 ) ) ;
#79875 = CARTESIAN_POINT ( 'NONE',  ( -58.62287095715007013, -23.96127896941631619, -0.6493128931037843721 ) ) ;
#79876 = CARTESIAN_POINT ( 'NONE',  ( -0.1859688948871585645, 20.53422428922035081, -1.500000000000002220 ) ) ;
#79877 = VERTEX_POINT ( 'NONE', #23473 ) ;
#79878 = CYLINDRICAL_SURFACE ( 'NONE', #70451, 1.399999999999998579 ) ;
#79879 = EDGE_CURVE ( 'NONE', #36769, #65212, #162, .T. ) ;
#79880 = CARTESIAN_POINT ( 'NONE',  ( -0.02075734969026423599, 6.475225279485573360, -28.54397719988136828 ) ) ;
#79881 = CARTESIAN_POINT ( 'NONE',  ( -64.52287095715006160, -23.47593901973090169, -1.443836447538996870 ) ) ;
#79882 = CARTESIAN_POINT ( 'NONE',  ( -22.28969446433750434, -1.297463027894488086, -1.500000000000002220 ) ) ;
#79884 = DIRECTION ( 'NONE',  ( -0.7071067811865474617, 0.000000000000000000, -0.7071067811865474617 ) ) ;
#79883 = VECTOR ( 'NONE', #3474, 1000.000000000000000 ) ;
#79885 = DIRECTION ( 'NONE',  ( -0.000000000000000000, -1.000000000000000000, 0.000000000000000000 ) ) ;
#79886 = ORIENTED_EDGE ( 'NONE', *, *, #74513, .F. ) ;
#79887 = CARTESIAN_POINT ( 'NONE',  ( -42.62287095715003460, -24.33832256526968507, 0.1851278514119854834 ) ) ;
#79888 = CARTESIAN_POINT ( 'NONE',  ( -63.62287095715003460, -23.48783264082478084, -1.443836473390069042 ) ) ;
#79889 = LOCAL_TIME ( 0, 54, 15.00000000000000000, #67870 ) ;
#79890 = CARTESIAN_POINT ( 'NONE',  ( 18.01467621842780176, -10.50282939286117667, 11.49999999999998934 ) ) ;
#79891 = ORIENTED_EDGE ( 'NONE', *, *, #72579, .T. ) ;
#79893 = VERTEX_POINT ( 'NONE', #8275 ) ;
#79892 = CARTESIAN_POINT ( 'NONE',  ( -52.52287095715007581, -24.51283580621455727, 0.6167428607047122924 ) ) ;
#79894 = ORIENTED_EDGE ( 'NONE', *, *, #28693, .T. ) ;
#79895 = AXIS2_PLACEMENT_3D ( 'NONE', #34916, #97313, #66384 ) ;
#79896 = CARTESIAN_POINT ( 'NONE',  ( -69.33560399441930144, -25.25935264438429684, 7.166139204845690003 ) ) ;
#79897 = CARTESIAN_POINT ( 'NONE',  ( 21.00884048613226440, 1.293913838035418040, -1.500000000000002220 ) ) ;
#79898 = EDGE_LOOP ( 'NONE', ( #99607, #49347, #51105, #90482 ) ) ;
#79899 = CARTESIAN_POINT ( 'NONE',  ( -69.52287095715006160, -23.48786465467241058, 11.44779295918254647 ) ) ;
#79900 = CARTESIAN_POINT ( 'NONE',  ( 26.73860345374794534, 1.477225279485574028, 3.440769881205036427E-15 ) ) ;
#79901 = CARTESIAN_POINT ( 'NONE',  ( -120.6237998820897843, -24.92592662359561118, 8.075495903017998245 ) ) ;
#79902 = B_SPLINE_CURVE_WITH_KNOTS ( 'NONE', 3,
 ( #30744, #77900, #77402, #54591, #37371, #22118 ),
 .UNSPECIFIED., .F., .F.,
 ( 4, 2, 4 ),
 ( 6.391158118973930141E-06, 0.001387004593080795036, 0.002767618028042615873 ),
 .UNSPECIFIED. ) ;
#79903 = CIRCLE ( 'NONE', #15076, 1.836000000000000743 ) ;
#79904 = CARTESIAN_POINT ( 'NONE',  ( -101.1119640259560271, -25.03152421035094832, 7.433728220542129783 ) ) ;
#79905 = EDGE_CURVE ( 'NONE', #41375, #97248, #35708, .T. ) ;
#79906 = CARTESIAN_POINT ( 'NONE',  ( -59.56671735520578892, -23.48783264082476308, -1.443836473390097908 ) ) ;
#79907 = CARTESIAN_POINT ( 'NONE',  ( -21.63489631200954122, -1.325961216813365429, -1.500000000000002220 ) ) ;
#79908 = DIRECTION ( 'NONE',  ( -7.163199596004101480E-14, 1.000000000000000000, 7.440411327181627631E-14 ) ) ;
#79909 = ADVANCED_FACE ( 'NONE', ( #14876 ), #70173, .T. ) ;
#79911 = VERTEX_POINT ( 'NONE', #91010 ) ;
#79910 = CARTESIAN_POINT ( 'NONE',  ( -2.380169663812839342, 22.11153957539610104, 11.49999999999999645 ) ) ;
#79912 = CARTESIAN_POINT ( 'NONE',  ( -5.366453405989236813, 2.939152317953647894E-15, -24.00000000000000000 ) ) ;
#79913 = DIRECTION ( 'NONE',  ( 1.797729424027682620E-15, 1.000000000000000000, 1.064096645546785541E-13 ) ) ;
#79914 = VERTEX_POINT ( 'NONE', #1673 ) ;
#79916 = ORIENTED_EDGE ( 'NONE', *, *, #83583, .F. ) ;
#79915 = CARTESIAN_POINT ( 'NONE',  ( -118.6228709571500559, -24.64965695001469115, 8.947790433994175174 ) ) ;
#79917 = VERTEX_POINT ( 'NONE', #41746 ) ;
#79918 = CYLINDRICAL_SURFACE ( 'NONE', #28681, 1.000000000000000000 ) ;
#79919 = EDGE_CURVE ( 'NONE', #39840, #24258, #38836, .T. ) ;
#79920 = CARTESIAN_POINT ( 'NONE',  ( 1.109688723463823301, -20.12803150795971874, -1.500000000000002220 ) ) ;
#79921 = EDGE_CURVE ( 'NONE', #47216, #20204, #68307, .T. ) ;
#79922 = CARTESIAN_POINT ( 'NONE',  ( 14.76093561896379214, -5.965225279485572685, -26.55548769130089681 ) ) ;
#79923 = ORIENTED_EDGE ( 'NONE', *, *, #14540, .T. ) ;
#79924 = CARTESIAN_POINT ( 'NONE',  ( -130.5728709571500303, -24.13533882933943175, 10.52299274931600337 ) ) ;
#79925 = CARTESIAN_POINT ( 'NONE',  ( -9.774569144048079750, -20.17623354167628946, -1.500000000000002220 ) ) ;
#79926 = ADVANCED_FACE ( 'NONE', ( #54959 ), #2182, .T. ) ;
#79927 = ORIENTED_EDGE ( 'NONE', *, *, #40955, .T. ) ;
#79928 = EDGE_LOOP ( 'NONE', ( #28482, #89136, #93957, #84291 ) ) ;
#79929 = FACE_OUTER_BOUND ( 'NONE', #79011, .T. ) ;
#79931 = CARTESIAN_POINT ( 'NONE',  ( 3.509873074917118085, 5.965225279485572685, 29.15869884040363758 ) ) ;
#79930 = CIRCLE ( 'NONE', #13435, 1.249999999999997558 ) ;
#79932 = FACE_OUTER_BOUND ( 'NONE', #22387, .T. ) ;
#79933 = CARTESIAN_POINT ( 'NONE',  ( 30.32108885906865936, 6.376774720514426953, 3.274824222184972822 ) ) ;
#79934 = EDGE_CURVE ( 'NONE', #89410, #63331, #64599, .T. ) ;
#79935 = CARTESIAN_POINT ( 'NONE',  ( -97.23961491194229723, -25.30559561715418226, 6.147794833475641596 ) ) ;
#79936 = CARTESIAN_POINT ( 'NONE',  ( -10.82925958622295859, 16.30987832687952022, -1.500000000000002220 ) ) ;
#79937 = B_SPLINE_CURVE_WITH_KNOTS ( 'NONE', 3,
 ( #41138, #88809, #49758, #71586, #34518, #87804 ),
 .UNSPECIFIED., .F., .F.,
 ( 4, 2, 4 ),
 ( 0.000000000000000000, 0.0002343639316654294483, 0.0004687278633308588965 ),
 .UNSPECIFIED. ) ;
#79938 = CIRCLE ( 'NONE', #68570, 2.249999999999998668 ) ;
#79939 = CARTESIAN_POINT ( 'NONE',  ( -57.62287095715004881, -29.50248528299804818, 1.056150453629034924 ) ) ;
#79940 = ORIENTED_EDGE ( 'NONE', *, *, #84721, .T. ) ;
#79941 = CARTESIAN_POINT ( 'NONE',  ( -20.54356019850136050, 6.435454313062578535, -1.500000000000002220 ) ) ;
#79942 = DIRECTION ( 'NONE',  ( 0.000000000000000000, 0.000000000000000000, -1.000000000000000000 ) ) ;
#79944 = CARTESIAN_POINT ( 'NONE',  ( -114.5228709571500758, -23.47593901973090524, -1.443836447538996204 ) ) ;
#79943 = B_SPLINE_CURVE_WITH_KNOTS ( 'NONE', 3,
 ( #90879, #74651, #81273, #13244, #73664, #4658 ),
 .UNSPECIFIED., .F., .F.,
 ( 4, 2, 4 ),
 ( 0.000000000000000000, 0.001380901958385391580, 0.002761803916770783161 ),
 .UNSPECIFIED. ) ;
#79945 = CARTESIAN_POINT ( 'NONE',  ( -123.5228709571500190, -23.73934037231757443, 11.05740245334327732 ) ) ;
#79947 = B_SPLINE_CURVE_WITH_KNOTS ( 'NONE', 3,
 ( #40536, #94804, #31914, #79582 ),
 .UNSPECIFIED., .F., .F.,
 ( 4, 4 ),
 ( 2.775557561562891351E-17, 0.0001000000000000167286 ),
 .UNSPECIFIED. ) ;
#79946 = DIRECTION ( 'NONE',  ( -3.773278334444167608E-23, 1.000000000000000000, 0.000000000000000000 ) ) ;
#79948 = CARTESIAN_POINT ( 'NONE',  ( -19.87571804785047647, -11.42512898079034400, -1.500000000000002220 ) ) ;
#79949 = MECHANICAL_CONTEXT ( 'NONE', #7717, 'mechanical' ) ;
#79950 = LINE ( 'NONE', #73350, #71006 ) ;
#79951 = CARTESIAN_POINT ( 'NONE',  ( -53.54760685552204080, -24.15543982623906771, -0.2315651400026670914 ) ) ;
#79952 = CARTESIAN_POINT ( 'NONE',  ( 8.649182803842551337, -18.14983140373652404, 11.49999999999999645 ) ) ;
#79953 = CARTESIAN_POINT ( 'NONE',  ( -40.55620429048338593, -25.00182538069145011, 7.747789668545099317 ) ) ;
#79954 = CARTESIAN_POINT ( 'NONE',  ( -31.52287095715007581, -23.96127896942127933, -0.6493128930940336163 ) ) ;
#79955 = CARTESIAN_POINT ( 'NONE',  ( 14.76093561896379214, 3.316774720514426456, -26.55548769130089681 ) ) ;
#79956 = CARTESIAN_POINT ( 'NONE',  ( -102.6228709571500559, -24.64898659630368272, 1.056161002820829697 ) ) ;
#79957 = CARTESIAN_POINT ( 'NONE',  ( -82.52287095715006160, -23.47596703998600631, 11.44779298504228571 ) ) ;
#79958 = CARTESIAN_POINT ( 'NONE',  ( 17.59243620335545799, -9.192777620008959261, 11.49999999999998934 ) ) ;
#79959 = DIRECTION ( 'NONE',  ( -0.000000000000000000, 1.000000000000000000, -0.000000000000000000 ) ) ;
#79960 = CARTESIAN_POINT ( 'NONE',  ( -16.89733858281218204, -10.06102416988892934, -1.500000000000002220 ) ) ;
#79961 = CARTESIAN_POINT ( 'NONE',  ( -42.54640892709206668, -24.15543982623907127, -0.2315651400026575435 ) ) ;
#79962 = VECTOR ( 'NONE', #66888, 1000.000000000000227 ) ;
#79963 = DIRECTION ( 'NONE',  ( -0.8264557562326033668, -6.845827386180409975E-16, -0.5630016722799281448 ) ) ;
#79964 = COORDINATED_UNIVERSAL_TIME_OFFSET ( 0, 0, .AHEAD. ) ;
#79965 = CARTESIAN_POINT ( 'NONE',  ( 15.31892417638225012, 3.658177093025726023, -28.50911884272268182 ) ) ;
#79966 = CARTESIAN_POINT ( 'NONE',  ( -39.11375990658831370, -25.30200599664514982, 4.685637363869906480 ) ) ;
#79967 = CARTESIAN_POINT ( 'NONE',  ( 20.62939718826500979, -0.8834638802319035866, 11.49999999999999645 ) ) ;
#79968 = PLANE ( 'NONE',  #99143 ) ;
#79969 = DIRECTION ( 'NONE',  ( 0.000000000000000000, -0.000000000000000000, -1.000000000000000000 ) ) ;
#79970 = VECTOR ( 'NONE', #52605, 1000.000000000000114 ) ;
#79972 = EDGE_CURVE ( 'NONE', #80402, #5790, #86895, .T. ) ;
#79971 = CARTESIAN_POINT ( 'NONE',  ( 2.010693963185784749, 22.50221635003889276, 11.49999999999999645 ) ) ;
#79973 = VERTEX_POINT ( 'NONE', #33617 ) ;
#79974 = CARTESIAN_POINT ( 'NONE',  ( -69.56233234027952506, -25.25639530571745439, 6.775360290800271912 ) ) ;
#79975 = CARTESIAN_POINT ( 'NONE',  ( 30.64109438017208120, 3.316774720514426456, 28.31981406664616330 ) ) ;
#79976 = CARTESIAN_POINT ( 'NONE',  ( -72.62287095715004170, -24.50321055353805377, 9.387540953477529371 ) ) ;
#79977 = VECTOR ( 'NONE', #1578, 1000.000000000000227 ) ;
#79978 = CARTESIAN_POINT ( 'NONE',  ( -110.5228709571500474, -24.15431212366389957, -0.2830839119429225947 ) ) ;
#79979 = CARTESIAN_POINT ( 'NONE',  ( -41.26959558397305727, -29.50249893827660941, 7.338705366995167623 ) ) ;
#79980 = ORIENTED_EDGE ( 'NONE', *, *, #62758, .T. ) ;
#79981 = CARTESIAN_POINT ( 'NONE',  ( -79.89247415061277025, -25.31596245313187055, 5.073623374384617968 ) ) ;
#79982 = CARTESIAN_POINT ( 'NONE',  ( -21.19308438721250099, -8.479022899233653376, -1.500000000000002220 ) ) ;
#79983 = DIRECTION ( 'NONE',  ( 1.000000000000000000, 3.773278334444167608E-23, 8.201307833595939069E-29 ) ) ;
#79984 = DIRECTION ( 'NONE',  ( -3.773278334453079618E-23, 0.9999999999976377785, 2.173523156925979975E-06 ) ) ;
#79985 = CARTESIAN_POINT ( 'NONE',  ( -63.50463970142624959, -24.15620529776628089, 10.23563542870660470 ) ) ;
#79986 = B_SPLINE_CURVE_WITH_KNOTS ( 'NONE', 3,
 ( #24152, #32768, #33265, #62744 ),
 .UNSPECIFIED., .F., .F.,
 ( 4, 4 ),
 ( 0.000000000000000000, 1.000000000000000000 ),
 .UNSPECIFIED. ) ;
#79987 = CARTESIAN_POINT ( 'NONE',  ( -21.66288588771858770, -5.991481186202806342, 11.49999999999999645 ) ) ;
#79988 = ORIENTED_EDGE ( 'NONE', *, *, #70685, .T. ) ;
#79989 = CARTESIAN_POINT ( 'NONE',  ( -43.52946602040498902, -24.65952944569304606, 1.056160979905694131 ) ) ;
#79990 = CARTESIAN_POINT ( 'NONE',  ( 7.969717912702302343, -20.46423023992739942, -1.500000000000002220 ) ) ;
#79991 = CARTESIAN_POINT ( 'NONE',  ( -54.62287095715007013, -23.96127896941632685, -0.6493128931037892571 ) ) ;
#79992 = ADVANCED_FACE ( 'NONE', ( #78267 ), #40231, .T. ) ;
#79993 = PLANE ( 'NONE',  #75413 ) ;
#79994 = DIRECTION ( 'NONE',  ( 2.352173255807804438E-16, -2.352173255807796056E-16, -1.000000000000000000 ) ) ;
#79995 = EDGE_LOOP ( 'NONE', ( #92125, #20734, #69919, #36122 ) ) ;
#79996 = CARTESIAN_POINT ( 'NONE',  ( -92.52287095715006160, -24.64898659630529210, 1.056161002820827921 ) ) ;
#79997 = DIRECTION ( 'NONE',  ( 0.9975640502598241977, -0.06975647374412546897, -0.000000000000000000 ) ) ;
#79998 = VERTEX_POINT ( 'NONE', #32611 ) ;
#79999 = CARTESIAN_POINT ( 'NONE',  ( -54.54194454780496670, -24.35071581493543391, 9.817618358456034144 ) ) ;
#80000 = CARTESIAN_POINT ( 'NONE',  ( 3.385237411341575964, -20.22741857368478335, -1.500000000000002220 ) ) ;
#80001 = ORIENTED_EDGE ( 'NONE', *, *, #81643, .T. ) ;
#80002 = ORIENTED_EDGE ( 'NONE', *, *, #98334, .F. ) ;
#80003 = VERTEX_POINT ( 'NONE', #40727 ) ;
#80004 = ORIENTED_EDGE ( 'NONE', *, *, #54162, .F. ) ;
#80005 = CARTESIAN_POINT ( 'NONE',  ( -84.62287095715004170, -24.65952944569304606, 1.056160979905699460 ) ) ;
#80006 = CARTESIAN_POINT ( 'NONE',  ( 14.65057173600216345, 17.85730367728733725, -1.500000000000002220 ) ) ;
#80007 = CARTESIAN_POINT ( 'NONE',  ( -104.5872714728782711, -24.51419770103158768, 9.386484678747164523 ) ) ;
#80008 = CARTESIAN_POINT ( 'NONE',  ( -20.32544160278596834, -1.370942541838689799, -1.500000000000002220 ) ) ;
#80009 = AXIS2_PLACEMENT_3D ( 'NONE', #68191, #61085, #99118 ) ;
#80010 = ORIENTED_EDGE ( 'NONE', *, *, #18417, .T. ) ;
#80011 = CARTESIAN_POINT ( 'NONE',  ( -71.70008735307283132, -25.22833616190947126, 6.373748403976279064 ) ) ;
#80012 = EDGE_CURVE ( 'NONE', #86729, #50770, #63477, .T. ) ;
#80013 = CARTESIAN_POINT ( 'NONE',  ( -88.62287095715004170, -24.34917612406838217, 0.1852690917426653427 ) ) ;
#80014 = ADVANCED_FACE ( 'NONE', ( #8778 ), #10277, .T. ) ;
#80015 = PLANE ( 'NONE',  #28676 ) ;
#80016 = LINE ( 'NONE', #49086, #61020 ) ;
#80017 = VERTEX_POINT ( 'NONE', #47844 ) ;
#80018 = CARTESIAN_POINT ( 'NONE',  ( -101.6228709571500559, -29.50247984919015209, -1.443849546365050029 ) ) ;
#80020 = VECTOR ( 'NONE', #72458, 1000.000000000000000 ) ;
#80019 = CARTESIAN_POINT ( 'NONE',  ( -49.10641598061040725, -25.31573638291652273, 4.048599298564869109 ) ) ;
#80021 = ADVANCED_FACE ( 'NONE', ( #41234 ), #9266, .F. ) ;
#80022 = ORIENTED_EDGE ( 'NONE', *, *, #28187, .F. ) ;
#80023 = CARTESIAN_POINT ( 'NONE',  ( -12.88759680649768136, 16.30154091734715749, -1.500000000000002220 ) ) ;
#80024 = ORIENTED_EDGE ( 'NONE', *, *, #87345, .F. ) ;
#80026 = ORIENTED_EDGE ( 'NONE', *, *, #71886, .T. ) ;
#80025 = DIRECTION ( 'NONE',  ( -1.000000000000000000, -3.773278334444166432E-23, -8.201307841325785021E-29 ) ) ;
#80027 = B_SPLINE_CURVE_WITH_KNOTS ( 'NONE', 3,
 ( #87018, #81413, #34244, #48474 ),
 .UNSPECIFIED., .F., .F.,
 ( 4, 4 ),
 ( 0.000000000000000000, 9.999999999998897304E-05 ),
 .UNSPECIFIED. ) ;
#80028 = DIRECTION ( 'NONE',  ( 0.000000000000000000, 2.173523156925980399E-06, -0.9999999999976378895 ) ) ;
#80029 = CARTESIAN_POINT ( 'NONE',  ( -97.52287095715009002, -23.96177878511308990, 10.65340807706329329 ) ) ;
#80030 = ORIENTED_EDGE ( 'NONE', *, *, #47278, .F. ) ;
#80031 = ORIENTED_EDGE ( 'NONE', *, *, #36786, .F. ) ;
#80032 = B_SPLINE_CURVE_WITH_KNOTS ( 'NONE', 3,
 ( #50520, #56149, #50037, #95696, #79466, #34801, #96203, #80970 ),
 .UNSPECIFIED., .F., .F.,
 ( 4, 2, 2, 4 ),
 ( 0.000000000000000000, 0.002001098010032798143, 0.003001647015049197214, 0.004002196020065596285 ),
 .UNSPECIFIED. ) ;
#80033 = DIRECTION ( 'NONE',  ( -0.000000000000000000, -1.000000000000000000, 0.000000000000000000 ) ) ;
#80034 = DIRECTION ( 'NONE',  ( -3.773278334444166432E-23, 1.000000000000000000, 0.000000000000000000 ) ) ;
#80035 = CARTESIAN_POINT ( 'NONE',  ( -78.52287095715006160, -23.47593901973090169, -1.443836447538996648 ) ) ;
#80036 = ADVANCED_FACE ( 'NONE', ( #56473, #79279 ), #48855, .T. ) ;
#80038 = ORIENTED_EDGE ( 'NONE', *, *, #76059, .T. ) ;
#80037 = CARTESIAN_POINT ( 'NONE',  ( -19.11006845027251799, 11.06304553819242642, 11.49999999999999645 ) ) ;
#80039 = CARTESIAN_POINT ( 'NONE',  ( -49.16102892102028932, -25.15009172915296887, 7.003546792922761277 ) ) ;
#80040 = CARTESIAN_POINT ( 'NONE',  ( -22.11960324842224423, 4.537628740662121629, -1.500000000000002220 ) ) ;
#80042 = ORIENTED_EDGE ( 'NONE', *, *, #53796, .T. ) ;
#80041 = DIRECTION ( 'NONE',  ( 0.000000000000000000, 0.9999999999976377785, 2.173523156925979975E-06 ) ) ;
#80043 = ORIENTED_EDGE ( 'NONE', *, *, #95707, .F. ) ;
#80044 = FACE_OUTER_BOUND ( 'NONE', #1308, .T. ) ;
#80045 = EDGE_CURVE ( 'NONE', #72031, #17423, #79780, .T. ) ;
#80046 = EDGE_CURVE ( 'NONE', #94222, #35033, #90161, .T. ) ;
#80047 = DIRECTION ( 'NONE',  ( 0.000000000000000000, 0.000000000000000000, -1.000000000000000000 ) ) ;
#80048 = ORIENTED_EDGE ( 'NONE', *, *, #30397, .T. ) ;
#80049 = CARTESIAN_POINT ( 'NONE',  ( -14.54676392617323266, -15.37779485849079464, -1.500000000000002220 ) ) ;
#80050 = DIRECTION ( 'NONE',  ( -1.000000000000000000, 0.000000000000000000, -0.000000000000000000 ) ) ;
#80051 = CARTESIAN_POINT ( 'NONE',  ( 30.58729439590573662, -5.356774720514427379, 26.14186284044631492 ) ) ;
#80052 = CARTESIAN_POINT ( 'NONE',  ( -7.282824509310913186, -5.876774720514415407, 19.84584863393302356 ) ) ;
#80053 = PLANE ( 'NONE',  #55144 ) ;
#80054 = CARTESIAN_POINT ( 'NONE',  ( -2.380169663812839342, 22.11153957539610104, -1.500000000000002220 ) ) ;
#80055 = CARTESIAN_POINT ( 'NONE',  ( -114.5554611002867773, -23.96119346886881374, -0.6495511937831859317 ) ) ;
#80056 = EDGE_CURVE ( 'NONE', #1389, #77260, #57474, .T. ) ;
#80057 = ORIENTED_EDGE ( 'NONE', *, *, #50244, .T. ) ;
#80058 = CARTESIAN_POINT ( 'NONE',  ( -5.439936175300728927, -6.376774720514410077, 19.67454710845353816 ) ) ;
#80059 = CARTESIAN_POINT ( 'NONE',  ( -37.48487686491367299, -24.51314013834316796, 0.6176544820404176184 ) ) ;
#80060 = CARTESIAN_POINT ( 'NONE',  ( -5.977879402576776968, -18.46583800616800630, 11.49999999999999645 ) ) ;
#80061 = EDGE_CURVE ( 'NONE', #90955, #4409, #49863, .T. ) ;
#80062 = CARTESIAN_POINT ( 'NONE',  ( -41.68476140872422775, -25.21340872514199916, 3.506346521580342213 ) ) ;
#80063 = CARTESIAN_POINT ( 'NONE',  ( -8.160000000000000142, -9.123836073446797812, -2.666350264951732552 ) ) ;
#80064 = B_SPLINE_CURVE_WITH_KNOTS ( 'NONE', 3,
 ( #91295, #21764, #52738, #60862, #83677, #14159 ),
 .UNSPECIFIED., .F., .F.,
 ( 4, 2, 4 ),
 ( 1.570887131794952276E-05, 0.001396322306279765193, 0.002776935741241580609 ),
 .UNSPECIFIED. ) ;
#80065 = EDGE_CURVE ( 'NONE', #58859, #497, #58467, .T. ) ;
#80066 = CARTESIAN_POINT ( 'NONE',  ( -18.70048401425367501, 5.426029767813830063, -1.500000000000002220 ) ) ;
#80067 = CARTESIAN_POINT ( 'NONE',  ( -9.048234560742015375, 19.43086790383670603, 11.49999999999998934 ) ) ;
#80068 = CARTESIAN_POINT ( 'NONE',  ( -56.62287095715005592, -23.48786465467241413, 11.44779295918254824 ) ) ;
#80069 = CARTESIAN_POINT ( 'NONE',  ( -26.98755670591954114, -24.57999526489839326, 1.764415294430758507 ) ) ;
#80070 = FACE_OUTER_BOUND ( 'NONE', #29191, .T. ) ;
#80071 = CARTESIAN_POINT ( 'NONE',  ( -123.6228709571500559, -23.47596703998600631, 11.44779298504227860 ) ) ;
#80072 = CARTESIAN_POINT ( 'NONE',  ( -22.72798930328562150, -0.2126449523330483371, -1.500000000000002220 ) ) ;
#80073 = EDGE_CURVE ( 'NONE', #26998, #15184, #40456, .T. ) ;
#80074 = DIRECTION ( 'NONE',  ( -1.000000000000000000, -4.023591475097605070E-15, 1.444818008257218650E-16 ) ) ;
#80075 = CARTESIAN_POINT ( 'NONE',  ( -54.52287095715006870, -29.50250243563736774, 8.947779886222146928 ) ) ;
#80076 = DIRECTION ( 'NONE',  ( -0.000000000000000000, 1.000000000000000000, -0.000000000000000000 ) ) ;
#80077 = CARTESIAN_POINT ( 'NONE',  ( 11.38277053702107899, 16.36964821499295653, 11.49999999999999645 ) ) ;
#80078 = CARTESIAN_POINT ( 'NONE',  ( -104.5531608873337035, -24.15543982623907482, -0.2315651400026580709 ) ) ;
#80079 = CARTESIAN_POINT ( 'NONE',  ( -39.55295621575191234, -23.96169478059712787, 10.65365249895718769 ) ) ;
#80080 = CARTESIAN_POINT ( 'NONE',  ( -31.52287095715006160, -29.50248528299804818, 1.056150453629029817 ) ) ;
#80081 = ORIENTED_EDGE ( 'NONE', *, *, #14933, .F. ) ;
#80082 = DIRECTION ( 'NONE',  ( 0.000000000000000000, 0.000000000000000000, -1.000000000000000000 ) ) ;
#80083 = CARTESIAN_POINT ( 'NONE',  ( -32.99705628988545669, -25.31516574674648368, 3.894478520810415567 ) ) ;
#80084 = VECTOR ( 'NONE', #15582, 1000.000000000000227 ) ;
#80085 = CARTESIAN_POINT ( 'NONE',  ( -18.45943378446990835, 11.37049804852326140, 11.49999999999998934 ) ) ;
#80086 = DIRECTION ( 'NONE',  ( 3.773278334444167608E-23, -1.000000000000000000, 0.000000000000000000 ) ) ;
#80087 = CARTESIAN_POINT ( 'NONE',  ( -19.44331071757236273, 1.017868325215548708, -1.500000000000002220 ) ) ;
#80088 = CARTESIAN_POINT ( 'NONE',  ( -125.5228709571500616, -29.50249982740957577, 7.747779886224967605 ) ) ;
#80089 = ORIENTED_EDGE ( 'NONE', *, *, #11038, .F. ) ;
#80090 = VECTOR ( 'NONE', #67661, 1000.000000000000000 ) ;
#80091 = DIRECTION ( 'NONE',  ( -3.773278334444167608E-23, 1.000000000000000000, 0.000000000000000000 ) ) ;
#80092 = CARTESIAN_POINT ( 'NONE',  ( 20.35601985306173134, -1.938729116259007679, 11.49999999999999645 ) ) ;
#80093 = CARTESIAN_POINT ( 'NONE',  ( -110.6228709571500701, -23.48783264082479505, -1.443836473390060160 ) ) ;
#80094 = CARTESIAN_POINT ( 'NONE',  ( -118.6228709571500701, -23.96127896941633040, -0.6493128931037773777 ) ) ;
#80095 = ORIENTED_EDGE ( 'NONE', *, *, #82572, .T. ) ;
#80096 = FACE_OUTER_BOUND ( 'NONE', #81292, .T. ) ;
#80097 = CARTESIAN_POINT ( 'NONE',  ( 33.50227909998848475, 4.005981270903656188, -11.48786002470558643 ) ) ;
#80098 = CARTESIAN_POINT ( 'NONE',  ( 7.234974673537251100, -6.376774720514415407, 19.99114326857715795 ) ) ;
#80099 = CARTESIAN_POINT ( 'NONE',  ( -49.27764846858840997, -25.26180677598144086, 6.145204968850301874 ) ) ;
#80100 = CARTESIAN_POINT ( 'NONE',  ( -129.5895376238166818, -23.48783264082478794, -1.443836473390056607 ) ) ;
#80101 = B_SPLINE_CURVE_WITH_KNOTS ( 'NONE', 3,
 ( #9740, #39181, #93967, #10238 ),
 .UNSPECIFIED., .F., .F.,
 ( 4, 4 ),
 ( 0.000000000000000000, 9.999999999998897304E-05 ),
 .UNSPECIFIED. ) ;
#80102 = DIRECTION ( 'NONE',  ( -3.773278334453079618E-23, 0.9999999999976377785, 2.173523156925979975E-06 ) ) ;
#80103 = VERTEX_POINT ( 'NONE', #27005 ) ;
#80104 = CARTESIAN_POINT ( 'NONE',  ( -66.64658286559381395, -23.73791477778911840, 11.05961554403170766 ) ) ;
#80105 = CARTESIAN_POINT ( 'NONE',  ( -12.88233675513024856, -19.01995677650982230, 11.49999999999999645 ) ) ;
#80106 = CARTESIAN_POINT ( 'NONE',  ( 12.47407908559008760, -19.03963781694049473, -1.500000000000002220 ) ) ;
#80107 = CARTESIAN_POINT ( 'NONE',  ( -110.5871102190748729, -24.83644354573579349, 8.397322867130096569 ) ) ;
#80108 = CARTESIAN_POINT ( 'NONE',  ( -98.52287095715006160, -23.48783264082477018, -1.443836473390087916 ) ) ;
#80109 = CARTESIAN_POINT ( 'NONE',  ( -90.49972952456502640, -24.92564183028978775, 1.928384488918253092 ) ) ;
#80110 = CARTESIAN_POINT ( 'NONE',  ( -70.52287095715009002, -23.85196035786899671, -0.8779234886475163480 ) ) ;
#80111 = CARTESIAN_POINT ( 'NONE',  ( -82.58953762381672448, -23.48783264082478084, -1.443836473390065933 ) ) ;
#80112 = CARTESIAN_POINT ( 'NONE',  ( 3.414333255021221092, 21.62243999391013105, -1.500000000000002220 ) ) ;
#80113 = CARTESIAN_POINT ( 'NONE',  ( 32.53135143123563466, 0.3587747205144265483, 6.926385399448451885 ) ) ;
#80114 = ADVANCED_FACE ( 'NONE', ( #88911 ), #96509, .F. ) ;
#80115 = CARTESIAN_POINT ( 'NONE',  ( -115.6228709571500701, -24.15431212366392089, -0.2830839119429090500 ) ) ;
#80116 = CARTESIAN_POINT ( 'NONE',  ( -71.33443329732202187, -25.30573833935151740, 5.086063791536371781 ) ) ;
#80117 = CARTESIAN_POINT ( 'NONE',  ( -98.99594346619821295, -25.31200630955432018, 5.589963903709685766 ) ) ;
#80118 = ORIENTED_EDGE ( 'NONE', *, *, #29148, .T. ) ;
#80119 = EDGE_CURVE ( 'NONE', #14495, #82155, #16168, .T. ) ;
#80120 = CARTESIAN_POINT ( 'NONE',  ( -19.81292649638395531, 4.959676026661640869, -1.500000000000002220 ) ) ;
#80121 = ORIENTED_EDGE ( 'NONE', *, *, #78480, .F. ) ;
#80122 = B_SPLINE_CURVE_WITH_KNOTS ( 'NONE', 3,
 ( #16207, #68999, #39552, #60903 ),
 .UNSPECIFIED., .F., .F.,
 ( 4, 4 ),
 ( 0.000000000000000000, 1.000000000000000000 ),
 .UNSPECIFIED. ) ;
#80123 = ORIENTED_EDGE ( 'NONE', *, *, #55861, .F. ) ;
#80124 = CARTESIAN_POINT ( 'NONE',  ( -11.53412672884717871, -19.92380006517282709, -1.500000000000002220 ) ) ;
#80125 = FACE_OUTER_BOUND ( 'NONE', #92016, .T. ) ;
#80126 = ADVANCED_FACE ( 'NONE', ( #5162 ), #44234, .F. ) ;
#80127 = ORIENTED_EDGE ( 'NONE', *, *, #2367, .F. ) ;
#80128 = CARTESIAN_POINT ( 'NONE',  ( -101.5562042904833930, -24.65952944569304606, 1.056160979905701236 ) ) ;
#80129 = ADVANCED_FACE ( 'NONE', ( #73187 ), #24025, .T. ) ;
#80130 = CARTESIAN_POINT ( 'NONE',  ( 30.53060340732036337, 1.682774720514426114, 3.744237563515920634E-15 ) ) ;
#80131 = EDGE_CURVE ( 'NONE', #68269, #49130, #24732, .T. ) ;
#80132 = CARTESIAN_POINT ( 'NONE',  ( -9.749999999999984013, 18.74999999999999645, 0.000000000000000000 ) ) ;
#80133 = CARTESIAN_POINT ( 'NONE',  ( 10.24059822343752479, -5.876774720514426953, -2.394817856121274864E-14 ) ) ;
#80135 = ORIENTED_EDGE ( 'NONE', *, *, #75428, .F. ) ;
#80134 = CARTESIAN_POINT ( 'NONE',  ( -21.04715019690976874, -3.721878931196799467, 11.49999999999999645 ) ) ;
#80136 = EDGE_CURVE ( 'NONE', #28190, #52365, #44727, .T. ) ;
#80137 = EDGE_LOOP ( 'NONE', ( #18227, #71564, #70787, #74016 ) ) ;
#80138 = CARTESIAN_POINT ( 'NONE',  ( 2.725811458822067657, 22.07344620009914138, -1.500000000000002220 ) ) ;
#80139 = CARTESIAN_POINT ( 'NONE',  ( 9.361532043782798240, 18.45020211870636118, -1.500000000000002220 ) ) ;
#80140 = AXIS2_PLACEMENT_3D ( 'NONE', #23802, #100408, #69983 ) ;
#80141 = B_SPLINE_CURVE_WITH_KNOTS ( 'NONE', 3,
 ( #25621, #25108, #55586, #62701, #93617, #71303, #46965, #87527 ),
 .UNSPECIFIED., .F., .F.,
 ( 4, 2, 2, 4 ),
 ( 0.000000000000000000, 0.002001098010032802479, 0.003001647015049203719, 0.004002196020065604959 ),
 .UNSPECIFIED. ) ;
#80142 = ORIENTED_EDGE ( 'NONE', *, *, #12281, .T. ) ;
#80143 = CARTESIAN_POINT ( 'NONE',  ( -5.923037968371668072, -6.376774720514413630, 19.62288733224861303 ) ) ;
#80144 = CARTESIAN_POINT ( 'NONE',  ( -110.6228709571500559, -24.99156045073393173, 7.747789690856161648 ) ) ;
#80145 = ORIENTED_EDGE ( 'NONE', *, *, #5909, .T. ) ;
#80146 = CARTESIAN_POINT ( 'NONE',  ( -83.62287095715005592, -24.50321055353805377, 9.387540953477522265 ) ) ;
#80147 = ORIENTED_EDGE ( 'NONE', *, *, #70975, .F. ) ;
#80148 = FACE_OUTER_BOUND ( 'NONE', #77002, .T. ) ;
#80149 = DIRECTION ( 'NONE',  ( 0.000000000000000000, -0.000000000000000000, -1.000000000000000000 ) ) ;
#80150 = CARTESIAN_POINT ( 'NONE',  ( 0.8369575198195864374, -20.89415947959451003, -1.500000000000002220 ) ) ;
#80151 = EDGE_CURVE ( 'NONE', #58306, #5356, #468, .T. ) ;
#80152 = CARTESIAN_POINT ( 'NONE',  ( -15.17958814119055155, -15.74432251006154715, 11.49999999999999645 ) ) ;
#80153 = CIRCLE ( 'NONE', #78467, 0.3000000000000016542 ) ;
#80154 = CARTESIAN_POINT ( 'NONE',  ( -107.6228709571500417, -23.73934037231757799, 11.05740245334328264 ) ) ;
#80155 = CARTESIAN_POINT ( 'NONE',  ( 15.32643653063177958, -3.577630190450218350, -27.14485409495429380 ) ) ;
#80156 = CARTESIAN_POINT ( 'NONE',  ( 22.48772827135616126, 0.8316936486096353498, 11.49999999999998934 ) ) ;
#80157 = CARTESIAN_POINT ( 'NONE',  ( -17.10473743203234775, -12.04273770408705246, -1.500000000000002220 ) ) ;
#80158 = DIRECTION ( 'NONE',  ( -3.773278334444166432E-23, 1.000000000000000000, 0.000000000000000000 ) ) ;
#80159 = DIRECTION ( 'NONE',  ( 0.000000000000000000, 0.000000000000000000, 1.000000000000000000 ) ) ;
#80160 = DIRECTION ( 'NONE',  ( 0.000000000000000000, -1.000000000000000000, 0.000000000000000000 ) ) ;
#80162 = ORIENTED_EDGE ( 'NONE', *, *, #78721, .T. ) ;
#80161 = EDGE_CURVE ( 'NONE', #83380, #89496, #93744, .T. ) ;
#80163 = ORIENTED_EDGE ( 'NONE', *, *, #96389, .T. ) ;
#80164 = ORIENTED_EDGE ( 'NONE', *, *, #26253, .F. ) ;
#80165 = CARTESIAN_POINT ( 'NONE',  ( -52.49586652078557591, -24.34968618360933945, 0.1864209137778880532 ) ) ;
#80166 = ORIENTED_EDGE ( 'NONE', *, *, #58968, .F. ) ;
#80167 = EDGE_CURVE ( 'NONE', #85963, #98513, #84037, .T. ) ;
#80168 = CARTESIAN_POINT ( 'NONE',  ( -2.751442626040462081, 21.25944542233241563, -1.500000000000002220 ) ) ;
#80169 = ORIENTED_EDGE ( 'NONE', *, *, #19140, .F. ) ;
#80170 = CARTESIAN_POINT ( 'NONE',  ( -95.55620429048337883, -23.47593901973091235, -1.443836447539001089 ) ) ;
#80171 = CARTESIAN_POINT ( 'NONE',  ( -17.90976863334866920, 11.11529090135583075, -1.500000000000002220 ) ) ;
#80172 = CARTESIAN_POINT ( 'NONE',  ( -30.45987962603713939, -25.30658194294376173, 6.147639284700202822 ) ) ;
#80173 = CARTESIAN_POINT ( 'NONE',  ( 9.402885806365684829, -5.965225279485572685, 29.04108526060719342 ) ) ;
#80174 = CARTESIAN_POINT ( 'NONE',  ( 0.000000000000000000, -16.94322527948557422, -1.149999999999999911 ) ) ;
#80175 = DIRECTION ( 'NONE',  ( -1.000000000000000000, -3.773278334444166432E-23, -8.201307841325785021E-29 ) ) ;
#80176 = CARTESIAN_POINT ( 'NONE',  ( 18.22792733936863030, -12.41963300964812156, -1.500000000000002220 ) ) ;
#80177 = ORIENTED_EDGE ( 'NONE', *, *, #6982, .T. ) ;
#80178 = LINE ( 'NONE', #2071, #64872 ) ;
#80179 = B_SPLINE_CURVE_WITH_KNOTS ( 'NONE', 3,
 ( #14251, #75649, #45226, #20869, #51840, #90888, #21859, #76150, #97504, #98487, #6649, #99488, #52832, #74661, #28988, #29983, #43727, #75160, #27999 ),
 .UNSPECIFIED., .F., .F.,
 ( 4, 1, 1, 1, 1, 1, 1, 1, 1, 1, 1, 1, 1, 1, 1, 1, 4 ),
 ( 0.000000000000000000, 0.06815824415599770758, 0.1347066022023564180, 0.2018649976035981897, 0.2707882662774624971, 0.3400242943604918633, 0.4080827390537212218, 0.4768131952581446398, 0.5473460643070942044, 0.5856397954238958814, 0.6288649531777639190, 0.6771532033637904791, 0.7308028113651051649, 0.7898066155325015325, 0.8543250087420142247, 0.9243651340575425035, 1.000000000000000000 ),
 .UNSPECIFIED. ) ;
#80180 = CARTESIAN_POINT ( 'NONE',  ( -111.6228709571501128, -24.35013146730204525, 9.818937971375108376 ) ) ;
#80181 = CARTESIAN_POINT ( 'NONE',  ( -41.14436886340001820, -25.31624709515424598, 5.395510681755817828 ) ) ;
#80182 = EDGE_CURVE ( 'NONE', #39193, #81122, #61955, .T. ) ;
#80183 = CARTESIAN_POINT ( 'NONE',  ( -62.64802848561124193, -23.73791477778912196, 11.05961554403171121 ) ) ;
#80184 = CARTESIAN_POINT ( 'NONE',  ( -26.29960327999231495, -24.65857663733338967, 2.249178454020304585 ) ) ;
#80185 = AXIS2_PLACEMENT_3D ( 'NONE', #34655, #71718, #65624 ) ;
#80186 = LINE ( 'NONE', #87802, #22216 ) ;
#80187 = CARTESIAN_POINT ( 'NONE',  ( -14.61619677566029729, 15.53698580111986693, -1.500000000000002220 ) ) ;
#80188 = CARTESIAN_POINT ( 'NONE',  ( -91.62287095715004170, -23.47596703998600631, 11.44779298504227860 ) ) ;
#80189 = CARTESIAN_POINT ( 'NONE',  ( -124.5228709571500616, -23.72747288104470798, -1.053458166803225460 ) ) ;
#80190 = ADVANCED_FACE ( 'NONE', ( #37608 ), #64818, .F. ) ;
#80191 = DIRECTION ( 'NONE',  ( 0.000000000000000000, -0.9999999999976377785, -2.173523156925979128E-06 ) ) ;
#80192 = PLANE ( 'NONE',  #68607 ) ;
#80193 = CARTESIAN_POINT ( 'NONE',  ( -14.16962031475959272, 17.58799634409329471, -1.500000000000002220 ) ) ;
#80194 = CARTESIAN_POINT ( 'NONE',  ( -15.87499999999997868, 0.000000000000000000, 0.000000000000000000 ) ) ;
#80195 = ORIENTED_EDGE ( 'NONE', *, *, #28939, .F. ) ;
#80196 = CARTESIAN_POINT ( 'NONE',  ( 8.720681858489903959, 3.316774720514428232, -28.09278397295777197 ) ) ;
#80197 = CARTESIAN_POINT ( 'NONE',  ( 2.904396343079095111, -5.876774720514415407, 19.95793242748194984 ) ) ;
#80198 = CARTESIAN_POINT ( 'NONE',  ( -19.50520112914412252, -2.896358124273927359, 11.49999999999999645 ) ) ;
#80199 = FACE_OUTER_BOUND ( 'NONE', #90921, .T. ) ;
#80200 = CARTESIAN_POINT ( 'NONE',  ( -96.62287095715005592, -23.47593901973091235, -1.443836447539001089 ) ) ;
#80201 = EDGE_CURVE ( 'NONE', #20296, #16787, #77151, .T. ) ;
#80202 = ORIENTED_EDGE ( 'NONE', *, *, #68508, .T. ) ;
#80203 = DIRECTION ( 'NONE',  ( 0.000000000000000000, -2.173523156925980399E-06, 0.9999999999976378895 ) ) ;
#80204 = CARTESIAN_POINT ( 'NONE',  ( -24.90875734969025501, 6.475225279485573360, 26.43402280011862615 ) ) ;
#80205 = CARTESIAN_POINT ( 'NONE',  ( -105.5228709571501042, -24.92604778743017135, 8.074972756849355449 ) ) ;
#80206 = PLANE ( 'NONE',  #42122 ) ;
#80207 = CARTESIAN_POINT ( 'NONE',  ( -68.62287095715005592, -24.65952944569304606, 1.056160979905698794 ) ) ;
#80208 = CYLINDRICAL_SURFACE ( 'NONE', #65958, 1.000000000000000000 ) ;
#80209 = CARTESIAN_POINT ( 'NONE',  ( -81.87216895719394927, -25.23777318042872508, 6.379003627969344947 ) ) ;
#80210 = CARTESIAN_POINT ( 'NONE',  ( -11.78406182805296254, 15.88391379356440503, 11.49999999999998934 ) ) ;
#80211 = ORIENTED_EDGE ( 'NONE', *, *, #84654, .F. ) ;
#80212 = CARTESIAN_POINT ( 'NONE',  ( 8.147030896810244727, 18.52525024547675869, 11.49999999999999645 ) ) ;
#80213 = DIRECTION ( 'NONE',  ( -1.000000000000000000, -0.000000000000000000, -0.000000000000000000 ) ) ;
#80214 = VECTOR ( 'NONE', #84583, 1000.000000000000000 ) ;
#80215 = ORIENTED_EDGE ( 'NONE', *, *, #50586, .T. ) ;
#80216 = CARTESIAN_POINT ( 'NONE',  ( -65.52287095715006160, -23.47596703998600631, 11.44779298504228748 ) ) ;
#80217 = DIRECTION ( 'NONE',  ( -4.251773225433346808E-15, 0.000000000000000000, 1.000000000000000000 ) ) ;
#80218 = FACE_OUTER_BOUND ( 'NONE', #51351, .T. ) ;
#80219 = CARTESIAN_POINT ( 'NONE',  ( -82.62287095715005592, -23.47593901973091235, -1.443836447539004642 ) ) ;
#80220 = CARTESIAN_POINT ( 'NONE',  ( -7.641025641025641413, -6.376774720514418959, 20.36458333333334636 ) ) ;
#80221 = CARTESIAN_POINT ( 'NONE',  ( 19.72776355195876619, -6.376774720514426953, 28.39950002376592764 ) ) ;
#80222 = CARTESIAN_POINT ( 'NONE',  ( 19.28819943863484454, -5.468471092112969778, 11.49999999999998934 ) ) ;
#80223 = AXIS2_PLACEMENT_3D ( 'NONE', #2037, #55322, #8635 ) ;
#80224 = DIRECTION ( 'NONE',  ( -0.9951627101165078093, -0.09824042138329590335, -1.421085471520200214E-14 ) ) ;
#80225 = EDGE_LOOP ( 'NONE', ( #85148, #19373, #48303, #33448 ) ) ;
#80226 = CIRCLE ( 'NONE', #60830, 6.600000000000001421 ) ;
#80227 = CARTESIAN_POINT ( 'NONE',  ( -32.62287095715005592, -24.66019654487199020, 8.947790411086137041 ) ) ;
#80228 = CARTESIAN_POINT ( 'NONE',  ( -89.62287095715004170, -29.50248528299804818, 1.056150453629040253 ) ) ;
#80229 = CARTESIAN_POINT ( 'NONE',  ( -79.39460018469020497, -25.28987694977702816, 5.623653258205846939 ) ) ;
#80230 = DIRECTION ( 'NONE',  ( -0.09824042138329590335, 4.470611911092166224E-17, -0.9951627101165078093 ) ) ;
#80231 = B_SPLINE_CURVE_WITH_KNOTS ( 'NONE', 3,
 ( #86521, #93622, #95141, #9395, #2807, #32734 ),
 .UNSPECIFIED., .F., .F.,
 ( 4, 2, 4 ),
 ( 6.384118678608569234E-06, 0.001386860460828372166, 0.002767336802978135821 ),
 .UNSPECIFIED. ) ;
#80232 = CARTESIAN_POINT ( 'NONE',  ( -73.62685968689160632, -24.51314013834315375, 0.6176544820404104019 ) ) ;
#80233 = CARTESIAN_POINT ( 'NONE',  ( 1.949999999999999956, 0.1925000000000000044, -0.1925000000000000600 ) ) ;
#80234 = ADVANCED_FACE ( 'NONE', ( #2561 ), #86280, .F. ) ;
#80235 = CARTESIAN_POINT ( 'NONE',  ( -99.90567954317651811, -25.30060005375480969, 6.009289253917325269 ) ) ;
#80236 = VERTEX_POINT ( 'NONE', #56360 ) ;
#80237 = EDGE_CURVE ( 'NONE', #94885, #27247, #78147, .T. ) ;
#80238 = CARTESIAN_POINT ( 'NONE',  ( -15.70679263237263434, -12.88635299011707502, 11.49999999999998934 ) ) ;
#80239 = VERTEX_POINT ( 'NONE', #1052 ) ;
#80240 = CARTESIAN_POINT ( 'NONE',  ( -32.49651614175236602, -24.15543982623907127, -0.2315651400026567941 ) ) ;
#80241 = ADVANCED_FACE ( 'NONE', ( #70556 ), #72079, .T. ) ;
#80242 = CARTESIAN_POINT ( 'NONE',  ( -127.5903467349210132, -23.73791477778912551, 11.05961554403169345 ) ) ;
#80243 = VERTEX_POINT ( 'NONE', #17779 ) ;
#80244 = CARTESIAN_POINT ( 'NONE',  ( -59.56672357952546548, -23.48786465467241058, 11.44779295918255357 ) ) ;
#80245 = ADVANCED_FACE ( 'NONE', ( #40619 ), #35588, .T. ) ;
#80246 = CARTESIAN_POINT ( 'NONE',  ( 15.09050776547575090, 3.531431454755690869, -27.29583770106899365 ) ) ;
#80247 = CARTESIAN_POINT ( 'NONE',  ( -86.62287095715004170, -23.47593901973091235, -1.443836447539002865 ) ) ;
#80248 = CARTESIAN_POINT ( 'NONE',  ( 19.38521227897113874, -8.589346653930519437, 11.49999999999999645 ) ) ;
#80249 = AXIS2_PLACEMENT_3D ( 'NONE', #36655, #59011, #99035 ) ;
#80250 = B_SPLINE_CURVE_WITH_KNOTS ( 'NONE', 3,
 ( #41719, #80262, #65568, #72659, #81760, #3156 ),
 .UNSPECIFIED., .F., .F.,
 ( 4, 2, 4 ),
 ( 0.000000000000000000, 0.001380901958385390930, 0.002761803916770781860 ),
 .UNSPECIFIED. ) ;
#80251 = CARTESIAN_POINT ( 'NONE',  ( 17.13038851031509680, -14.05419017248541813, -1.500000000000002220 ) ) ;
#80252 = ADVANCED_FACE ( 'NONE', ( #24875 ), #31994, .F. ) ;
#80253 = CARTESIAN_POINT ( 'NONE',  ( -16.28974412851428255, -12.55652860423730388, -1.500000000000002220 ) ) ;
#80254 = VERTEX_POINT ( 'NONE', #87278 ) ;
#80255 = CARTESIAN_POINT ( 'NONE',  ( -111.6228709571500559, -23.48783264082479505, -1.443836473390060604 ) ) ;
#80256 = ORIENTED_EDGE ( 'NONE', *, *, #89716, .T. ) ;
#80257 = CARTESIAN_POINT ( 'NONE',  ( -37.22287095715005734, -23.47596703998600276, 11.44779298504227683 ) ) ;
#80258 = CARTESIAN_POINT ( 'NONE',  ( 2.591664760199015927, -5.876774720514418071, 20.15921530338947321 ) ) ;
#80259 = ORIENTED_EDGE ( 'NONE', *, *, #82231, .F. ) ;
#80260 = ORIENTED_EDGE ( 'NONE', *, *, #80182, .F. ) ;
#80261 = ORIENTED_EDGE ( 'NONE', *, *, #68734, .T. ) ;
#80262 = CARTESIAN_POINT ( 'NONE',  ( -116.6228709571500417, -23.72773821059535848, 11.05748984161097503 ) ) ;
#80263 = CARTESIAN_POINT ( 'NONE',  ( 7.052174998393318184, -5.876774720514418071, 20.39928653130861136 ) ) ;
#80264 = CARTESIAN_POINT ( 'NONE',  ( 5.705253819860196529, -6.376774720514415407, 19.95963554344900714 ) ) ;
#80265 = CARTESIAN_POINT ( 'NONE',  ( 11.71144010791963730, -17.07555522294065753, -1.500000000000002220 ) ) ;
#80266 = CARTESIAN_POINT ( 'NONE',  ( -20.76051858633888259, -6.224802954461835292, 11.49999999999999645 ) ) ;
#80267 = EDGE_LOOP ( 'NONE', ( #81164, #78352, #28295, #78525, #85127, #57086 ) ) ;
#80268 = DIRECTION ( 'NONE',  ( 0.000000000000000000, -0.000000000000000000, 1.000000000000000000 ) ) ;
#80269 = DIRECTION ( 'NONE',  ( 0.000000000000000000, 0.000000000000000000, -1.000000000000000000 ) ) ;
#80270 = CARTESIAN_POINT ( 'NONE',  ( -9.774569144048079750, -20.17623354167628946, -1.500000000000002220 ) ) ;
#80271 = CARTESIAN_POINT ( 'NONE',  ( -2.749999999999999112, 26.59999999999999432, 0.000000000000000000 ) ) ;
#80272 = CARTESIAN_POINT ( 'NONE',  ( -71.62287095715005592, -23.73907113216990794, -1.053371485793230811 ) ) ;
#80273 = EDGE_LOOP ( 'NONE', ( #46975, #6778, #66203, #38123 ) ) ;
#80274 = CARTESIAN_POINT ( 'NONE',  ( -45.58953762381671737, -24.99132157543083821, 2.256160258750496084 ) ) ;
#80275 = CARTESIAN_POINT ( 'NONE',  ( -98.62287095715005592, -29.50248528299804818, 1.056150453629042030 ) ) ;
#80276 = VERTEX_POINT ( 'NONE', #64483 ) ;
#80277 = ORIENTED_EDGE ( 'NONE', *, *, #92775, .F. ) ;
#80278 = VECTOR ( 'NONE', #82225, 1000.000000000000000 ) ;
#80279 = CARTESIAN_POINT ( 'NONE',  ( -46.54046596679725667, -24.35071581493542325, 9.817618358456032368 ) ) ;
#80280 = ORIENTED_EDGE ( 'NONE', *, *, #3420, .T. ) ;
#80281 = VECTOR ( 'NONE', #54053, 1000.000000000000114 ) ;
#80282 = DIRECTION ( 'NONE',  ( 3.773278334444167608E-23, -1.000000000000000000, 0.000000000000000000 ) ) ;
#80283 = CARTESIAN_POINT ( 'NONE',  ( -0.06837171988653999166, -21.26218376953697486, -1.500000000000002220 ) ) ;
#80284 = ORIENTED_EDGE ( 'NONE', *, *, #39530, .F. ) ;
#80285 = CARTESIAN_POINT ( 'NONE',  ( -100.5101194842158634, -25.12316535023712660, 7.100618891458206683 ) ) ;
#80286 = CARTESIAN_POINT ( 'NONE',  ( 3.468383421097696928, -21.53508805063734854, -1.500000000000002220 ) ) ;
#80287 = FACE_OUTER_BOUND ( 'NONE', #11, .T. ) ;
#80288 = CARTESIAN_POINT ( 'NONE',  ( 6.561060095583167495, -6.376774720514427841, 21.83518827598938117 ) ) ;
#80289 = CIRCLE ( 'NONE', #27061, 251.9358649670780892 ) ;
#80290 = CARTESIAN_POINT ( 'NONE',  ( -35.62287095715006302, -23.84047902841601285, -0.8780736468305813114 ) ) ;
#80291 = CARTESIAN_POINT ( 'NONE',  ( 19.17057494584436839, 10.47865234463220396, -1.500000000000002220 ) ) ;
#80292 = LINE ( 'NONE', #4676, #78732 ) ;
#80293 = EDGE_LOOP ( 'NONE', ( #23795, #82687, #58071, #54458 ) ) ;
#80294 = CARTESIAN_POINT ( 'NONE',  ( 29.57907552799943218, -3.518969226524878646, 29.21818156447044501 ) ) ;
#80295 = CARTESIAN_POINT ( 'NONE',  ( -85.58383951320973893, -24.83644354573578994, 8.397322867130101898 ) ) ;
#80296 = AXIS2_PLACEMENT_3D ( 'NONE', #84888, #64089, #62569 ) ;
#80297 = VECTOR ( 'NONE', #20836, 1000.000000000000000 ) ;
#80298 = ORIENTED_EDGE ( 'NONE', *, *, #96853, .T. ) ;
#80299 = CARTESIAN_POINT ( 'NONE',  ( -99.62287095715005592, -23.47596703998600631, 11.44779298504227860 ) ) ;
#80300 = EDGE_LOOP ( 'NONE', ( #71675, #18996, #96139, #83389 ) ) ;
#80301 = CARTESIAN_POINT ( 'NONE',  ( -8.499999999999987566, 18.99999999999977973, 0.000000000000000000 ) ) ;
#80302 = CARTESIAN_POINT ( 'NONE',  ( -113.6228709571500275, -23.96127896941632685, -0.6493128931037774887 ) ) ;
#80303 = CARTESIAN_POINT ( 'NONE',  ( -15.86343167427570577, 14.10970434637795634, -1.500000000000002220 ) ) ;
#80304 = PLANE ( 'NONE',  #28785 ) ;
#80305 = CARTESIAN_POINT ( 'NONE',  ( -30.56688274934923655, -25.56688301298833821, 3.825958421598584014 ) ) ;
#80306 = EDGE_CURVE ( 'NONE', #47994, #47959, #51337, .T. ) ;
#80307 = PLANE ( 'NONE',  #68037 ) ;
#80308 = CARTESIAN_POINT ( 'NONE',  ( -118.6228709571500559, -29.50247984919015209, -1.443849546365046699 ) ) ;
#80309 = CARTESIAN_POINT ( 'NONE',  ( 11.34002819025610087, 15.78594478779102950, 11.49999999999998934 ) ) ;
#80310 = EDGE_CURVE ( 'NONE', #69320, #93091, #23439, .T. ) ;
#80311 = CARTESIAN_POINT ( 'NONE',  ( -45.52502742233122746, -24.92564183028978775, 1.928384488918256645 ) ) ;
#80312 = VERTEX_POINT ( 'NONE', #47225 ) ;
#80313 = CARTESIAN_POINT ( 'NONE',  ( -2.678125609936932605, 19.29598960679622976, 11.49999999999999645 ) ) ;
#80314 = CARTESIAN_POINT ( 'NONE',  ( -5.554587162835583847, -5.876774720514415407, 19.99258394656885329 ) ) ;
#80315 = CARTESIAN_POINT ( 'NONE',  ( -42.52287095715005449, -23.48786465467240347, 11.44779295918255180 ) ) ;
#80316 = ORIENTED_EDGE ( 'NONE', *, *, #59115, .F. ) ;
#80317 = CARTESIAN_POINT ( 'NONE',  ( -97.52287095715009002, -24.51283580621364067, 0.6167428607019849185 ) ) ;
#80318 = CARTESIAN_POINT ( 'NONE',  ( -89.50344290891156618, -24.65952944569304250, 1.056160979905700126 ) ) ;
#80319 = CARTESIAN_POINT ( 'NONE',  ( 13.91401389203221406, -6.376774720514426953, 158.0376437107427137 ) ) ;
#80320 = CARTESIAN_POINT ( 'NONE',  ( 12.66784028006542151, -2.682774720514427003, -27.12025593822526304 ) ) ;
#80321 = CARTESIAN_POINT ( 'NONE',  ( 15.21843288076463629, 12.49332292251147614, 11.49999999999998934 ) ) ;
#80322 = ORIENTED_EDGE ( 'NONE', *, *, #36947, .F. ) ;
#80323 = VECTOR ( 'NONE', #27697, 1000.000000000000114 ) ;
#80324 = CARTESIAN_POINT ( 'NONE',  ( 33.13288845015618023, 5.965225279485572685, -0.1650522222209214185 ) ) ;
#80325 = CARTESIAN_POINT ( 'NONE',  ( -17.29220519630379016, 15.29500218549028645, -1.500000000000002220 ) ) ;
#80326 = PERSON_AND_ORGANIZATION ( #70597, #27821 ) ;
#80327 = EDGE_LOOP ( 'NONE', ( #84628, #75254, #18342, #11145 ) ) ;
#80328 = CARTESIAN_POINT ( 'NONE',  ( -125.5228709571500900, -24.15516710230294706, 10.28746687063725318 ) ) ;
#80329 = CARTESIAN_POINT ( 'NONE',  ( -2.070328576748420524, -6.376774720514410077, 19.46575348430201657 ) ) ;
#80330 = DIRECTION ( 'NONE',  ( 0.000000000000000000, 0.000000000000000000, 1.000000000000000000 ) ) ;
#80331 = FACE_OUTER_BOUND ( 'NONE', #65544, .T. ) ;
#80332 = CARTESIAN_POINT ( 'NONE',  ( -119.5228709571500616, -24.50216790748206819, 0.6166512839542566127 ) ) ;
#80333 = APPLICATION_CONTEXT ( 'configuration controlled 3d designs of mechanical parts and assemblies' ) ;
#80334 = CARTESIAN_POINT ( 'NONE',  ( -75.62287095715005592, -23.47596703998600631, 11.44779298504227860 ) ) ;
#80335 = LINE ( 'NONE', #97058, #62442 ) ;
#80336 = CARTESIAN_POINT ( 'NONE',  ( -15.85412420263326538, -12.13584807887712458, 11.49999999999998934 ) ) ;
#80337 = LINE ( 'NONE', #10831, #40367 ) ;
#80338 = CARTESIAN_POINT ( 'NONE',  ( -16.82575997001036328, 10.57904039763333159, -1.500000000000002220 ) ) ;
#80339 = EDGE_LOOP ( 'NONE', ( #17254, #75088, #52180, #3057 ) ) ;
#80340 = CARTESIAN_POINT ( 'NONE',  ( 8.599999999999999645, 24.84999999999999787, 0.000000000000000000 ) ) ;
#80341 = ADVANCED_FACE ( 'NONE', ( #86779 ), #54835, .T. ) ;
#80342 = DIRECTION ( 'NONE',  ( -0.9940716917543757081, -0.000000000000000000, -0.1087265912856348465 ) ) ;
#80343 = PLANE ( 'NONE',  #20377 ) ;
#80344 = CARTESIAN_POINT ( 'NONE',  ( 12.98941176893815275, -6.376774720518460171, -28.15829778590956067 ) ) ;
#80345 = CARTESIAN_POINT ( 'NONE',  ( 14.06386034339543478, -15.33156129944631729, 11.49999999999999645 ) ) ;
#80346 = CARTESIAN_POINT ( 'NONE',  ( -7.421417143192116761, -6.376774720514411854, 19.43823095447975291 ) ) ;
#80347 = CARTESIAN_POINT ( 'NONE',  ( 1.754398552524170762, 17.92127466780477718, 9.000000000000000000 ) ) ;
#80348 = CARTESIAN_POINT ( 'NONE',  ( 22.85402955525884394, -0.1436109537974766814, 11.49999999999999645 ) ) ;
#80349 = VERTEX_POINT ( 'NONE', #80174 ) ;
#80350 = DIRECTION ( 'NONE',  ( 0.000000000000000000, 0.9999999999976377785, 2.173523156925979128E-06 ) ) ;
#80352 = CIRCLE ( 'NONE', #8360, 1.050000000000000488 ) ;
#80351 = CARTESIAN_POINT ( 'NONE',  ( -38.52287095715009713, -23.96127896942170921, -0.6493128930931766352 ) ) ;
#80353 = VERTEX_POINT ( 'NONE', #28375 ) ;
#80354 = EDGE_CURVE ( 'NONE', #61052, #11601, #69489, .T. ) ;
#80355 = AXIS2_PLACEMENT_3D ( 'NONE', #49898, #65130, #11317 ) ;
#80356 = CARTESIAN_POINT ( 'NONE',  ( -9.806399893892750796, 17.69452640759178408, 11.49999999999998934 ) ) ;
#80357 = CARTESIAN_POINT ( 'NONE',  ( 7.267403311989051318, -6.376774720514426065, 21.43157132964656952 ) ) ;
#80358 = B_SPLINE_CURVE_WITH_KNOTS ( 'NONE', 3,
 ( #81607, #26817, #74485, #58767 ),
 .UNSPECIFIED., .F., .F.,
 ( 4, 4 ),
 ( 0.000000000000000000, 0.001846153846153858469 ),
 .UNSPECIFIED. ) ;
#80359 = CARTESIAN_POINT ( 'NONE',  ( 14.52511747680497933, 6.475225279485573360, -27.86035006098926559 ) ) ;
#80360 = EDGE_CURVE ( 'NONE', #13954, #51364, #87649, .T. ) ;
#80361 = AXIS2_PLACEMENT_3D ( 'NONE', #16570, #78468, #1866 ) ;
#80362 = B_SPLINE_CURVE_WITH_KNOTS ( 'NONE', 3,
 ( #27485, #66570, #35097, #12732 ),
 .UNSPECIFIED., .F., .F.,
 ( 4, 4 ),
 ( 0.000000000000000000, 9.999999999998897304E-05 ),
 .UNSPECIFIED. ) ;
#80363 = CARTESIAN_POINT ( 'NONE',  ( -106.5895376238167387, -24.64898659630368627, 1.056161002820392270 ) ) ;
#80364 = EDGE_CURVE ( 'NONE', #13454, #52986, #76063, .T. ) ;
#80365 = ORIENTED_EDGE ( 'NONE', *, *, #44166, .F. ) ;
#80366 = CARTESIAN_POINT ( 'NONE',  ( -79.56610238236960697, -25.31162433482952423, 5.317911015495634608 ) ) ;
#80367 = CARTESIAN_POINT ( 'NONE',  ( -51.62287095715005592, -23.48783264082478084, -1.443836473390070596 ) ) ;
#80368 = CARTESIAN_POINT ( 'NONE',  ( -7.547287378330592489, -18.53391252851691462, -1.500000000000002220 ) ) ;
#80369 = EDGE_CURVE ( 'NONE', #86861, #58117, #74549, .T. ) ;
#80370 = CARTESIAN_POINT ( 'NONE',  ( 13.96602909953038640, 15.60522523583095200, 11.49999999999999645 ) ) ;
#80371 = CARTESIAN_POINT ( 'NONE',  ( -27.25988310792305214, -5.965225279485572685, 30.32664379231667695 ) ) ;
#80372 = CARTESIAN_POINT ( 'NONE',  ( -124.6228709571500275, -23.72773821059535848, 11.05748984161097503 ) ) ;
#80373 = CARTESIAN_POINT ( 'NONE',  ( 14.91618686576236108, -16.25093855066790738, 11.49999999999998934 ) ) ;
#80374 = EDGE_CURVE ( 'NONE', #26606, #3797, #9724, .T. ) ;
#80375 = CARTESIAN_POINT ( 'NONE',  ( 9.679460662220623846, 4.838530677111208433, -26.38948590882341705 ) ) ;
#80376 = ORIENTED_EDGE ( 'NONE', *, *, #71672, .T. ) ;
#80377 = CARTESIAN_POINT ( 'NONE',  ( -47.52287095715006160, -24.65952944569304606, 1.056160979905693686 ) ) ;
#80378 = CARTESIAN_POINT ( 'NONE',  ( 282.9764569301858046, 4.540774720514427543, 20.79159422840526616 ) ) ;
#80379 = CARTESIAN_POINT ( 'NONE',  ( -50.55620429048340014, -24.99132157543166599, 2.256160258750668390 ) ) ;
#80380 = VERTEX_POINT ( 'NONE', #49247 ) ;
#80381 = CARTESIAN_POINT ( 'NONE',  ( -123.6228709571500559, -23.47596703998600631, 11.44779298504227860 ) ) ;
#80382 = ORIENTED_EDGE ( 'NONE', *, *, #40627, .F. ) ;
#80383 = VERTEX_POINT ( 'NONE', #96897 ) ;
#80384 = LINE ( 'NONE', #85993, #100360 ) ;
#80385 = CARTESIAN_POINT ( 'NONE',  ( 30.93860345374796594, 6.475225279485573360, 19.84760796525321780 ) ) ;
#80387 = EDGE_CURVE ( 'NONE', #14248, #16991, #55079, .T. ) ;
#80386 = CARTESIAN_POINT ( 'NONE',  ( 31.82032313667048484, -5.965225279485572685, 9.148483289431936782 ) ) ;
#80388 = CARTESIAN_POINT ( 'NONE',  ( 12.01435098137705637, -16.61664908515649941, -1.500000000000002220 ) ) ;
#80389 = VERTEX_POINT ( 'NONE', #10665 ) ;
#80390 = CARTESIAN_POINT ( 'NONE',  ( -91.62287095715004170, -29.50250786944525672, 11.44777988621623344 ) ) ;
#80391 = CARTESIAN_POINT ( 'NONE',  ( -19.80875734969026425, -5.965225279485572685, 31.02402280011862246 ) ) ;
#80392 = CARTESIAN_POINT ( 'NONE',  ( -96.55620429048339304, -24.66019654487199730, 8.947790411086124607 ) ) ;
#80393 = CARTESIAN_POINT ( 'NONE',  ( -18.48265707593502327, -12.51853143457666562, 11.49999999999998934 ) ) ;
#80394 = CARTESIAN_POINT ( 'NONE',  ( 29.70220533433690946, -3.451715827188561736, 28.20564067601642222 ) ) ;
#80395 = CARTESIAN_POINT ( 'NONE',  ( -104.6228709571500559, -24.64898659630529210, 1.056161002820829697 ) ) ;
#80396 = ORIENTED_EDGE ( 'NONE', *, *, #70784, .F. ) ;
#80397 = CARTESIAN_POINT ( 'NONE',  ( 10.34999999999998010, 27.69999999999999929, 0.000000000000000000 ) ) ;
#80398 = CARTESIAN_POINT ( 'NONE',  ( -73.52287095715010423, -24.34917612406836795, 0.1852690917426544071 ) ) ;
#80399 = CARTESIAN_POINT ( 'NONE',  ( -16.98601802344612111, -12.12340321765213069, 11.49999999999998934 ) ) ;
#80400 = VERTEX_POINT ( 'NONE', #89786 ) ;
#80402 = VERTEX_POINT ( 'NONE', #34999 ) ;
#80401 = CARTESIAN_POINT ( 'NONE',  ( -86.62287095715004170, -29.50247984919015209, -1.443849546365051806 ) ) ;
#80403 = ORIENTED_EDGE ( 'NONE', *, *, #32422, .T. ) ;
#80404 = CARTESIAN_POINT ( 'NONE',  ( -32.99388727629348494, -25.11010231571544082, 2.831122766524410750 ) ) ;
#80405 = CARTESIAN_POINT ( 'NONE',  ( 17.02745815656931683, -12.38318283856952107, -1.500000000000002220 ) ) ;
#80406 = ORIENTED_EDGE ( 'NONE', *, *, #35629, .T. ) ;
#80407 = DIRECTION ( 'NONE',  ( 0.000000000000000000, -1.000000000000000000, 0.000000000000000000 ) ) ;
#80408 = CARTESIAN_POINT ( 'NONE',  ( -78.62287095715007013, -23.48783264082478439, -1.443836473390065711 ) ) ;
#80409 = CARTESIAN_POINT ( 'NONE',  ( -120.5892019400240827, -24.63419186844610920, 9.035850630976920428 ) ) ;
#80410 = CARTESIAN_POINT ( 'NONE',  ( -86.63552721385731559, -23.96169478059713498, 10.65365249895717881 ) ) ;
#80411 = CARTESIAN_POINT ( 'NONE',  ( -49.98701657552408761, -25.11998546545770594, 2.886102727180880567 ) ) ;
#80412 = CARTESIAN_POINT ( 'NONE',  ( -21.53672441135761773, -2.854535511010750870, -1.500000000000002220 ) ) ;
#80413 = CARTESIAN_POINT ( 'NONE',  ( -80.60699767246597958, -25.24759804226244597, 7.098405785189711992 ) ) ;
#80415 = ORIENTED_EDGE ( 'NONE', *, *, #30402, .F. ) ;
#80414 = CARTESIAN_POINT ( 'NONE',  ( -5.617636847906702258, 21.56867655435222630, 11.49999999999999645 ) ) ;
#80416 = CARTESIAN_POINT ( 'NONE',  ( -51.02375840103924531, -25.24728759653825350, 5.363929794370636550 ) ) ;
#80417 = DIRECTION ( 'NONE',  ( 1.000000000000000000, -1.232047923278981953E-16, 0.000000000000000000 ) ) ;
#80418 = FACE_OUTER_BOUND ( 'NONE', #40723, .T. ) ;
#80419 = ORIENTED_EDGE ( 'NONE', *, *, #43262, .F. ) ;
#80420 = VECTOR ( 'NONE', #79458, 1000.000000000000000 ) ;
#80422 = ORIENTED_EDGE ( 'NONE', *, *, #18829, .F. ) ;
#80421 = CARTESIAN_POINT ( 'NONE',  ( -53.01255352321339842, -4.132774720514426292, 35.59556822165056644 ) ) ;
#80423 = ADVANCED_FACE ( 'NONE', ( #89287 ), #73074, .T. ) ;
#80424 = ORIENTED_EDGE ( 'NONE', *, *, #25317, .F. ) ;
#80425 = DIRECTION ( 'NONE',  ( 0.000000000000000000, 0.000000000000000000, -1.000000000000000000 ) ) ;
#80426 = EDGE_CURVE ( 'NONE', #90367, #88122, #24288, .T. ) ;
#80427 = CIRCLE ( 'NONE', #5892, 1.250000000000001998 ) ;
#80428 = CARTESIAN_POINT ( 'NONE',  ( -4.621320343559624177, 12.75000000000004974, 2.100000000000000089 ) ) ;
#80429 = CARTESIAN_POINT ( 'NONE',  ( 29.73860345376319003, -5.356471260711259674, 19.84760796525321425 ) ) ;
#80430 = EDGE_LOOP ( 'NONE', ( #47935, #35462, #34470, #97320 ) ) ;
#80431 = VECTOR ( 'NONE', #50807, 1000.000000000000000 ) ;
#80432 = CARTESIAN_POINT ( 'NONE',  ( -130.5728709571500588, -24.35282530332708362, -0.01110346469458741055 ) ) ;
#80433 = CARTESIAN_POINT ( 'NONE',  ( -16.90645664988545249, 14.66980924573920397, -1.500000000000002220 ) ) ;
#80434 = CIRCLE ( 'NONE', #78812, 91.74549126261078413 ) ;
#80435 = VECTOR ( 'NONE', #55996, 1000.000000000000000 ) ;
#80436 = ORIENTED_EDGE ( 'NONE', *, *, #52873, .T. ) ;
#80437 = CARTESIAN_POINT ( 'NONE',  ( -112.5161576296912074, -24.35071581493543391, 9.817618358456016381 ) ) ;
#80438 = CARTESIAN_POINT ( 'NONE',  ( -101.5146321277283761, -24.15620529776628800, 10.23563542870660292 ) ) ;
#80439 = FACE_OUTER_BOUND ( 'NONE', #77142, .T. ) ;
#80440 = CARTESIAN_POINT ( 'NONE',  ( 29.73828978136053891, -14.82721238576461609, -4.021765098496561386 ) ) ;
#80441 = AXIS2_PLACEMENT_3D ( 'NONE', #93187, #93689, #86582 ) ;
#80442 = CARTESIAN_POINT ( 'NONE',  ( -130.5728709571500588, -24.26827793580486414, 9.960784317162948653 ) ) ;
#80443 = CARTESIAN_POINT ( 'NONE',  ( 13.16580039582533423, -14.52177825760336205, 11.49999999999998934 ) ) ;
#80444 = CARTESIAN_POINT ( 'NONE',  ( 0.000000000000000000, 1.826774720514426464, 0.000000000000000000 ) ) ;
#80445 = EDGE_LOOP ( 'NONE', ( #8990, #11639, #94502 ) ) ;
#80446 = CARTESIAN_POINT ( 'NONE',  ( -10.19830463584622571, -18.94658877215714909, 11.49999999999998934 ) ) ;
#80447 = CARTESIAN_POINT ( 'NONE',  ( -75.62287095715004170, -25.00182538069145366, 7.747789668545099317 ) ) ;
#80448 = CARTESIAN_POINT ( 'NONE',  ( -81.01373513877602761, -25.31572665590242366, 5.057100087033362001 ) ) ;
#80449 = DIRECTION ( 'NONE',  ( -1.000000000000000000, 0.000000000000000000, 1.104558621438292892E-14 ) ) ;
#80450 = CARTESIAN_POINT ( 'NONE',  ( 15.58962545129234556, 1.684774720514426560, -26.91365498785467736 ) ) ;
#80451 = CARTESIAN_POINT ( 'NONE',  ( 22.95104020007722667, -0.4190376320207603866, -1.500000000000002220 ) ) ;
#80452 = APPROVAL ( #15541, 'UNSPECIFIED' ) ;
#80453 = PERSON_AND_ORGANIZATION ( #70597, #27821 ) ;
#80454 = CARTESIAN_POINT ( 'NONE',  ( -31.62287095715005236, -24.66019654487199020, 8.947790411086138818 ) ) ;
#80455 = CARTESIAN_POINT ( 'NONE',  ( -49.52204961490906499, -23.48783264082477018, -1.443836473390094133 ) ) ;
#80456 = CARTESIAN_POINT ( 'NONE',  ( 13.72940079880349984, -14.68433028913016791, 11.49999999999999645 ) ) ;
#80457 = DIRECTION ( 'NONE',  ( -3.773278334453079030E-23, 0.9999999999976377785, 2.173523156925979128E-06 ) ) ;
#80458 = CARTESIAN_POINT ( 'NONE',  ( -41.52287095715006870, -29.50250786944525672, 11.44777988621624232 ) ) ;
#80459 = DIRECTION ( 'NONE',  ( 1.000000000000000000, 3.773278334444166432E-23, 8.201307841325785021E-29 ) ) ;
#80460 = CARTESIAN_POINT ( 'NONE',  ( 33.74124265030975067, 3.622774720514426949, -12.32597719988138252 ) ) ;
#80461 = CARTESIAN_POINT ( 'NONE',  ( 14.85834502026402681, 2.682774720514426559, -27.37203305628894867 ) ) ;
#80462 = CARTESIAN_POINT ( 'NONE',  ( -15.05033210666397103, 12.90603908704162173, -1.500000000000002220 ) ) ;
#80463 = DIRECTION ( 'NONE',  ( -3.773278334453079030E-23, 0.9999999999976377785, 2.173523156925979128E-06 ) ) ;
#80464 = CARTESIAN_POINT ( 'NONE',  ( -18.32884136524465291, -7.267937366463995907, -1.500000000000002220 ) ) ;
#80465 = VECTOR ( 'NONE', #83500, 1000.000000000000000 ) ;
#80466 = CARTESIAN_POINT ( 'NONE',  ( 16.04643365539530109, -3.607965404481770832, -27.87003593022056691 ) ) ;
#80467 = COORDINATED_UNIVERSAL_TIME_OFFSET ( 0, 0, .AHEAD. ) ;
#80468 = DIRECTION ( 'NONE',  ( 3.773278334444166432E-23, -1.000000000000000000, 0.000000000000000000 ) ) ;
#80469 = CARTESIAN_POINT ( 'NONE',  ( -82.62287095715005592, -29.50248528299804818, 1.056150453629038477 ) ) ;
#80470 = CARTESIAN_POINT ( 'NONE',  ( 16.46467569749531634, 12.45148609503053017, 11.49999999999999645 ) ) ;
#80471 = PLANE ( 'NONE',  #67557 ) ;
#80472 = CARTESIAN_POINT ( 'NONE',  ( -19.30582015231555104, -11.89196067722419237, 11.49999999999999645 ) ) ;
#80473 = VERTEX_POINT ( 'NONE', #72569 ) ;
#80474 = CARTESIAN_POINT ( 'NONE',  ( -69.63000454671555417, -25.12219088186380134, 6.841411392149890247 ) ) ;
#80475 = DIRECTION ( 'NONE',  ( -3.773278334453079618E-23, 0.9999999999976377785, 2.173523156925979975E-06 ) ) ;
#80476 = EDGE_CURVE ( 'NONE', #36980, #47332, #47753, .T. ) ;
#80477 = CARTESIAN_POINT ( 'NONE',  ( -110.5228709571500616, -25.00158670708909625, 2.256160236439166411 ) ) ;
#80478 = FACE_OUTER_BOUND ( 'NONE', #89643, .T. ) ;
#80479 = VECTOR ( 'NONE', #60123, 1000.000000000000114 ) ;
#80480 = EDGE_LOOP ( 'NONE', ( #58457, #39681, #88360, #2386 ) ) ;
#80481 = FACE_OUTER_BOUND ( 'NONE', #16017, .T. ) ;
#80482 = CARTESIAN_POINT ( 'NONE',  ( -19.58686714514938387, 11.73587220785771379, 11.49999999999998934 ) ) ;
#80483 = DIRECTION ( 'NONE',  ( 0.000000000000000000, 1.478457507934778393E-16, -1.000000000000000000 ) ) ;
#80484 = CARTESIAN_POINT ( 'NONE',  ( -96.51075182989580981, -24.34968618360933945, 0.1864209137778868874 ) ) ;
#80485 = CARTESIAN_POINT ( 'NONE',  ( -82.55075552779136672, -24.15620529776628089, 10.23563542870660825 ) ) ;
#80486 = ADVANCED_FACE ( 'NONE', ( #64980 ), #80671, .F. ) ;
#80487 = CARTESIAN_POINT ( 'NONE',  ( -17.89120377161202313, 13.61666483413312712, 11.49999999999999645 ) ) ;
#80488 = ORIENTED_EDGE ( 'NONE', *, *, #86302, .T. ) ;
#80489 = CARTESIAN_POINT ( 'NONE',  ( -99.62287095715005592, -24.65952944569304961, 1.056160979905702124 ) ) ;
#80490 = CARTESIAN_POINT ( 'NONE',  ( -11.46427080702723522, -18.74017919159951973, -1.500000000000002220 ) ) ;
#80491 = EDGE_CURVE ( 'NONE', #67044, #42771, #6467, .T. ) ;
#80492 = CARTESIAN_POINT ( 'NONE',  ( -125.7765869487822670, -25.31326647857923007, 3.500947721614712016 ) ) ;
#80493 = AXIS2_PLACEMENT_3D ( 'NONE', #34034, #16294, #24905 ) ;
#80494 = CARTESIAN_POINT ( 'NONE',  ( -111.5203660093640678, -23.73766607897670511, -1.055555164236450461 ) ) ;
#80495 = CARTESIAN_POINT ( 'NONE',  ( 9.315600972258334167, 0.3587747205144265483, 28.35070303307545458 ) ) ;
#80496 = ORIENTED_EDGE ( 'NONE', *, *, #3878, .F. ) ;
#80497 = CARTESIAN_POINT ( 'NONE',  ( -48.55325661869351705, -23.96169478059713143, 10.65365249895718236 ) ) ;
#80498 = CARTESIAN_POINT ( 'NONE',  ( -107.5228709571500758, -23.47596703998600631, 11.44779298504228038 ) ) ;
#80499 = VERTEX_POINT ( 'NONE', #91277 ) ;
#80500 = VECTOR ( 'NONE', #30738, 1000.000000000000114 ) ;
#80501 = CARTESIAN_POINT ( 'NONE',  ( -54.65831064146149743, -23.48786465467240347, 11.44779295918255357 ) ) ;
#80502 = CARTESIAN_POINT ( 'NONE',  ( 20.32696876622996029, 2.630761579057304900, 11.49999999999998934 ) ) ;
#80503 = EDGE_LOOP ( 'NONE', ( #7299, #63168, #42740, #7843 ) ) ;
#80504 = CIRCLE ( 'NONE', #65979, 2.500000000000000444 ) ;
#80505 = ORIENTED_EDGE ( 'NONE', *, *, #28523, .T. ) ;
#80506 = ORIENTED_EDGE ( 'NONE', *, *, #73115, .F. ) ;
#80507 = CARTESIAN_POINT ( 'NONE',  ( -84.62287095715004170, -24.51283580621365132, 0.6167428607019797004 ) ) ;
#80508 = CARTESIAN_POINT ( 'NONE',  ( 6.910522817300494225, 22.03692736239173300, 11.49999999999998934 ) ) ;
#80510 = EDGE_CURVE ( 'NONE', #48044, #6944, #61042, .T. ) ;
#80509 = CARTESIAN_POINT ( 'NONE',  ( 14.63527791052757898, 4.349658986764157298, -28.08406249416238154 ) ) ;
#80511 = CARTESIAN_POINT ( 'NONE',  ( -18.95781532540867076, -7.450117396690965066, -1.500000000000002220 ) ) ;
#80512 = VERTEX_POINT ( 'NONE', #61345 ) ;
#80513 = CARTESIAN_POINT ( 'NONE',  ( -71.25388481961385878, -25.09966334678765421, 7.231536832813914906 ) ) ;
#80514 = CARTESIAN_POINT ( 'NONE',  ( -29.49548802756975974, -24.06924278478361856, 10.23563548314527338 ) ) ;
#80515 = AXIS2_PLACEMENT_3D ( 'NONE', #52850, #31504, #38618 ) ;
#80516 = DIRECTION ( 'NONE',  ( -2.338552693767719605E-15, 0.000000000000000000, 1.000000000000000000 ) ) ;
#80517 = CARTESIAN_POINT ( 'NONE',  ( -71.53177174497976409, -25.25855234727440646, 6.885843230737062726 ) ) ;
#80518 = ORIENTED_EDGE ( 'NONE', *, *, #53371, .T. ) ;
#80519 = CARTESIAN_POINT ( 'NONE',  ( -29.05456498926589504, -24.76881090259380613, 3.361080071346441933 ) ) ;
#80520 = CARTESIAN_POINT ( 'NONE',  ( -49.11003834631243592, -25.31573659134376442, 4.144493024849963625 ) ) ;
#80521 = ORIENTED_EDGE ( 'NONE', *, *, #1110, .F. ) ;
#80522 = CARTESIAN_POINT ( 'NONE',  ( -19.91680486407696904, 5.911688619927280008, -1.500000000000002220 ) ) ;
#80523 = VERTEX_POINT ( 'NONE', #21748 ) ;
#80524 = B_SPLINE_CURVE_WITH_KNOTS ( 'NONE', 3,
 ( #25109, #17508, #86516, #1790 ),
 .UNSPECIFIED., .F., .F.,
 ( 4, 4 ),
 ( 0.01303003236488493519, 0.01305095637151315775 ),
 .UNSPECIFIED. ) ;
#80526 = VERTEX_POINT ( 'NONE', #67956 ) ;
#80525 = CARTESIAN_POINT ( 'NONE',  ( -125.5196044704536007, -24.83618233451450763, 1.606449574219537046 ) ) ;
#80527 = LINE ( 'NONE', #95254, #8237 ) ;
#80528 = DIRECTION ( 'NONE',  ( 0.000000000000000000, -2.173523156925980399E-06, 0.9999999999976378895 ) ) ;
#80529 = ORIENTED_EDGE ( 'NONE', *, *, #18191, .T. ) ;
#80530 = ORIENTED_EDGE ( 'NONE', *, *, #70001, .T. ) ;
#80531 = CARTESIAN_POINT ( 'NONE',  ( -29.62287095715005947, -23.87211438191165058, -0.6496301950016380999 ) ) ;
#80532 = FACE_OUTER_BOUND ( 'NONE', #71097, .T. ) ;
#80534 = ADVANCED_FACE ( 'NONE', ( #77038 ), #6545, .T. ) ;
#80533 = CARTESIAN_POINT ( 'NONE',  ( -70.55843555340263151, -25.24515045242101507, 5.327474807685200098 ) ) ;
#80536 = ORIENTED_EDGE ( 'NONE', *, *, #35868, .F. ) ;
#80535 = CARTESIAN_POINT ( 'NONE',  ( 5.627179592841175193, 21.36305014179116668, 11.49999999999999645 ) ) ;
#80537 = CARTESIAN_POINT ( 'NONE',  ( -101.5228709571500758, -23.47596703998600631, 11.44779298504228215 ) ) ;
#80538 = CARTESIAN_POINT ( 'NONE',  ( 22.41689761077644860, -2.907977976681301424, 11.49999999999998934 ) ) ;
#80539 = CIRCLE ( 'NONE', #87046, 0.8160000000000007248 ) ;
#80541 = ORIENTED_EDGE ( 'NONE', *, *, #83324, .F. ) ;
#80540 = LINE ( 'NONE', #88665, #31231 ) ;
#80542 = EDGE_CURVE ( 'NONE', #19840, #66017, #97340, .T. ) ;
#80543 = EDGE_LOOP ( 'NONE', ( #92962, #65448, #5663, #53254 ) ) ;
#80544 = VECTOR ( 'NONE', #33757, 1000.000000000000114 ) ;
#80545 = DIRECTION ( 'NONE',  ( 0.000000000000000000, -0.9999999999976377785, -2.173523156925979128E-06 ) ) ;
#80546 = ADVANCED_FACE ( 'NONE', ( #68941 ), #36487, .T. ) ;
#80547 = CARTESIAN_POINT ( 'NONE',  ( -101.5468792378191978, -29.50249654204571215, 6.236241424690079249 ) ) ;
#80548 = ORIENTED_EDGE ( 'NONE', *, *, #64838, .T. ) ;
#80549 = CARTESIAN_POINT ( 'NONE',  ( -10.65520286329281596, -18.28862552182625123, -1.500000000000002220 ) ) ;
#80550 = FACE_OUTER_BOUND ( 'NONE', #31693, .T. ) ;
#80551 = LINE ( 'NONE', #42510, #67034 ) ;
#80552 = CARTESIAN_POINT ( 'NONE',  ( -40.49165087243459737, -25.29352311369862605, 5.543942880681965946 ) ) ;
#80553 = CARTESIAN_POINT ( 'NONE',  ( -19.85906585229243504, 9.992431322412627992, -1.500000000000002220 ) ) ;
#80554 = DIRECTION ( 'NONE',  ( 0.000000000000000000, -2.173523156925980399E-06, 0.9999999999976378895 ) ) ;
#80555 = B_SPLINE_CURVE_WITH_KNOTS ( 'NONE', 3,
 ( #15097, #76482, #7478, #60294, #29322, #6988 ),
 .UNSPECIFIED., .F., .F.,
 ( 4, 2, 4 ),
 ( 0.000000000000000000, 0.001380764517853254672, 0.002761529035706509344 ),
 .UNSPECIFIED. ) ;
#80556 = ORIENTED_EDGE ( 'NONE', *, *, #37843, .T. ) ;
#80557 = CARTESIAN_POINT ( 'NONE',  ( -110.5562042904834072, -23.47596703998600631, 11.44779298504227683 ) ) ;
#80558 = CARTESIAN_POINT ( 'NONE',  ( 31.82032313667048484, 0.3587747205144265483, 9.148483289431938559 ) ) ;
#80559 = CARTESIAN_POINT ( 'NONE',  ( -36.53861774053764577, -24.35071581493542325, 9.817618358456030592 ) ) ;
#80560 = B_SPLINE_CURVE_WITH_KNOTS ( 'NONE', 3,
 ( #37772, #30149, #98660, #75823 ),
 .UNSPECIFIED., .F., .F.,
 ( 4, 4 ),
 ( 0.4107933374670430515, 0.4197997687391585853 ),
 .UNSPECIFIED. ) ;
#80561 = DIRECTION ( 'NONE',  ( -3.773278334453079618E-23, 0.9999999999976377785, 2.173523156925979975E-06 ) ) ;
#80562 = CARTESIAN_POINT ( 'NONE',  ( 0.2958748881272694198, 19.47992435465491212, -1.500000000000002220 ) ) ;
#80563 = CARTESIAN_POINT ( 'NONE',  ( 15.25824911148008844, 15.06768998368162471, 11.49999999999998934 ) ) ;
#80564 = CARTESIAN_POINT ( 'NONE',  ( -0.7614568544629641833, -6.376774720514410077, 19.18727597066020962 ) ) ;
#80565 = CARTESIAN_POINT ( 'NONE',  ( -22.05275734969026047, -5.965225279485572685, 30.51402280011862089 ) ) ;
#80566 = CARTESIAN_POINT ( 'NONE',  ( -77.55884306925648275, -23.73766607897670156, -1.055555164236459564 ) ) ;
#80567 = CARTESIAN_POINT ( 'NONE',  ( 19.47892149737544187, 11.75266795981601753, -1.500000000000002220 ) ) ;
#80568 = ADVANCED_FACE ( 'NONE', ( #99866 ), #86434, .T. ) ;
#80569 = CARTESIAN_POINT ( 'NONE',  ( 22.02124265030972694, -19.69946567084332401, 16.20402280011846585 ) ) ;
#80570 = CARTESIAN_POINT ( 'NONE',  ( -98.62740225175618036, -24.34968618360934656, 0.1864209137778829184 ) ) ;
#80571 = DIRECTION ( 'NONE',  ( -0.000000000000000000, 1.000000000000000000, -0.000000000000000000 ) ) ;
#80572 = CARTESIAN_POINT ( 'NONE',  ( -6.132916590032589710, 18.96384228413732842, 11.49999999999999645 ) ) ;
#80573 = CARTESIAN_POINT ( 'NONE',  ( -69.52287095715006160, -24.65952944569304606, 1.056160979905697239 ) ) ;
#80574 = EDGE_CURVE ( 'NONE', #30754, #14223, #79186, .T. ) ;
#80575 = AXIS2_PLACEMENT_3D ( 'NONE', #90280, #5534, #36485 ) ;
#80576 = FACE_OUTER_BOUND ( 'NONE', #58989, .T. ) ;
#80577 = CARTESIAN_POINT ( 'NONE',  ( -48.53099033229920423, -24.65952944569304606, 1.056160979905697461 ) ) ;
#80578 = EDGE_LOOP ( 'NONE', ( #51061, #11389, #55839, #35452 ) ) ;
#80579 = DIRECTION ( 'NONE',  ( 3.773278334444167608E-23, -1.000000000000000000, 0.000000000000000000 ) ) ;
#80580 = CARTESIAN_POINT ( 'NONE',  ( -31.21621552302040925, -25.31558585043574183, 4.997857581739419075 ) ) ;
#80581 = CARTESIAN_POINT ( 'NONE',  ( -9.282276271697774916, -19.63344595494797673, 11.49999999999998934 ) ) ;
#80582 = ADVANCED_FACE ( 'NONE', ( #73325 ), #93703, .T. ) ;
#80583 = CARTESIAN_POINT ( 'NONE',  ( -51.33976102265904018, -25.09150690715527787, 7.330714471490653139 ) ) ;
#80584 = CARTESIAN_POINT ( 'NONE',  ( 6.866622826037362515, -18.30913693658520103, -1.500000000000002220 ) ) ;
#80585 = EDGE_CURVE ( 'NONE', #82122, #15222, #23754, .T. ) ;
#80586 = PLANE ( 'NONE',  #42622 ) ;
#80587 = ORIENTED_EDGE ( 'NONE', *, *, #27462, .F. ) ;
#80588 = COORDINATED_UNIVERSAL_TIME_OFFSET ( 0, 0, .AHEAD. ) ;
#80589 = DIRECTION ( 'NONE',  ( -3.773278334453079618E-23, 0.9999999999976377785, 2.173523156925979552E-06 ) ) ;
#80590 = CARTESIAN_POINT ( 'NONE',  ( -18.43012528856881715, -8.789534013050598560, 11.49999999999999645 ) ) ;
#80591 = CARTESIAN_POINT ( 'NONE',  ( -110.5562042904833930, -23.48783264082478794, -1.443836473390060160 ) ) ;
#80592 = FACE_OUTER_BOUND ( 'NONE', #35764, .T. ) ;
#80593 = ORIENTED_EDGE ( 'NONE', *, *, #73053, .F. ) ;
#80594 = CARTESIAN_POINT ( 'NONE',  ( 0.3910256410256441884, -6.376774720514427841, 21.75000000000000000 ) ) ;
#80595 = LINE ( 'NONE', #82097, #54225 ) ;
#80596 = PLANE ( 'NONE',  #55476 ) ;
#80597 = EDGE_CURVE ( 'NONE', #94573, #39942, #14935, .T. ) ;
#80598 = CARTESIAN_POINT ( 'NONE',  ( -109.5922554486619021, -23.96119346886880663, -0.6495511937832053606 ) ) ;
#80599 = VERTEX_POINT ( 'NONE', #54232 ) ;
#80600 = DIRECTION ( 'NONE',  ( 0.000000000000000000, 0.000000000000000000, 1.000000000000000000 ) ) ;
#80601 = VECTOR ( 'NONE', #52342, 1000.000000000000000 ) ;
#80602 = CARTESIAN_POINT ( 'NONE',  ( 11.31314246093949727, 19.96360691973900359, 11.49999999999999645 ) ) ;
#80603 = CARTESIAN_POINT ( 'NONE',  ( 2.720868037236281012, -22.60253418658637869, 11.49999999999998934 ) ) ;
#80604 = CARTESIAN_POINT ( 'NONE',  ( -110.5895321101819917, -24.52399227489125266, 9.353111116836528183 ) ) ;
#80605 = B_SPLINE_SURFACE_WITH_KNOTS ( 'NONE', 3, 1, ( 
 ( #92855, #86254 ),
 ( #15733, #62426 ),
 ( #78617, #85752 ),
 ( #16237, #47199 ),
 ( #16733, #47700 ),
 ( #37578, #60929 ),
 ( #68530, #29960 ) ),
 .UNSPECIFIED., .F., .F., .F.,
 ( 4, 1, 1, 1, 4 ),
 ( 2, 2 ),
 ( 0.000000000000000000, 0.2499864026691193120, 0.4969648798681425284, 0.7462659243093365813, 1.000000000000000000 ),
 ( 0.000000000000000000, 1.000000000000000000 ),
 .UNSPECIFIED. ) ;
#80606 = CARTESIAN_POINT ( 'NONE',  ( 33.74607884027702909, -5.965225279485572685, -4.999864028243830916 ) ) ;
#80607 = CARTESIAN_POINT ( 'NONE',  ( -90.49854698813747689, -25.00158670708910336, 2.256160236439220146 ) ) ;
#80608 = AXIS2_PLACEMENT_3D ( 'NONE', #64242, #41384, #33768 ) ;
#80609 = CARTESIAN_POINT ( 'NONE',  ( -54.52287095715011844, -23.73907113216988307, -1.053371485793257456 ) ) ;
#80610 = CARTESIAN_POINT ( 'NONE',  ( -93.62287095715007013, -23.47596703998600631, 11.44779298504227860 ) ) ;
#80611 = CARTESIAN_POINT ( 'NONE',  ( 6.672210613628693388, 20.84999943921648935, 11.49999999999998934 ) ) ;
#80612 = ADVANCED_FACE ( 'NONE', ( #39495 ), #932, .T. ) ;
#80613 = DIRECTION ( 'NONE',  ( 1.000000000000000000, -0.000000000000000000, 0.000000000000000000 ) ) ;
#80614 = EDGE_CURVE ( 'NONE', #97460, #74029, #92353, .T. ) ;
#80615 = CARTESIAN_POINT ( 'NONE',  ( -115.6228709571500701, -24.92579138211019796, 1.929029949965668456 ) ) ;
#80616 = DIRECTION ( 'NONE',  ( 3.773278334444165844E-23, -1.000000000000000000, 0.000000000000000000 ) ) ;
#80617 = CARTESIAN_POINT ( 'NONE',  ( 9.045332206306586187, -0.8999999999999998002, 3.697389739420775534 ) ) ;
#80618 = ORIENTED_EDGE ( 'NONE', *, *, #74619, .T. ) ;
#80619 = PRODUCT_DEFINITION_SHAPE ( 'NONE', 'NONE',  #3602 ) ;
#80620 = CARTESIAN_POINT ( 'NONE',  ( -6.584652030910324250, 19.34213596296284265, 11.49999999999998934 ) ) ;
#80621 = ORIENTED_EDGE ( 'NONE', *, *, #65289, .F. ) ;
#80622 = ORIENTED_EDGE ( 'NONE', *, *, #7319, .T. ) ;
#80623 = VERTEX_POINT ( 'NONE', #79044 ) ;
#80624 = CARTESIAN_POINT ( 'NONE',  ( 22.51966570110743149, 4.691836548664650053, 11.49999999999998934 ) ) ;
#80626 = EDGE_CURVE ( 'NONE', #85746, #35212, #50013, .T. ) ;
#80625 = CARTESIAN_POINT ( 'NONE',  ( -105.6228709571500559, -23.48783264082479150, -1.443836473390060160 ) ) ;
#80627 = CARTESIAN_POINT ( 'NONE',  ( -1.055277534996966970, 20.15608268182561247, -1.500000000000002220 ) ) ;
#80628 = ORIENTED_EDGE ( 'NONE', *, *, #12786, .F. ) ;
#80629 = CARTESIAN_POINT ( 'NONE',  ( -67.62287095715005592, -23.73934037231756733, 11.05740245334329330 ) ) ;
#80630 = AXIS2_PLACEMENT_3D ( 'NONE', #31400, #92788, #30393 ) ;
#80631 = CARTESIAN_POINT ( 'NONE',  ( -34.58953762381672448, -24.64965694238406613, 8.947790433994663672 ) ) ;
#80632 = EDGE_CURVE ( 'NONE', #61087, #8902, #12899, .T. ) ;
#80633 = EDGE_CURVE ( 'NONE', #19444, #42575, #44373, .T. ) ;
#80634 = CARTESIAN_POINT ( 'NONE',  ( -98.62287095715009855, -23.96177878511308990, 10.65340807706329684 ) ) ;
#80635 = CARTESIAN_POINT ( 'NONE',  ( -53.59900155969933877, -23.96169478059712787, 10.65365249895718591 ) ) ;
#80637 = ORIENTED_EDGE ( 'NONE', *, *, #96338, .F. ) ;
#80636 = CARTESIAN_POINT ( 'NONE',  ( 11.27511198983438412, 18.17944245918264912, 11.49999999999999645 ) ) ;
#80638 = FACE_OUTER_BOUND ( 'NONE', #3150, .T. ) ;
#80639 = VERTEX_POINT ( 'NONE', #90042 ) ;
#80640 = CARTESIAN_POINT ( 'NONE',  ( 22.17158117043571863, -1.905908075979310334, -1.500000000000002220 ) ) ;
#80641 = B_SPLINE_CURVE_WITH_KNOTS ( 'NONE', 3,
 ( #12157, #41130, #58358, #88300, #65485, #89794 ),
 .UNSPECIFIED., .F., .F.,
 ( 4, 2, 4 ),
 ( 1.570887131794176733E-05, 0.001396322306279758037, 0.002776935741241574537 ),
 .UNSPECIFIED. ) ;
#80642 = CARTESIAN_POINT ( 'NONE',  ( 20.01179378540625819, 5.277757631783551950, -1.500000000000002220 ) ) ;
#80643 = VECTOR ( 'NONE', #36843, 1000.000000000000000 ) ;
#80644 = VERTEX_POINT ( 'NONE', #27649 ) ;
#80645 = CARTESIAN_POINT ( 'NONE',  ( -6.185411026474866958, -6.376774720514411854, 19.34586827028016742 ) ) ;
#80646 = CARTESIAN_POINT ( 'NONE',  ( -68.92155128426668398, -25.30060019737137367, 6.009288023823078362 ) ) ;
#80647 = ORIENTED_EDGE ( 'NONE', *, *, #98783, .T. ) ;
#80648 = CARTESIAN_POINT ( 'NONE',  ( -78.94303308397304875, -25.27645460285955181, 5.977536667781793156 ) ) ;
#80649 = VECTOR ( 'NONE', #47240, 1000.000000000000000 ) ;
#80650 = EDGE_LOOP ( 'NONE', ( #24105, #46162, #23201, #24693 ) ) ;
#80651 = CARTESIAN_POINT ( 'NONE',  ( 9.422519371942208011, 6.475225279485576024, -27.03574706870085720 ) ) ;
#80652 = CARTESIAN_POINT ( 'NONE',  ( 5.463070048063013218, -20.23478146675526190, -1.500000000000002220 ) ) ;
#80653 = CARTESIAN_POINT ( 'NONE',  ( 1.548332177993611225, -21.85883989728069565, 11.49999999999999645 ) ) ;
#80654 = CARTESIAN_POINT ( 'NONE',  ( -107.6228709571500985, -23.96177878511308634, 10.65340807706329507 ) ) ;
#80655 = CARTESIAN_POINT ( 'NONE',  ( -6.794891441663577503, 21.43730618243864683, -1.500000000000002220 ) ) ;
#80656 = CARTESIAN_POINT ( 'NONE',  ( 18.03207908435136986, 10.65457695745678457, 11.49999999999998934 ) ) ;
#80657 = PLANE ( 'NONE',  #53023 ) ;
#80658 = DIRECTION ( 'NONE',  ( 0.000000000000000000, 1.000000000000000000, 0.000000000000000000 ) ) ;
#80659 = CARTESIAN_POINT ( 'NONE',  ( -91.52287095715006160, -24.64965694238575011, 8.947790433994196491 ) ) ;
#80660 = VERTEX_POINT ( 'NONE', #98631 ) ;
#80661 = ORIENTED_EDGE ( 'NONE', *, *, #72752, .T. ) ;
#80662 = ORIENTED_EDGE ( 'NONE', *, *, #91456, .T. ) ;
#80663 = CARTESIAN_POINT ( 'NONE',  ( -51.52287095715006870, -23.48786465467241058, 11.44779295918255002 ) ) ;
#80664 = VERTEX_POINT ( 'NONE', #36255 ) ;
#80665 = CARTESIAN_POINT ( 'NONE',  ( 14.52366289275476419, -15.72616519631134580, -1.500000000000002220 ) ) ;
#80666 = ORIENTED_EDGE ( 'NONE', *, *, #57032, .F. ) ;
#80667 = CARTESIAN_POINT ( 'NONE',  ( -26.09992617429942285, -24.95874029368170000, 5.209038662095228922 ) ) ;
#80668 = CARTESIAN_POINT ( 'NONE',  ( 19.72786461798894209, 7.474574171381012100, -1.500000000000002220 ) ) ;
#80669 = CARTESIAN_POINT ( 'NONE',  ( -30.42619003775230269, -24.66229007638825621, 8.908675929220798650 ) ) ;
#80670 = DIRECTION ( 'NONE',  ( -0.000000000000000000, -1.000000000000000000, -0.000000000000000000 ) ) ;
#80671 = PLANE ( 'NONE',  #42199 ) ;
#80672 = CARTESIAN_POINT ( 'NONE',  ( -101.5575534224985574, -23.73766607897671221, -1.055555164236452237 ) ) ;
#80673 = CARTESIAN_POINT ( 'NONE',  ( -129.6237316671312101, -23.96169478059714564, 10.65365249895717348 ) ) ;
#80674 = CARTESIAN_POINT ( 'NONE',  ( -18.71521858236628333, -11.60751834597489740, -1.500000000000002220 ) ) ;
#80675 = ORIENTED_EDGE ( 'NONE', *, *, #98511, .F. ) ;
#80676 = CARTESIAN_POINT ( 'NONE',  ( -116.5544677183481639, -24.15543982623908548, -0.2315651400026407236 ) ) ;
#80677 = DIRECTION ( 'NONE',  ( -3.773278334453079618E-23, 0.9999999999976377785, 2.173523156925979975E-06 ) ) ;
#80678 = CARTESIAN_POINT ( 'NONE',  ( 22.81105451610979173, -6.475225279485573360, -18.46691820600746681 ) ) ;
#80679 = AXIS2_PLACEMENT_3D ( 'NONE', #74913, #28758, #59721 ) ;
#80680 = CARTESIAN_POINT ( 'NONE',  ( -62.65464089196193243, -23.48786465467241413, 11.44779295918255002 ) ) ;
#80681 = B_SPLINE_CURVE_WITH_KNOTS ( 'NONE', 3,
 ( #3152, #12227, #57444, #67050, #12726, #27480 ),
 .UNSPECIFIED., .F., .F.,
 ( 4, 2, 4 ),
 ( 0.000000000000000000, 0.001380764517853249034, 0.002761529035706498068 ),
 .UNSPECIFIED. ) ;
#80682 = CARTESIAN_POINT ( 'NONE',  ( -25.53616547081472987, -24.90994025867288642, 4.571154658487995626 ) ) ;
#80683 = CARTESIAN_POINT ( 'NONE',  ( -79.62287095715005592, -29.50248528299804818, 1.056150453629038477 ) ) ;
#80684 = CARTESIAN_POINT ( 'NONE',  ( 19.59546714036918758, 8.467717511154198462, 11.49999999999998934 ) ) ;
#80685 = CARTESIAN_POINT ( 'NONE',  ( -97.62287095715001328, -24.51387760970724372, 9.387446482453411178 ) ) ;
#80686 = CARTESIAN_POINT ( 'NONE',  ( -51.94857094028245115, -25.30060005375479903, 6.009289253917323492 ) ) ;
#80687 = CARTESIAN_POINT ( 'NONE',  ( -0.1447603125146491310, -21.17596399598531676, 11.48393099501409687 ) ) ;
#80688 = CARTESIAN_POINT ( 'NONE',  ( -67.58953762381669605, -24.66019654487198665, 8.947790411086131712 ) ) ;
#80689 = CARTESIAN_POINT ( 'NONE',  ( -16.99934442671578694, -14.85117937636706031, -1.500000000000002220 ) ) ;
#80690 = EDGE_CURVE ( 'NONE', #47965, #2532, #37956, .T. ) ;
#80691 = B_SPLINE_CURVE_WITH_KNOTS ( 'NONE', 3,
 ( #80625, #58792, #49696, #33955 ),
 .UNSPECIFIED., .F., .F.,
 ( 4, 4 ),
 ( 0.000000000000000000, 9.999999999996123101E-05 ),
 .UNSPECIFIED. ) ;
#80692 = B_SPLINE_SURFACE_WITH_KNOTS ( 'NONE', 3, 3, ( 
 ( #15287, #29515, #46757, #77679 ),
 ( #69595, #23906, #61985, #14286 ),
 ( #60494, #53871, #91411, #31019 ),
 ( #46252, #30014, #92412, #92911 ),
 ( #77179, #31520, #8191, #39132 ),
 ( #22883, #23388, #22390, #76672 ),
 ( #62485, #7685, #53374, #93411 ) ),
 .UNSPECIFIED., .F., .F., .F.,
 ( 4, 3, 4 ),
 ( 4, 4 ),
 ( 0.3409880801055691912, 0.5103009464560217534, 0.6796138128064742601 ),
 ( 0.3860895931267444570, 0.4170344922427780543 ),
 .UNSPECIFIED. ) ;
#80693 = CARTESIAN_POINT ( 'NONE',  ( -47.52287095715004028, -24.51283580621461411, 0.6167428607048329736 ) ) ;
#80694 = EDGE_LOOP ( 'NONE', ( #20983, #71907, #9509, #14990 ) ) ;
#80695 = CARTESIAN_POINT ( 'NONE',  ( 30.53060340732036693, 4.132774720514426292, -2.322449884495168870 ) ) ;
#80696 = CARTESIAN_POINT ( 'NONE',  ( -79.58816022331352258, -24.34968618360933945, 0.1864209137778814473 ) ) ;
#80697 = CARTESIAN_POINT ( 'NONE',  ( 0.5484783294719396407, -19.75002165935583776, 11.49999999999999645 ) ) ;
#80698 = CARTESIAN_POINT ( 'NONE',  ( -49.52287095715006870, -23.72747288104469732, -1.053458166803227236 ) ) ;
#80700 = B_SPLINE_CURVE_WITH_KNOTS ( 'NONE', 3,
 ( #69509, #93330, #42616, #86228 ),
 .UNSPECIFIED., .F., .F.,
 ( 4, 4 ),
 ( 0.000000000000000000, 0.0001000000000000028644 ),
 .UNSPECIFIED. ) ;
#80699 = CARTESIAN_POINT ( 'NONE',  ( -67.56550939864793293, -23.48783264082477018, -1.443836473390094799 ) ) ;
#80701 = VERTEX_POINT ( 'NONE', #75796 ) ;
#80702 = CARTESIAN_POINT ( 'NONE',  ( -117.5228709571500758, -24.65952944569305316, 1.056160979905705899 ) ) ;
#80703 = CARTESIAN_POINT ( 'NONE',  ( -29.77605907665351737, -25.26026821586171422, 4.091748813052181966 ) ) ;
#80705 = EDGE_CURVE ( 'NONE', #61817, #40347, #1660, .T. ) ;
#80704 = CARTESIAN_POINT ( 'NONE',  ( -100.4426124108961176, -25.12268565766455808, 7.101635559697120570 ) ) ;
#80706 = CARTESIAN_POINT ( 'NONE',  ( -15.70146493180990888, -14.86199287721409590, 11.49999999999998934 ) ) ;
#80707 = EDGE_CURVE ( 'NONE', #14386, #37312, #43868, .T. ) ;
#80708 = CARTESIAN_POINT ( 'NONE',  ( -42.62287095715004881, -29.50248528299804818, 1.056150453629031594 ) ) ;
#80709 = AXIS2_PLACEMENT_3D ( 'NONE', #14544, #38883, #69845 ) ;
#80710 = CARTESIAN_POINT ( 'NONE',  ( -65.62287095715005592, -24.99156045073393173, 7.747789690856161648 ) ) ;
#80711 = EDGE_CURVE ( 'NONE', #62807, #42765, #65729, .T. ) ;
#80712 = CARTESIAN_POINT ( 'NONE',  ( -0.1490749075164066184, -21.12010817310450861, 11.44779298504228038 ) ) ;
#80713 = CARTESIAN_POINT ( 'NONE',  ( -4.444543648262984981, 12.92677669529668627, 0.000000000000000000 ) ) ;
#80714 = CARTESIAN_POINT ( 'NONE',  ( -18.42202159362721048, -7.168033771007030097, -1.500000000000002220 ) ) ;
#80715 = ORIENTED_EDGE ( 'NONE', *, *, #5596, .F. ) ;
#80716 = EDGE_CURVE ( 'NONE', #47332, #79914, #79105, .T. ) ;
#80717 = CARTESIAN_POINT ( 'NONE',  ( 20.05691770114479766, 3.104179615465487707, 11.49999999999999645 ) ) ;
#80718 = CARTESIAN_POINT ( 'NONE',  ( -7.627782137226129855, -5.876774720514414518, 20.04377961306771994 ) ) ;
#80719 = VECTOR ( 'NONE', #29969, 1000.000000000000000 ) ;
#80720 = ORIENTED_EDGE ( 'NONE', *, *, #83499, .T. ) ;
#80721 = CARTESIAN_POINT ( 'NONE',  ( 26.73860345374794534, 5.058662225110310828, -7.113848178280766099 ) ) ;
#80722 = CARTESIAN_POINT ( 'NONE',  ( -110.6228709571500559, -24.99132157543166954, 2.256160258750667502 ) ) ;
#80723 = CARTESIAN_POINT ( 'NONE',  ( -8.676776695296460673, 18.57322330470351091, 2.100000000000000089 ) ) ;
#80724 = LINE ( 'NONE', #88842, #46903 ) ;
#80725 = VECTOR ( 'NONE', #95447, 1000.000000000000000 ) ;
#80726 = CARTESIAN_POINT ( 'NONE',  ( -103.6228709571500701, -24.33927499327855060, 9.819080762295817166 ) ) ;
#80727 = CARTESIAN_POINT ( 'NONE',  ( -86.52287095715006160, -24.66019654487199375, 8.947790411086119278 ) ) ;
#80728 = CARTESIAN_POINT ( 'NONE',  ( -5.935188749463110369, 19.13178230186815298, -1.500000000000002220 ) ) ;
#80729 = EDGE_CURVE ( 'NONE', #66603, #17632, #6294, .T. ) ;
#80730 = CARTESIAN_POINT ( 'NONE',  ( -76.62287095715007013, -24.64898659630367916, 1.056161002820826145 ) ) ;
#80731 = VERTEX_POINT ( 'NONE', #89540 ) ;
#80732 = ADVANCED_FACE ( 'NONE', ( #50990 ), #13397, .T. ) ;
#80733 = AXIS2_PLACEMENT_3D ( 'NONE', #15438, #62636, #79339 ) ;
#80734 = DIRECTION ( 'NONE',  ( -1.000000000000000000, 0.000000000000000000, 0.000000000000000000 ) ) ;
#80735 = PLANE ( 'NONE',  #15363 ) ;
#80736 = DIRECTION ( 'NONE',  ( 0.000000000000000000, 0.000000000000000000, -1.000000000000000000 ) ) ;
#80737 = DIRECTION ( 'NONE',  ( 0.000000000000000000, 4.336808689942019708E-16, -1.000000000000000000 ) ) ;
#80738 = CARTESIAN_POINT ( 'NONE',  ( -73.55409649099257763, -23.96119346886880663, -0.6495511937832116889 ) ) ;
#80739 = EDGE_CURVE ( 'NONE', #16861, #100167, #77821, .T. ) ;
#80740 = CARTESIAN_POINT ( 'NONE',  ( 14.66599494348427335, 4.455096676454847859, -28.01208847159952597 ) ) ;
#80741 = CARTESIAN_POINT ( 'NONE',  ( -49.98787894874461557, -25.19317122439448653, 3.352862466847235545 ) ) ;
#80742 = ORIENTED_EDGE ( 'NONE', *, *, #74867, .F. ) ;
#80743 = CARTESIAN_POINT ( 'NONE',  ( 9.809556900635294951, 17.81656380412256269, -1.500000000000002220 ) ) ;
#80744 = VERTEX_POINT ( 'NONE', #67718 ) ;
#80745 = CARTESIAN_POINT ( 'NONE',  ( -5.713817535623205046, 22.21719745612757535, -1.500000000000002220 ) ) ;
#80746 = EDGE_CURVE ( 'NONE', #19840, #80599, #28145, .T. ) ;
#80747 = CARTESIAN_POINT ( 'NONE',  ( 31.63284457977613684, 3.861502214243257125, 27.22238481897691287 ) ) ;
#80748 = CARTESIAN_POINT ( 'NONE',  ( -127.6245371603278755, -23.73791477778912551, 11.05961554403169345 ) ) ;
#80749 = VERTEX_POINT ( 'NONE', #11913 ) ;
#80750 = CARTESIAN_POINT ( 'NONE',  ( -49.10837252249681484, -25.27212926941085769, 4.099823236261497250 ) ) ;
#80751 = EDGE_CURVE ( 'NONE', #7479, #50183, #59104, .T. ) ;
#80752 = B_SPLINE_CURVE_WITH_KNOTS ( 'NONE', 3,
 ( #83962, #60153, #75843, #45414 ),
 .UNSPECIFIED., .F., .F.,
 ( 4, 4 ),
 ( 0.4891186356891960019, 0.4901193827299611394 ),
 .UNSPECIFIED. ) ;
#80753 = CARTESIAN_POINT ( 'NONE',  ( -49.27841808360716414, -25.12215218622909418, 6.176813154470331746 ) ) ;
#80754 = B_SPLINE_CURVE_WITH_KNOTS ( 'NONE', 3,
 ( #48502, #87044, #63741, #55109 ),
 .UNSPECIFIED., .F., .F.,
 ( 4, 4 ),
 ( 0.000000000000000000, 9.999999999998206125E-05 ),
 .UNSPECIFIED. ) ;
#80755 = CARTESIAN_POINT ( 'NONE',  ( -66.62287095715005592, -24.64965695001468404, 8.947790433994184056 ) ) ;
#80756 = CARTESIAN_POINT ( 'NONE',  ( -19.98547761299008130, 7.154247560337752887, 11.49999999999999645 ) ) ;
#80757 = CARTESIAN_POINT ( 'NONE',  ( -5.973063517705734071, 21.31661749205449041, 11.49999999999998934 ) ) ;
#80758 = EDGE_CURVE ( 'NONE', #86899, #30864, #82700, .T. ) ;
#80759 = CARTESIAN_POINT ( 'NONE',  ( 13.11803791274172681, -15.88952355948706341, 11.49999999999998934 ) ) ;
#80760 = ORIENTED_EDGE ( 'NONE', *, *, #92459, .T. ) ;
#80761 = CARTESIAN_POINT ( 'NONE',  ( -28.84663072490566194, 0.3587747205144265483, 28.73989617533406715 ) ) ;
#80762 = VERTEX_POINT ( 'NONE', #20510 ) ;
#80763 = DIRECTION ( 'NONE',  ( 0.000000000000000000, 2.173523156925980399E-06, -0.9999999999976378895 ) ) ;
#80764 = DIRECTION ( 'NONE',  ( 0.000000000000000000, -0.9999999999976377785, -2.173523156925979975E-06 ) ) ;
#80765 = ORIENTED_EDGE ( 'NONE', *, *, #17952, .T. ) ;
#80766 = VERTEX_POINT ( 'NONE', #31623 ) ;
#80767 = ORIENTED_EDGE ( 'NONE', *, *, #80387, .T. ) ;
#80768 = DIRECTION ( 'NONE',  ( -0.000000000000000000, -1.000000000000000000, 0.000000000000000000 ) ) ;
#80769 = DIRECTION ( 'NONE',  ( -0.000000000000000000, -1.000000000000000000, -0.000000000000000000 ) ) ;
#80770 = CARTESIAN_POINT ( 'NONE',  ( 5.963731207934512391, -6.376774720514413630, 19.80418863844947097 ) ) ;
#80771 = CARTESIAN_POINT ( 'NONE',  ( -5.954758479537505700, 19.85987847461844424, -1.500000000000002220 ) ) ;
#80772 = CARTESIAN_POINT ( 'NONE',  ( 14.13103794885040898, -16.47871000921984219, 11.49999999999999645 ) ) ;
#80773 = ORIENTED_EDGE ( 'NONE', *, *, #43144, .T. ) ;
#80774 = LINE ( 'NONE', #10762, #48273 ) ;
#80775 = CARTESIAN_POINT ( 'NONE',  ( -105.5228709571500758, -23.47593901973090524, -1.443836447538996426 ) ) ;
#80776 = CARTESIAN_POINT ( 'NONE',  ( 22.22467975111640470, 2.813832150844377100, 11.49999999999998934 ) ) ;
#80777 = AXIS2_PLACEMENT_3D ( 'NONE', #19062, #41927, #80468 ) ;
#80778 = B_SPLINE_CURVE_WITH_KNOTS ( 'NONE', 3,
 ( #8323, #32155, #47396, #85439 ),
 .UNSPECIFIED., .F., .F.,
 ( 4, 4 ),
 ( 0.000000000000000000, 1.000000000000000000 ),
 .UNSPECIFIED. ) ;
#80779 = CARTESIAN_POINT ( 'NONE',  ( -79.62287095715004170, -24.65952944569304606, 1.056160979905697461 ) ) ;
#80780 = CARTESIAN_POINT ( 'NONE',  ( -121.5228709571500616, -24.64965694238408034, 8.947790433994191162 ) ) ;
#80781 = ORIENTED_EDGE ( 'NONE', *, *, #25925, .F. ) ;
#80782 = CARTESIAN_POINT ( 'NONE',  ( -32.52287095715006160, -24.65952944569304606, 1.056160979905690134 ) ) ;
#80783 = CARTESIAN_POINT ( 'NONE',  ( -119.4728709548940628, -25.21112548385455199, 2.000950964958121414 ) ) ;
#80784 = ORIENTED_EDGE ( 'NONE', *, *, #13828, .F. ) ;
#80785 = ORIENTED_EDGE ( 'NONE', *, *, #95524, .T. ) ;
#80786 = CARTESIAN_POINT ( 'NONE',  ( -38.62287095715005592, -29.50248528299804818, 1.056150453629031594 ) ) ;
#80787 = VERTEX_POINT ( 'NONE', #92520 ) ;
#80788 = CARTESIAN_POINT ( 'NONE',  ( 12.23393567461250697, 17.36540613969008007, -1.500000000000002220 ) ) ;
#80789 = B_SPLINE_CURVE_WITH_KNOTS ( 'NONE', 3,
 ( #22744, #53728, #98882, #84659 ),
 .UNSPECIFIED., .F., .F.,
 ( 4, 4 ),
 ( 0.9904932114349886962, 1.000000000000000000 ),
 .UNSPECIFIED. ) ;
#80790 = VERTEX_POINT ( 'NONE', #23491 ) ;
#80791 = CARTESIAN_POINT ( 'NONE',  ( -88.62358598722710212, -24.65952944569304606, 1.056160979905700126 ) ) ;
#80792 = CARTESIAN_POINT ( 'NONE',  ( 4.989390281198801347, -21.28523531580253803, 11.49999999999998934 ) ) ;
#80793 = DIRECTION ( 'NONE',  ( 0.000000000000000000, -0.9999999999976377785, -2.173523156925979975E-06 ) ) ;
#80794 = AXIS2_PLACEMENT_3D ( 'NONE', #92818, #17201, #93318 ) ;
#80795 = CARTESIAN_POINT ( 'NONE',  ( 33.96422015159436114, -5.965225279485572685, -7.233236000911337449 ) ) ;
#80796 = CARTESIAN_POINT ( 'NONE',  ( -35.62287095715006302, -24.91544648472620338, 1.928969306349229695 ) ) ;
#80797 = CARTESIAN_POINT ( 'NONE',  ( 11.25260618158950621, 18.78031238747207610, -1.500000000000002220 ) ) ;
#80798 = FACE_OUTER_BOUND ( 'NONE', #10385, .T. ) ;
#80799 = EDGE_LOOP ( 'NONE', ( #88115, #44438, #61653, #69915 ) ) ;
#80800 = CARTESIAN_POINT ( 'NONE',  ( -65.62287095715004170, -24.92579138211018375, 1.929029949965667123 ) ) ;
#80801 = CARTESIAN_POINT ( 'NONE',  ( -73.55620429048339304, -24.64898659630528854, 1.056161002820822592 ) ) ;
#80802 = ORIENTED_EDGE ( 'NONE', *, *, #5680, .F. ) ;
#80803 = FACE_OUTER_BOUND ( 'NONE', #30705, .T. ) ;
#80804 = AXIS2_PLACEMENT_3D ( 'NONE', #19804, #29418, #98422 ) ;
#80805 = ORIENTED_EDGE ( 'NONE', *, *, #88971, .T. ) ;
#80806 = CARTESIAN_POINT ( 'NONE',  ( 11.44401587981593060, 6.475225279485572472, -27.05278809890034353 ) ) ;
#80807 = CARTESIAN_POINT ( 'NONE',  ( -20.48352739510140452, -22.69081920706126354, -1.443836447538997314 ) ) ;
#80808 = CARTESIAN_POINT ( 'NONE',  ( -20.90244970016518877, -3.954922567530639199, -1.500000000000002220 ) ) ;
#80809 = CARTESIAN_POINT ( 'NONE',  ( -118.6228709571500559, -29.50250786944525672, 11.44777988621622811 ) ) ;
#80810 = CARTESIAN_POINT ( 'NONE',  ( 22.02124265030973760, -4.543225279485573864, 16.20402280011862217 ) ) ;
#80811 = CARTESIAN_POINT ( 'NONE',  ( -85.49691536098328015, -24.92564183028979485, 1.928384488918252204 ) ) ;
#80812 = CARTESIAN_POINT ( 'NONE',  ( -68.53708757987610056, -24.65952944569304606, 1.056160979905701236 ) ) ;
#80813 = CARTESIAN_POINT ( 'NONE',  ( 10.09180897563621926, 16.61094848277074476, -1.500000000000002220 ) ) ;
#80814 = CARTESIAN_POINT ( 'NONE',  ( -45.53467254122168839, -24.63355581998386867, 0.9682620441943888823 ) ) ;
#80815 = ORIENTED_EDGE ( 'NONE', *, *, #82193, .T. ) ;
#80816 = EDGE_CURVE ( 'NONE', #27205, #1265, #45156, .T. ) ;
#80817 = CARTESIAN_POINT ( 'NONE',  ( 11.58774116221665729, 15.72987433093905096, 11.49999999999999645 ) ) ;
#80818 = CARTESIAN_POINT ( 'NONE',  ( 31.62416306531753918, -4.295372699094516022, 26.87458401151571508 ) ) ;
#80819 = ADVANCED_FACE ( 'NONE', ( #60604 ), #29206, .T. ) ;
#80820 = CARTESIAN_POINT ( 'NONE',  ( -116.5228709571500616, -23.48786465467241769, 11.44779295918253759 ) ) ;
#80821 = ORIENTED_EDGE ( 'NONE', *, *, #46551, .F. ) ;
#80822 = EDGE_CURVE ( 'NONE', #39625, #22949, #45861, .T. ) ;
#80823 = CARTESIAN_POINT ( 'NONE',  ( -97.62287095715005592, -24.64898659630367916, 1.056161002820829697 ) ) ;
#80824 = CARTESIAN_POINT ( 'NONE',  ( -89.58846763882705488, -24.34968618360933945, 0.1864209137778942982 ) ) ;
#80825 = EDGE_CURVE ( 'NONE', #51581, #75656, #92024, .T. ) ;
#80826 = LINE ( 'NONE', #48379, #63394 ) ;
#80827 = LINE ( 'NONE', #27037, #26663 ) ;
#80828 = CARTESIAN_POINT ( 'NONE',  ( -8.027368788987615744, 17.96763083595211441, 11.49999999999998934 ) ) ;
#80829 = ORIENTED_EDGE ( 'NONE', *, *, #26862, .F. ) ;
#80830 = CARTESIAN_POINT ( 'NONE',  ( -7.357004447969931249, -10.77121780415746954, 1.154761385154455144 ) ) ;
#80831 = LINE ( 'NONE', #51378, #67407 ) ;
#80833 = EDGE_CURVE ( 'NONE', #44429, #31086, #3994, .T. ) ;
#80832 = COORDINATED_UNIVERSAL_TIME_OFFSET ( 0, 0, .AHEAD. ) ;
#80834 = ORIENTED_EDGE ( 'NONE', *, *, #55978, .T. ) ;
#80835 = FACE_OUTER_BOUND ( 'NONE', #80578, .T. ) ;
#80836 = CARTESIAN_POINT ( 'NONE',  ( -126.5228709571500616, -23.47593901973090524, -1.443836447538996204 ) ) ;
#80837 = CARTESIAN_POINT ( 'NONE',  ( -105.5228709571500758, -23.47593901973090524, -1.443836447538996426 ) ) ;
#80838 = DIRECTION ( 'NONE',  ( -1.000000000000000000, -3.773278334444166432E-23, -8.201307841325785021E-29 ) ) ;
#80839 = CARTESIAN_POINT ( 'NONE',  ( -80.91152895311172699, -25.20144873054373136, 6.835696071488102099 ) ) ;
#80840 = VECTOR ( 'NONE', #59393, 1000.000000000000227 ) ;
#80841 = AXIS2_PLACEMENT_3D ( 'NONE', #31494, #14759, #69569 ) ;
#80842 = PLANE ( 'NONE',  #58659 ) ;
#80843 = DIRECTION ( 'NONE',  ( 3.773278334444167608E-23, -1.000000000000000000, 0.000000000000000000 ) ) ;
#80844 = CARTESIAN_POINT ( 'NONE',  ( 6.088051586893210576, -19.00464151315268424, -1.500000000000002220 ) ) ;
#80845 = CARTESIAN_POINT ( 'NONE',  ( 31.59111626279633711, 5.965225279485572685, 16.27760796525321751 ) ) ;
#80846 = CARTESIAN_POINT ( 'NONE',  ( -19.08307359429613825, -5.530936995296134917, -1.500000000000002220 ) ) ;
#80847 = VERTEX_POINT ( 'NONE', #46858 ) ;
#80848 = VECTOR ( 'NONE', #93965, 1000.000000000000114 ) ;
#80849 = CARTESIAN_POINT ( 'NONE',  ( -120.5228709571501184, -23.48783264082477373, -1.443836473390081698 ) ) ;
#80850 = CARTESIAN_POINT ( 'NONE',  ( 1.949999999999999956, 0.1924999999999999489, 0.1925000000000000044 ) ) ;
#80851 = DIRECTION ( 'NONE',  ( 0.000000000000000000, 0.000000000000000000, -1.000000000000000000 ) ) ;
#80852 = CARTESIAN_POINT ( 'NONE',  ( 1.081820405348005165, -20.78239343107542680, 11.49999999999999645 ) ) ;
#80853 = CARTESIAN_POINT ( 'NONE',  ( -7.491187506528125262, -5.876774720514410077, 19.53857357749109980 ) ) ;
#80854 = AXIS2_PLACEMENT_3D ( 'NONE', #49411, #86948, #33160 ) ;
#80855 = DIRECTION ( 'NONE',  ( -1.000000000000000000, 0.000000000000000000, -0.000000000000000000 ) ) ;
#80856 = CARTESIAN_POINT ( 'NONE',  ( 5.898633191892585614, -22.09092271590295198, 11.49999999999999645 ) ) ;
#80857 = ORIENTED_EDGE ( 'NONE', *, *, #58941, .T. ) ;
#80858 = CARTESIAN_POINT ( 'NONE',  ( -55.22287095715007155, -23.47593901973090169, -1.443836447538997758 ) ) ;
#80859 = FACE_OUTER_BOUND ( 'NONE', #74441, .T. ) ;
#80860 = VERTEX_POINT ( 'NONE', #83916 ) ;
#80861 = CIRCLE ( 'NONE', #85714, 6.594667762285751245 ) ;
#80862 = CARTESIAN_POINT ( 'NONE',  ( 15.69265952521009488, -12.80212094623039576, 11.49999999999998934 ) ) ;
#80863 = CARTESIAN_POINT ( 'NONE',  ( -29.49875734969025842, -5.965225279485572685, 25.61802280011862720 ) ) ;
#80864 = FACE_OUTER_BOUND ( 'NONE', #43113, .T. ) ;
#80865 = CARTESIAN_POINT ( 'NONE',  ( -100.6228709571500417, -24.92579138211020151, 1.929029949965661572 ) ) ;
#80867 = ORIENTED_EDGE ( 'NONE', *, *, #22011, .F. ) ;
#80866 = ADVANCED_FACE ( 'NONE', ( #14395, #14893 ), #53490, .F. ) ;
#80868 = CARTESIAN_POINT ( 'NONE',  ( -79.46841724574004218, -25.31402286304979299, 4.799853472881489225 ) ) ;
#80869 = DIRECTION ( 'NONE',  ( 5.328431011793917330E-15, 0.000000000000000000, 1.000000000000000000 ) ) ;
#80870 = CARTESIAN_POINT ( 'NONE',  ( -17.52916707085001136, 9.785066945116392745, -1.500000000000002220 ) ) ;
#80871 = CARTESIAN_POINT ( 'NONE',  ( 7.388015978253313243, 19.69965359013245632, 11.49999999999999645 ) ) ;
#80872 = CARTESIAN_POINT ( 'NONE',  ( -29.51986997226218534, -25.07943211551384977, 6.939773859971299252 ) ) ;
#80873 = DIRECTION ( 'NONE',  ( -1.000000000000000000, -0.000000000000000000, -0.000000000000000000 ) ) ;
#80874 = CARTESIAN_POINT ( 'NONE',  ( 20.57837473233041692, -7.934362236255416256, 11.49999999999998934 ) ) ;
#80875 = EDGE_CURVE ( 'NONE', #64365, #24606, #45376, .T. ) ;
#80876 = CARTESIAN_POINT ( 'NONE',  ( -39.59566294291796140, -25.27806020191125214, 4.684364630645174721 ) ) ;
#80877 = CLOSED_SHELL ( 'NONE', ( #1910, #92787, #84652, #53974, #26051, #45781, #34373, #98017, #20662, #80252, #31646, #37733, #41180, #55843, #9446, #56864, #82899, #27569, #72945, #80986, #88383, #99523, #68833, #92213, #27096, #50716, #15985, #55219, #88629, #7517, #37861, #51615, #50791, #73289, #38084, #8231, #16074, #30367, #75123, #8429, #59525, #20387, #5536, #22539, #51390, #96279, #65947, #1451, #19295, #74311, #8806, #96641, #11283, #41940, #84264, #54827, #12705, #18150, #57168, #76065, #46578, #3524, #100413, #94224, #14410, #10204, #81825, #8416, #64320, #76379, #83702, #91263, #70040, #69497, #8104, #83508, #800, #88263, #54409, #38415, #39664, #4662, #32044, #19102, #42763, #22806, #49239, #7444, #41690, #72722, #95711, #55852, #48990, #94797, #72236, #30408, #67894, #12934, #64373, #72481, #71546, #16654, #86557, #3166, #54964, #57373, #88572, #22917, #14288, #57728, #38817, #84497, #91028, #31796, #74732, #60680, #19984, #49661, #75623, #83081, #68388, #77935, #16419, #69508, #86814, #4707, #37212, #100192, #49129, #55728, #76172, #97656, #44987, #54507, #31259, #80945, #87815, #62445, #73298, #74071, #28806, #64426, #50910, #9319, #10384, #57274, #50610, #48530, #10715, #21137, #60263, #80114, #77520, #19225, #87454, #91253, #64415, #47698, #15635, #96770, #93299, #1897, #88849, #60262, #83218, #28691, #6839, #16543, #24278, #19655, #70332, #45178, #43771, #53849, #21803, #29135, #52417, #69261, #90464, #72231, #39485, #97268, #28182, #49590, #19723, #82259, #75106, #83810, #48325, #75371, #64538, #11348, #38647, #73615, #55568, #99026, #33628, #52647, #26643, #34221, #75748, #72011, #84958, #83047, #18208, #19339, #67899, #91398, #22609, #26858, #60774, #53053, #64634, #28147, #68450, #58610, #39835, #35874, #5906, #34811, #88843, #52075, #21667, #95951, #32649, #12242, #54390, #54594, #68096, #10721, #22947, #58520, #12087, #98094, #54463, #99730, #88610, #17135, #53359, #41085, #37275, #76254, #43590, #32720, #84279, #37143, #82362, #12001, #81883, #6356, #11268, #85162, #36938, #41897, #60222, #39567, #67533, #2520, #22534, #21516, #99463, #68900, #8423, #17245, #57121, #7851, #82668, #58055, #14806, #46569, #22056, #39361, #54702, #28759, #20681, #84469, #83512, #80036, #95772, #68455, #54074, #73849, #18569 ) ) ;
#80878 = LINE ( 'NONE', #26595, #45202 ) ;
#80879 = CARTESIAN_POINT ( 'NONE',  ( 31.79364159983995464, 5.965225279485572685, -11.59305536555894278 ) ) ;
#80880 = CARTESIAN_POINT ( 'NONE',  ( 6.660000000000001030, -2.191226316053958875E-18, 2.701633758479787833E-17 ) ) ;
#80881 = CARTESIAN_POINT ( 'NONE',  ( -31.52580767185885691, -24.65952944569304250, 1.056160979905695463 ) ) ;
#80882 = ORIENTED_EDGE ( 'NONE', *, *, #57250, .F. ) ;
#80883 = ORIENTED_EDGE ( 'NONE', *, *, #21166, .T. ) ;
#80884 = CARTESIAN_POINT ( 'NONE',  ( 30.09341516180546350, 1.477225279485574028, -11.39311774897855933 ) ) ;
#80885 = DIRECTION ( 'NONE',  ( -0.000000000000000000, -0.000000000000000000, -1.000000000000000000 ) ) ;
#80886 = CARTESIAN_POINT ( 'NONE',  ( -94.62287095715004170, -23.72773821059536559, 11.05748984161097681 ) ) ;
#80887 = CARTESIAN_POINT ( 'NONE',  ( 4.502618398017903090, 20.03723546437915104, -1.500000000000002220 ) ) ;
#80888 = VERTEX_POINT ( 'NONE', #84415 ) ;
#80889 = DIRECTION ( 'NONE',  ( -1.000000000000000000, 0.000000000000000000, 0.000000000000000000 ) ) ;
#80890 = CARTESIAN_POINT ( 'NONE',  ( 11.56983764158150407, 0.3587747205144265483, 28.29037853177889517 ) ) ;
#80891 = CARTESIAN_POINT ( 'NONE',  ( -69.52287095715006160, -29.50250786944525672, 11.44777988621623699 ) ) ;
#80892 = CARTESIAN_POINT ( 'NONE',  ( -20.55042600948665310, 8.738301046694649798, 11.49999999999998934 ) ) ;
#80893 = DIRECTION ( 'NONE',  ( 0.000000000000000000, 0.000000000000000000, 1.000000000000000000 ) ) ;
#80894 = CARTESIAN_POINT ( 'NONE',  ( -121.9228709571500673, -23.47596703998600631, 11.44779298504227683 ) ) ;
#80895 = EDGE_LOOP ( 'NONE', ( #9076, #42873, #16609, #34308 ) ) ;
#80896 = CARTESIAN_POINT ( 'NONE',  ( -96.62287095715005592, -23.48783264082478794, -1.443836473390061936 ) ) ;
#80897 = CARTESIAN_POINT ( 'NONE',  ( -47.62287095715006302, -23.47596703998600276, 11.44779298504227505 ) ) ;
#80898 = CARTESIAN_POINT ( 'NONE',  ( -19.85847575633505713, -6.422239212204448044, 11.49999999999998934 ) ) ;
#80899 = ORIENTED_EDGE ( 'NONE', *, *, #49694, .F. ) ;
#80901 = VERTEX_POINT ( 'NONE', #77285 ) ;
#80900 = DIRECTION ( 'NONE',  ( -0.000000000000000000, -1.000000000000000000, -0.000000000000000000 ) ) ;
#80902 = ORIENTED_EDGE ( 'NONE', *, *, #80942, .T. ) ;
#80903 = CARTESIAN_POINT ( 'NONE',  ( -68.98049337452070517, -25.25935131006976064, 6.552244419545522724 ) ) ;
#80904 = CARTESIAN_POINT ( 'NONE',  ( -20.97943885474387216, 2.004451313549292735, -1.500000000000002220 ) ) ;
#80905 = ORIENTED_EDGE ( 'NONE', *, *, #2477, .F. ) ;
#80906 = DIRECTION ( 'NONE',  ( 1.000000000000000000, 0.000000000000000000, 0.000000000000000000 ) ) ;
#80907 = DIRECTION ( 'NONE',  ( 0.000000000000000000, 0.000000000000000000, -1.000000000000000000 ) ) ;
#80908 = CARTESIAN_POINT ( 'NONE',  ( -120.5888102207224790, -24.73531770709095312, 8.716586749053508498 ) ) ;
#80909 = VECTOR ( 'NONE', #67460, 1000.000000000000000 ) ;
#80910 = CARTESIAN_POINT ( 'NONE',  ( -2.749999999999999112, 27.59999999999999432, 2.100000000000000089 ) ) ;
#80911 = PLANE ( 'NONE',  #28752 ) ;
#80912 = CARTESIAN_POINT ( 'NONE',  ( -10.61912389536305490, -18.88692380039396213, -1.500000000000002220 ) ) ;
#80913 = CARTESIAN_POINT ( 'NONE',  ( -81.22562555205841761, -25.24759741702468219, 6.810744828488381586 ) ) ;
#80915 = ORIENTED_EDGE ( 'NONE', *, *, #92398, .T. ) ;
#80914 = CARTESIAN_POINT ( 'NONE',  ( 10.43072250204971851, -19.66636941823637841, 11.49999999999999645 ) ) ;
#80916 = LINE ( 'NONE', #95645, #35650 ) ;
#80917 = CARTESIAN_POINT ( 'NONE',  ( -95.62287095715007013, -23.48786465467241769, 11.44779295918254114 ) ) ;
#80918 = FACE_OUTER_BOUND ( 'NONE', #13473, .T. ) ;
#80919 = EDGE_LOOP ( 'NONE', ( #61083, #38461, #25633, #59718 ) ) ;
#80920 = VECTOR ( 'NONE', #28111, 1000.000000000000000 ) ;
#80922 = ORIENTED_EDGE ( 'NONE', *, *, #63921, .T. ) ;
#80921 = DIRECTION ( 'NONE',  ( -1.000000000000000000, -3.491481338843133355E-15, -2.352173255807796056E-16 ) ) ;
#80923 = AXIS2_PLACEMENT_3D ( 'NONE', #78222, #54405, #10229 ) ;
#80924 = ORIENTED_EDGE ( 'NONE', *, *, #30525, .F. ) ;
#80925 = B_SPLINE_CURVE_WITH_KNOTS ( 'NONE', 3,
 ( #22148, #13047, #98278, #92172 ),
 .UNSPECIFIED., .F., .F.,
 ( 4, 4 ),
 ( 0.000000000000000000, 0.0004038461538461851630 ),
 .UNSPECIFIED. ) ;
#80926 = CIRCLE ( 'NONE', #48566, 11.85241003308275864 ) ;
#80927 = DIRECTION ( 'NONE',  ( -0.9831680378442393398, 0.000000000000000000, -0.1827036106964188000 ) ) ;
#80928 = CARTESIAN_POINT ( 'NONE',  ( -121.5894513684704208, -24.34968618360934300, 0.1864209137778885528 ) ) ;
#80929 = VECTOR ( 'NONE', #38604, 1000.000000000000114 ) ;
#80930 = CARTESIAN_POINT ( 'NONE',  ( -48.62287095715009144, -24.34917612406837861, 0.1852690917426599304 ) ) ;
#80931 = CARTESIAN_POINT ( 'NONE',  ( -126.5228709571500332, -24.33927499327855770, 9.819080762295802955 ) ) ;
#80932 = ORIENTED_EDGE ( 'NONE', *, *, #3849, .F. ) ;
#80933 = EDGE_CURVE ( 'NONE', #30322, #82227, #59720, .T. ) ;
#80934 = CARTESIAN_POINT ( 'NONE',  ( -130.5728709571500872, -24.94533875906350318, 8.329945116542303296 ) ) ;
#80935 = CARTESIAN_POINT ( 'NONE',  ( -15.60622653811170402, 16.18669697583415967, -1.500000000000002220 ) ) ;
#80936 = EDGE_LOOP ( 'NONE', ( #14596, #85124, #9762, #47752 ) ) ;
#80937 = CARTESIAN_POINT ( 'NONE',  ( -96.62287095715005592, -29.50250243563736774, 8.947779886222138046 ) ) ;
#80938 = CARTESIAN_POINT ( 'NONE',  ( -101.5506312112252374, -24.35071581493543746, 9.817618358456027039 ) ) ;
#80939 = ADVANCED_FACE ( 'NONE', ( #93015 ), #54975, .F. ) ;
#80940 = CARTESIAN_POINT ( 'NONE',  ( 2.589743589743596086, -6.376774720514415407, 20.00140224358974095 ) ) ;
#80941 = CARTESIAN_POINT ( 'NONE',  ( 29.73860345376319358, -5.356774720496559894, 7.190646357373898680E-15 ) ) ;
#80942 = EDGE_CURVE ( 'NONE', #55923, #27877, #37742, .T. ) ;
#80943 = CARTESIAN_POINT ( 'NONE',  ( -30.57310351248101554, -25.30557784678703825, 3.856996771331004048 ) ) ;
#80944 = CARTESIAN_POINT ( 'NONE',  ( -3.586273028688536257, -19.27814873881845514, -1.500000000000002220 ) ) ;
#80945 = ADVANCED_FACE ( 'NONE', ( #54472 ), #85408, .F. ) ;
#80946 = CARTESIAN_POINT ( 'NONE',  ( -49.54372330632813259, -25.28866772429660870, 4.191984911758548371 ) ) ;
#80947 = ORIENTED_EDGE ( 'NONE', *, *, #46690, .F. ) ;
#80948 = CARTESIAN_POINT ( 'NONE',  ( 8.792760106793807040, 19.66521392739144858, 11.49999999999998934 ) ) ;
#80949 = DIRECTION ( 'NONE',  ( 1.000000000000000000, -0.000000000000000000, 0.000000000000000000 ) ) ;
#80950 = EDGE_CURVE ( 'NONE', #90167, #89315, #55154, .T. ) ;
#80951 = CARTESIAN_POINT ( 'NONE',  ( -80.76567584835706270, -25.30394766154488551, 4.998963552913667563 ) ) ;
#80952 = CARTESIAN_POINT ( 'NONE',  ( -63.58953762381672448, -24.66019654487198665, 8.947790411086129936 ) ) ;
#80953 = FACE_OUTER_BOUND ( 'NONE', #89145, .T. ) ;
#80954 = CARTESIAN_POINT ( 'NONE',  ( -14.90462150274475306, 17.49973755783957685, -1.500000000000002220 ) ) ;
#80955 = PERSON_AND_ORGANIZATION ( #70597, #27821 ) ;
#80956 = CARTESIAN_POINT ( 'NONE',  ( -102.6228709571500559, -23.47596703998600631, 11.44779298504227683 ) ) ;
#80957 = CARTESIAN_POINT ( 'NONE',  ( 1.175186991919851431, -0.3587747205144265483, 28.89597625626659649 ) ) ;
#80958 = CARTESIAN_POINT ( 'NONE',  ( -16.72505113720834657, 11.10480813184383742, 11.49999999999999645 ) ) ;
#80959 = CARTESIAN_POINT ( 'NONE',  ( -110.2646033073992129, -25.28814069144094034, 2.833559589122900846 ) ) ;
#80960 = FACE_OUTER_BOUND ( 'NONE', #87501, .T. ) ;
#80961 = DIRECTION ( 'NONE',  ( -3.773278334453079618E-23, 0.9999999999976377785, 2.173523156925979975E-06 ) ) ;
#80962 = CARTESIAN_POINT ( 'NONE',  ( -65.62287095715005592, -23.47593901973091235, -1.443836447539006196 ) ) ;
#80963 = EDGE_CURVE ( 'NONE', #76269, #99833, #13679, .T. ) ;
#80964 = CARTESIAN_POINT ( 'NONE',  ( -2.717543299849222826, 17.80004702990586196, 9.000000000000000000 ) ) ;
#80965 = CARTESIAN_POINT ( 'NONE',  ( 15.03354914759215966, -12.96403794047452607, 11.49999999999998934 ) ) ;
#80966 = DIRECTION ( 'NONE',  ( -3.773278334453079030E-23, 0.9999999999976377785, 2.173523156925979128E-06 ) ) ;
#80967 = CARTESIAN_POINT ( 'NONE',  ( 12.09797951242163805, 15.59582292391970704, -1.500000000000002220 ) ) ;
#80968 = CARTESIAN_POINT ( 'NONE',  ( -42.51346541940907287, -23.73766607897670156, -1.055555164236442689 ) ) ;
#80969 = COORDINATED_UNIVERSAL_TIME_OFFSET ( 0, 0, .AHEAD. ) ;
#80970 = CARTESIAN_POINT ( 'NONE',  ( -115.6228709571500559, -24.99132157543166954, 2.256160258750667502 ) ) ;
#80971 = CARTESIAN_POINT ( 'NONE',  ( -79.52287095715003318, -23.95044443724990657, 10.65354141964648704 ) ) ;
#80972 = CARTESIAN_POINT ( 'NONE',  ( -20.60669311552257810, 0.8253496925510150906, 11.49999999999999645 ) ) ;
#80973 = AXIS2_PLACEMENT_3D ( 'NONE', #43508, #74446, #4937 ) ;
#80974 = FACE_OUTER_BOUND ( 'NONE', #92820, .T. ) ;
#80975 = CARTESIAN_POINT ( 'NONE',  ( -18.78231125015805958, 12.62931641965373153, 11.49999999999999645 ) ) ;
#80976 = ORIENTED_EDGE ( 'NONE', *, *, #51042, .T. ) ;
#80977 = PLANE ( 'NONE',  #41080 ) ;
#80978 = CARTESIAN_POINT ( 'NONE',  ( -97.59370113735080565, -23.96119346886881374, -0.6495511937832058047 ) ) ;
#80979 = AXIS2_PLACEMENT_3D ( 'NONE', #34342, #7616, #95235 ) ;
#80980 = B_SPLINE_CURVE_WITH_KNOTS ( 'NONE', 3,
 ( #51056, #51556, #75367, #74868, #67283, #38304 ),
 .UNSPECIFIED., .F., .F.,
 ( 4, 2, 4 ),
 ( 0.000000000000000000, 0.001380764517854764749, 0.002761529035709529498 ),
 .UNSPECIFIED. ) ;
#80981 = EDGE_CURVE ( 'NONE', #89617, #20503, #677, .T. ) ;
#80982 = CARTESIAN_POINT ( 'NONE',  ( -110.2093792378191921, -25.29160350784524880, 5.585409231008217290 ) ) ;
#80983 = CARTESIAN_POINT ( 'NONE',  ( -45.55620429048339304, -25.00158670708908915, 2.256160236439166855 ) ) ;
#80984 = CIRCLE ( 'NONE', #90690, 1.530000000000002469 ) ;
#80985 = ORIENTED_EDGE ( 'NONE', *, *, #48552, .F. ) ;
#80986 = ADVANCED_FACE ( 'NONE', ( #56987 ), #79296, .F. ) ;
#80987 = ORIENTED_EDGE ( 'NONE', *, *, #65294, .T. ) ;
#80988 = FACE_OUTER_BOUND ( 'NONE', #18412, .T. ) ;
#80989 = CARTESIAN_POINT ( 'NONE',  ( -11.09240565882118368, -20.00103931635436538, -1.500000000000002220 ) ) ;
#80990 = CARTESIAN_POINT ( 'NONE',  ( -110.3346797185884327, -25.18492896333868813, 3.293943116708551777 ) ) ;
#80991 = AXIS2_PLACEMENT_3D ( 'NONE', #35593, #96980, #80764 ) ;
#80992 = DIRECTION ( 'NONE',  ( -3.773278334453079030E-23, 0.9999999999976377785, 2.173523156925978705E-06 ) ) ;
#80993 = CARTESIAN_POINT ( 'NONE',  ( -32.62287095715004881, -23.48783264082477729, -1.443836473390074371 ) ) ;
#80994 = CARTESIAN_POINT ( 'NONE',  ( -21.16606679798846358, 7.723709098063864076, 11.49999999999999645 ) ) ;
#80995 = EDGE_LOOP ( 'NONE', ( #32424, #95982, #74766, #92079 ) ) ;
#80996 = CARTESIAN_POINT ( 'NONE',  ( -43.48728809283164765, -24.51314013834316086, 0.6176544820404143987 ) ) ;
#80997 = CARTESIAN_POINT ( 'NONE',  ( -1.948345350117603125, -21.87844622001750139, 11.49999999999998934 ) ) ;
#80999 = CARTESIAN_POINT ( 'NONE',  ( -111.5135334585156102, -24.65952944569305316, 1.056160979905705677 ) ) ;
#80998 = AXIS2_PLACEMENT_3D ( 'NONE', #8290, #84908, #46355 ) ;
#81000 = CARTESIAN_POINT ( 'NONE',  ( -112.6228709571500559, -24.64965695001469115, 8.947790433994176951 ) ) ;
#81001 = VERTEX_POINT ( 'NONE', #94525 ) ;
#81002 = CARTESIAN_POINT ( 'NONE',  ( -35.62287095715005592, -29.50250786944525672, 11.44777988621624232 ) ) ;
#81003 = ADVANCED_FACE ( 'NONE', ( #49879 ), #2199, .F. ) ;
#81004 = DIRECTION ( 'NONE',  ( -3.773278334453079618E-23, 0.9999999999976377785, 2.173523156925979975E-06 ) ) ;
#81005 = ORIENTED_EDGE ( 'NONE', *, *, #23758, .T. ) ;
#81006 = LINE ( 'NONE', #51062, #61513 ) ;
#81007 = CARTESIAN_POINT ( 'NONE',  ( -14.05295919346176170, -14.94737400546395456, 11.49999999999998934 ) ) ;
#81008 = ORIENTED_EDGE ( 'NONE', *, *, #22778, .T. ) ;
#81009 = B_SPLINE_CURVE_WITH_KNOTS ( 'NONE', 3,
 ( #84722, #14706, #76099, #90340 ),
 .UNSPECIFIED., .F., .F.,
 ( 4, 4 ),
 ( 1.387778780781445676E-17, 0.0001000000000000028508 ),
 .UNSPECIFIED. ) ;
#81010 = ORIENTED_EDGE ( 'NONE', *, *, #81268, .T. ) ;
#81011 = ORIENTED_EDGE ( 'NONE', *, *, #78966, .T. ) ;
#81012 = CARTESIAN_POINT ( 'NONE',  ( -126.5228709571500332, -24.33832256527048088, 0.1851278514138670062 ) ) ;
#81013 = CARTESIAN_POINT ( 'NONE',  ( -5.338719972479099241, 22.46511350730333589, 11.49999999999998934 ) ) ;
#81014 = CARTESIAN_POINT ( 'NONE',  ( -104.5480580092806804, -24.66019654487200441, 8.947790411086108620 ) ) ;
#81015 = CARTESIAN_POINT ( 'NONE',  ( 15.61528876134825161, -13.05345633644532732, -1.500000000000002220 ) ) ;
#81016 = ADVANCED_FACE ( 'NONE', ( #25008 ), #32124, .F. ) ;
#81017 = ORIENTED_EDGE ( 'NONE', *, *, #8865, .T. ) ;
#81018 = CARTESIAN_POINT ( 'NONE',  ( -1.012926118674504883, -5.876774720514415407, 19.92818918856637822 ) ) ;
#81019 = CARTESIAN_POINT ( 'NONE',  ( -29.62069581956789222, -23.40858285148628681, 11.44779303447556984 ) ) ;
#81020 = CARTESIAN_POINT ( 'NONE',  ( -105.5132832374360277, -24.40034930558991633, 0.3402023900116059041 ) ) ;
#81021 = CARTESIAN_POINT ( 'NONE',  ( -35.55620429048339304, -23.47593901973091235, -1.443836447539011525 ) ) ;
#81022 = VERTEX_POINT ( 'NONE', #10294 ) ;
#81023 = B_SPLINE_CURVE_WITH_KNOTS ( 'NONE', 3,
 ( #66643, #20922, #1851, #25678, #64778, #56147 ),
 .UNSPECIFIED., .F., .F.,
 ( 4, 2, 4 ),
 ( 1.570887131794638196E-05, 0.001396322306279762157, 0.002776935741241578007 ),
 .UNSPECIFIED. ) ;
#81024 = CARTESIAN_POINT ( 'NONE',  ( -29.24577077129365321, -24.76881379442145814, 4.691559412919051653 ) ) ;
#81025 = PLANE ( 'NONE',  #97758 ) ;
#81026 = ORIENTED_EDGE ( 'NONE', *, *, #34721, .F. ) ;
#81027 = B_SPLINE_CURVE_WITH_KNOTS ( 'NONE', 3,
 ( #34984, #13624, #28868, #65962, #59830, #90764 ),
 .UNSPECIFIED., .F., .F.,
 ( 4, 2, 4 ),
 ( 0.000000000000000000, 0.001380764517853249034, 0.002761529035706497635 ),
 .UNSPECIFIED. ) ;
#81028 = CARTESIAN_POINT ( 'NONE',  ( -7.357705842588929457, 19.43699106120834230, 11.49999999999998934 ) ) ;
#81029 = ORIENTED_EDGE ( 'NONE', *, *, #2639, .F. ) ;
#81030 = CC_DESIGN_PERSON_AND_ORGANIZATION_ASSIGNMENT ( #55004, #61121, ( #29472 ) ) ;
#81032 = VERTEX_POINT ( 'NONE', #70692 ) ;
#81031 = CARTESIAN_POINT ( 'NONE',  ( -101.5603755832771071, -23.48783264082477373, -1.443836473390089248 ) ) ;
#81033 = CARTESIAN_POINT ( 'NONE',  ( -24.90875734969025501, 5.356774720514425603, 26.43402280011862615 ) ) ;
#81034 = CARTESIAN_POINT ( 'NONE',  ( -51.16340783650578317, -25.30574378417172454, 5.002672300970606223 ) ) ;
#81035 = ORIENTED_EDGE ( 'NONE', *, *, #62731, .F. ) ;
#81036 = ORIENTED_EDGE ( 'NONE', *, *, #19293, .T. ) ;
#81037 = CARTESIAN_POINT ( 'NONE',  ( -88.55620429048339304, -24.65952944569304606, 1.056160979905699904 ) ) ;
#81038 = DIRECTION ( 'NONE',  ( -3.773278334453079618E-23, 0.9999999999976377785, 2.173523156925979975E-06 ) ) ;
#81039 = CARTESIAN_POINT ( 'NONE',  ( -74.62287095715002749, -24.33832256527048088, 0.1851278514138608444 ) ) ;
#81041 = ORIENTED_EDGE ( 'NONE', *, *, #14930, .T. ) ;
#81040 = CARTESIAN_POINT ( 'NONE',  ( -13.14421341422731260, -17.72855101262432242, 11.49999999999999645 ) ) ;
#81042 = CARTESIAN_POINT ( 'NONE',  ( -20.27875734969026311, -6.376774720514428729, 27.00402280011862288 ) ) ;
#81043 = CARTESIAN_POINT ( 'NONE',  ( -11.86362535333686807, -19.25999739251378173, 11.49999999999998934 ) ) ;
#81045 = VERTEX_POINT ( 'NONE', #10798 ) ;
#81044 = CARTESIAN_POINT ( 'NONE',  ( -115.5505208059758360, -24.92592662359561473, 8.075495903017996469 ) ) ;
#81046 = ORIENTED_EDGE ( 'NONE', *, *, #10733, .T. ) ;
#81047 = PLANE ( 'NONE',  #98473 ) ;
#81048 = VECTOR ( 'NONE', #15847, 1000.000000000000114 ) ;
#81049 = CARTESIAN_POINT ( 'NONE',  ( -128.5562042904833788, -23.48783264082479150, -1.443836473390056829 ) ) ;
#81050 = EDGE_LOOP ( 'NONE', ( #80834, #10482, #75674, #6624 ) ) ;
#81051 = CARTESIAN_POINT ( 'NONE',  ( -18.51692787870624102, -10.26217664800131502, 11.49999999999998934 ) ) ;
#81052 = VECTOR ( 'NONE', #1764, 1000.000000000000000 ) ;
#81053 = CARTESIAN_POINT ( 'NONE',  ( -7.131053040288445999, -6.376774720514413630, 19.60308799987318196 ) ) ;
#81054 = FACE_OUTER_BOUND ( 'NONE', #51565, .T. ) ;
#81055 = CARTESIAN_POINT ( 'NONE',  ( 21.78807519107708401, 4.755904613692067073, -1.500000000000002220 ) ) ;
#81056 = LINE ( 'NONE', #11538, #34059 ) ;
#81057 = ADVANCED_FACE ( 'NONE', ( #94024 ), #79798, .F. ) ;
#81058 = ORIENTED_EDGE ( 'NONE', *, *, #96169, .T. ) ;
#81059 = CIRCLE ( 'NONE', #21064, 84.48086791635432746 ) ;
#81060 = DIRECTION ( 'NONE',  ( 0.000000000000000000, 1.000000000000000000, 0.000000000000000000 ) ) ;
#81061 = CARTESIAN_POINT ( 'NONE',  ( -91.52287095715006160, -29.50250243563736774, 8.947779886222139822 ) ) ;
#81062 = B_SPLINE_CURVE_WITH_KNOTS ( 'NONE', 3,
 ( #1737, #88474, #56034, #18948 ),
 .UNSPECIFIED., .F., .F.,
 ( 4, 4 ),
 ( 0.5891933397657490579, 0.5901940868065144175 ),
 .UNSPECIFIED. ) ;
#81063 = CARTESIAN_POINT ( 'NONE',  ( -36.49041699993523480, -24.35071581493542325, 9.817618358456030592 ) ) ;
#81064 = DIRECTION ( 'NONE',  ( -2.615445361545220718E-15, -0.000000000000000000, -1.000000000000000000 ) ) ;
#81065 = AXIS2_PLACEMENT_3D ( 'NONE', #92740, #78008, #907 ) ;
#81066 = CARTESIAN_POINT ( 'NONE',  ( 2.628080361126900133, -19.32819128710564272, 11.49999999999998934 ) ) ;
#81067 = EDGE_CURVE ( 'NONE', #99233, #99855, #41762, .T. ) ;
#81068 = VECTOR ( 'NONE', #6360, 1000.000000000000114 ) ;
#81069 = CARTESIAN_POINT ( 'NONE',  ( -2.751442626040462081, 21.25944542233241563, 11.49999999999998934 ) ) ;
#81070 = FACE_OUTER_BOUND ( 'NONE', #89972, .T. ) ;
#81071 = EDGE_CURVE ( 'NONE', #69030, #29733, #17406, .T. ) ;
#81072 = CARTESIAN_POINT ( 'NONE',  ( -2.499999999999993339, 19.99999999999999645, 0.000000000000000000 ) ) ;
#81073 = PLANE ( 'NONE',  #6891 ) ;
#81074 = CARTESIAN_POINT ( 'NONE',  ( -22.16177213047534877, -5.259615592301647879, -1.500000000000002220 ) ) ;
#81075 = AXIS2_PLACEMENT_3D ( 'NONE', #82678, #11179, #97894 ) ;
#81076 = CARTESIAN_POINT ( 'NONE',  ( -98.51142843485534684, -24.34968618360934300, 0.1864209137778828629 ) ) ;
#81077 = CARTESIAN_POINT ( 'NONE',  ( -24.90875734969025501, -6.475225279485573360, 26.43402280011862615 ) ) ;
#81078 = CARTESIAN_POINT ( 'NONE',  ( -7.573260116017839216, 18.43532004384545786, 11.49999999999999645 ) ) ;
#81079 = CARTESIAN_POINT ( 'NONE',  ( -20.27875734969026311, 6.143225279485574397, 24.00402280011862288 ) ) ;
#81080 = CARTESIAN_POINT ( 'NONE',  ( -39.48048556723951208, -24.66019654487198665, 8.947790411086131712 ) ) ;
#81081 = CARTESIAN_POINT ( 'NONE',  ( -81.62287095715005592, -29.50248528299804818, 1.056150453629038477 ) ) ;
#81082 = VERTEX_POINT ( 'NONE', #87924 ) ;
#81083 = EDGE_CURVE ( 'NONE', #534, #18471, #21082, .T. ) ;
#81084 = PLANE ( 'NONE',  #88234 ) ;
#81085 = CARTESIAN_POINT ( 'NONE',  ( -32.99702443869961854, -25.31600595412499644, 6.101236642668423471 ) ) ;
#81086 = CARTESIAN_POINT ( 'NONE',  ( 16.98214085172422827, 13.50221961261776293, 11.49999999999998934 ) ) ;
#81087 = CARTESIAN_POINT ( 'NONE',  ( -56.59864015429606354, -23.96169478059713498, 10.65365249895718236 ) ) ;
#81088 = CARTESIAN_POINT ( 'NONE',  ( 15.80261042061247068, 11.49252619723154112, -1.500000000000002220 ) ) ;
#81089 = CARTESIAN_POINT ( 'NONE',  ( -0.02075734969026423599, -6.376774720514426953, -0.08597719988137648983 ) ) ;
#81090 = ITEM_DEFINED_TRANSFORMATION ( 'NONE', 'NONE', #11529,  #37391 ) ;
#81091 = FACE_OUTER_BOUND ( 'NONE', #65659, .T. ) ;
#81092 = CARTESIAN_POINT ( 'NONE',  ( 13.31029742451639386, -15.53102932315203510, 11.49999999999999645 ) ) ;
#81093 = CARTESIAN_POINT ( 'NONE',  ( 10.24966870126729646, -6.475225279485571583, -27.02528057709740850 ) ) ;
#81094 = CARTESIAN_POINT ( 'NONE',  ( -118.6228709571500559, -23.73907113216991860, -1.053371485793222151 ) ) ;
#81095 = ORIENTED_EDGE ( 'NONE', *, *, #36786, .T. ) ;
#81096 = CARTESIAN_POINT ( 'NONE',  ( -23.31187512739357715, 0.3587747205144061202, -17.31005501743528541 ) ) ;
#81097 = CARTESIAN_POINT ( 'NONE',  ( -39.51912653461286595, -25.28892541655923054, 3.844034288105113273 ) ) ;
#81098 = DIRECTION ( 'NONE',  ( 0.000000000000000000, -2.173523156925979552E-06, 0.9999999999976378895 ) ) ;
#81099 = CARTESIAN_POINT ( 'NONE',  ( -49.27881313098881577, -25.25138871933836171, 6.114505553594992371 ) ) ;
#81100 = CARTESIAN_POINT ( 'NONE',  ( -31.24388727629347784, -24.87479601683088148, 8.247789944647559324 ) ) ;
#81101 = ORIENTED_EDGE ( 'NONE', *, *, #87842, .T. ) ;
#81102 = CARTESIAN_POINT ( 'NONE',  ( -111.3776484685884469, -25.29712067403330877, 4.332404411321261861 ) ) ;
#81103 = ADVANCED_FACE ( 'NONE', ( #3204 ), #72206, .T. ) ;
#81104 = CARTESIAN_POINT ( 'NONE',  ( 8.869223403490039459, -21.23658630136709391, 11.49999999999999645 ) ) ;
#81105 = CARTESIAN_POINT ( 'NONE',  ( 22.50852769316577096, -3.342225187595919689, 11.49999999999998934 ) ) ;
#81106 = CARTESIAN_POINT ( 'NONE',  ( -70.95923861438973290, -25.07168450528815740, 7.426717504460598640 ) ) ;
#81107 = CARTESIAN_POINT ( 'NONE',  ( -94.22287095715012128, -23.47593901973090880, -1.443836447538997314 ) ) ;
#81108 = CARTESIAN_POINT ( 'NONE',  ( -90.54767163586556933, -24.52300882791529801, 0.6510814631126391472 ) ) ;
#81109 = CARTESIAN_POINT ( 'NONE',  ( -0.7395115731254272573, 18.09566585216508727, 8.999999999999998224 ) ) ;
#81110 = FACE_OUTER_BOUND ( 'NONE', #21696, .T. ) ;
#81111 = AXIS2_PLACEMENT_3D ( 'NONE', #14999, #93117, #39838 ) ;
#81112 = CARTESIAN_POINT ( 'NONE',  ( -1.678574117887026373, -21.80011532881206548, 11.49999999999998934 ) ) ;
#81113 = EDGE_CURVE ( 'NONE', #55041, #44878, #95030, .T. ) ;
#81114 = CARTESIAN_POINT ( 'NONE',  ( -70.55620429048337883, -24.99132157543166954, 2.256160258750667946 ) ) ;
#81115 = LINE ( 'NONE', #13588, #23342 ) ;
#81116 = CARTESIAN_POINT ( 'NONE',  ( -27.96875734969026084, -3.316774720514426456, 26.43402280011862615 ) ) ;
#81117 = CARTESIAN_POINT ( 'NONE',  ( 9.383883476483161346, 17.86611652351680846, 2.100000000000000089 ) ) ;
#81118 = ORIENTED_EDGE ( 'NONE', *, *, #78908, .F. ) ;
#81119 = CARTESIAN_POINT ( 'NONE',  ( 0.5039804632396667206, -20.40334623801319580, -1.500000000000002220 ) ) ;
#81120 = ORIENTED_EDGE ( 'NONE', *, *, #94113, .T. ) ;
#81121 = ORIENTED_EDGE ( 'NONE', *, *, #71265, .T. ) ;
#81122 = VERTEX_POINT ( 'NONE', #49376 ) ;
#81123 = ORIENTED_EDGE ( 'NONE', *, *, #978, .F. ) ;
#81124 = CARTESIAN_POINT ( 'NONE',  ( -20.90396053131702914, -9.656267258341529214, 11.49999999999998934 ) ) ;
#81125 = DIRECTION ( 'NONE',  ( 0.000000000000000000, -1.000000000000000000, 0.000000000000000000 ) ) ;
#81126 = CARTESIAN_POINT ( 'NONE',  ( 15.73562052650688514, -12.66937975264744587, -1.500000000000002220 ) ) ;
#81127 = EDGE_LOOP ( 'NONE', ( #28834, #70381, #99612, #87538 ) ) ;
#81128 = FACE_OUTER_BOUND ( 'NONE', #84902, .T. ) ;
#81129 = CARTESIAN_POINT ( 'NONE',  ( -48.52287095715005449, -24.35013146730203815, 9.818937971375097717 ) ) ;
#81130 = B_SPLINE_CURVE_WITH_KNOTS ( 'NONE', 3,
 ( #10556, #26285, #72469, #19657 ),
 .UNSPECIFIED., .F., .F.,
 ( 4, 4 ),
 ( 0.2699787096657541574, 0.2789851409378695801 ),
 .UNSPECIFIED. ) ;
#81132 = CARTESIAN_POINT ( 'NONE',  ( -95.58289945215418015, -25.00158670708911046, 2.256160236439221034 ) ) ;
#81131 = AXIS2_PLACEMENT_3D ( 'NONE', #61980, #70082, #15281 ) ;
#81133 = CARTESIAN_POINT ( 'NONE',  ( -123.5562042904833788, -23.47593901973091235, -1.443836447538997536 ) ) ;
#81135 = VERTEX_POINT ( 'NONE', #48366 ) ;
#81134 = CARTESIAN_POINT ( 'NONE',  ( 21.34331307443176584, 0.5271963136488534429, 11.49999999999999645 ) ) ;
#81136 = CARTESIAN_POINT ( 'NONE',  ( 7.153659783701941777, -5.876774720514421624, 20.92502190304499265 ) ) ;
#81137 = VECTOR ( 'NONE', #33327, 1000.000000000000000 ) ;
#81138 = ORIENTED_EDGE ( 'NONE', *, *, #65147, .F. ) ;
#81139 = CARTESIAN_POINT ( 'NONE',  ( 21.27325221474336914, 6.521069146585026566, 11.49999999999998934 ) ) ;
#81140 = CARTESIAN_POINT ( 'NONE',  ( -18.79711486612840332, 8.613068827758688428, -1.500000000000002220 ) ) ;
#81141 = EDGE_CURVE ( 'NONE', #35597, #32574, #34068, .T. ) ;
#81142 = ADVANCED_FACE ( 'NONE', ( #26016 ), #80307, .F. ) ;
#81143 = AXIS2_PLACEMENT_3D ( 'NONE', #56425, #24942, #16835 ) ;
#81144 = EDGE_LOOP ( 'NONE', ( #1911, #73617, #91244, #29147, #74388, #75759, #56156, #11623, #22343 ) ) ;
#81145 = CARTESIAN_POINT ( 'NONE',  ( -68.92380496721939664, -25.20650855361216713, 6.812664954086296909 ) ) ;
#81146 = ORIENTED_EDGE ( 'NONE', *, *, #16612, .T. ) ;
#81147 = CARTESIAN_POINT ( 'NONE',  ( 0.000000000000000000, -16.94322527948557422, 0.000000000000000000 ) ) ;
#81148 = VERTEX_POINT ( 'NONE', #71199 ) ;
#81149 = CARTESIAN_POINT ( 'NONE',  ( 13.59451591917074431, -3.316774720514426456, -28.23515841827053308 ) ) ;
#81150 = CARTESIAN_POINT ( 'NONE',  ( 5.581485548573628996, 20.18083795961418403, -1.500000000000002220 ) ) ;
#81151 = CARTESIAN_POINT ( 'NONE',  ( -21.09739860443290382, 5.981408608369527258, 11.49999999999999645 ) ) ;
#81152 = LINE ( 'NONE', #72549, #99811 ) ;
#81153 = CARTESIAN_POINT ( 'NONE',  ( -18.84819291449097278, 12.34854029719970825, 11.49999999999998934 ) ) ;
#81154 = EDGE_CURVE ( 'NONE', #82392, #64064, #25736, .T. ) ;
#81155 = CARTESIAN_POINT ( 'NONE',  ( 13.87900837158347755, -15.70065903812341013, 11.49999999999998934 ) ) ;
#81156 = CARTESIAN_POINT ( 'NONE',  ( -26.09849696787948403, -24.88148762671936964, 5.165052607479680979 ) ) ;
#81157 = CARTESIAN_POINT ( 'NONE',  ( 6.127395130496778641, -5.876774720514417183, 20.13872869980892943 ) ) ;
#81158 = CARTESIAN_POINT ( 'NONE',  ( -119.5178257542950035, -24.51419770103158768, 9.386484678747164523 ) ) ;
#81159 = CARTESIAN_POINT ( 'NONE',  ( -68.52287095715007581, -23.47593901973090524, -1.443836447538997092 ) ) ;
#81160 = ORIENTED_EDGE ( 'NONE', *, *, #28265, .F. ) ;
#81161 = ORIENTED_EDGE ( 'NONE', *, *, #7550, .F. ) ;
#81162 = ORIENTED_EDGE ( 'NONE', *, *, #29886, .F. ) ;
#81163 = CARTESIAN_POINT ( 'NONE',  ( -52.62810917408141620, -24.51314013834315375, 0.6176544820404124003 ) ) ;
#81164 = ORIENTED_EDGE ( 'NONE', *, *, #34640, .F. ) ;
#81165 = CARTESIAN_POINT ( 'NONE',  ( 19.88731969966643476, 8.162773808193900749, -1.500000000000002220 ) ) ;
#81166 = CARTESIAN_POINT ( 'NONE',  ( -26.16566273216211513, -24.93396852503405370, 5.877190228123938986 ) ) ;
#81167 = CARTESIAN_POINT ( 'NONE',  ( 20.91448408463407205, 2.778442817847782020, 11.49999999999998934 ) ) ;
#81168 = CARTESIAN_POINT ( 'NONE',  ( -99.66789520314513595, -25.23538937966463891, 3.604794963105668160 ) ) ;
#81169 = LINE ( 'NONE', #3062, #49753 ) ;
#81170 = CARTESIAN_POINT ( 'NONE',  ( -96.62287095715005592, -23.47596703998600631, 11.44779298504227860 ) ) ;
#81171 = CARTESIAN_POINT ( 'NONE',  ( -81.52287095715001897, -24.66019654487199375, 8.947790411086126383 ) ) ;
#81173 = B_SPLINE_CURVE_WITH_KNOTS ( 'NONE', 3,
 ( #5646, #98483, #93761, #13252, #59446, #83270, #44717, #37097, #59955, #5154, #90884, #16633, #51836, #28983, #52332, #39483 ),
 .UNSPECIFIED., .F., .F.,
 ( 4, 2, 2, 2, 2, 2, 2, 4 ),
 ( 8.673617379884035472E-19, 0.0004698675029436834511, 0.0007048012544155247971, 0.0009397350058873660348, 0.001174668757359207272, 0.001409602508831048727, 0.001644536260302889965, 0.001879470011774731202 ),
 .UNSPECIFIED. ) ;
#81172 = CARTESIAN_POINT ( 'NONE',  ( -129.6238143503192077, -23.73791477778912906, 11.05961554403170233 ) ) ;
#81174 = CARTESIAN_POINT ( 'NONE',  ( 16.78392297789021015, 14.29496084597832883, -1.500000000000002220 ) ) ;
#81175 = ORIENTED_EDGE ( 'NONE', *, *, #88894, .F. ) ;
#81176 = B_SPLINE_CURVE_WITH_KNOTS ( 'NONE', 3,
 ( #9006, #70920, #1410, #32344, #63320, #94238 ),
 .UNSPECIFIED., .F., .F.,
 ( 4, 2, 4 ),
 ( 0.000000000000000000, 0.001380764517853252287, 0.002761529035706504574 ),
 .UNSPECIFIED. ) ;
#81177 = CARTESIAN_POINT ( 'NONE',  ( -65.52204159167497721, -23.48786465467241058, 11.44779295918254824 ) ) ;
#81178 = EDGE_CURVE ( 'NONE', #79014, #98210, #65610, .T. ) ;
#81179 = LINE ( 'NONE', #42635, #57909 ) ;
#81180 = CARTESIAN_POINT ( 'NONE',  ( -41.64605464260454681, -25.31624614353306058, 4.957686406151942116 ) ) ;
#81181 = CARTESIAN_POINT ( 'NONE',  ( -47.52287095715007581, -23.47593901973090169, -1.443836447538997092 ) ) ;
#81182 = CARTESIAN_POINT ( 'NONE',  ( -32.52287095715006160, -24.64898659630528854, 1.056161002820817485 ) ) ;
#81183 = CARTESIAN_POINT ( 'NONE',  ( -6.767052838139933080, -20.26514109264706676, 11.49999999999998934 ) ) ;
#81184 = CARTESIAN_POINT ( 'NONE',  ( -97.62287095715005592, -23.48786465467241058, 11.44779295918254114 ) ) ;
#81185 = CARTESIAN_POINT ( 'NONE',  ( -48.85382640980453317, -25.31392319263090585, 5.203681702801227438 ) ) ;
#81186 = VECTOR ( 'NONE', #70707, 1000.000000000000000 ) ;
#81187 = EDGE_CURVE ( 'NONE', #89111, #39193, #83957, .T. ) ;
#81188 = DIRECTION ( 'NONE',  ( 0.000000000000000000, 0.000000000000000000, -1.000000000000000000 ) ) ;
#81189 = CARTESIAN_POINT ( 'NONE',  ( -80.54762525791510086, -25.12326838703506127, 7.100031122939245876 ) ) ;
#81190 = CARTESIAN_POINT ( 'NONE',  ( 21.78986343443989071, 5.811249688775594002, -1.500000000000002220 ) ) ;
#81191 = ADVANCED_FACE ( 'NONE', ( #12279 ), #43256, .T. ) ;
#81192 = CARTESIAN_POINT ( 'NONE',  ( -49.27764846858840997, -29.50249634415583699, 6.145195751613371726 ) ) ;
#81193 = ORIENTED_EDGE ( 'NONE', *, *, #89586, .F. ) ;
#81194 = CARTESIAN_POINT ( 'NONE',  ( 4.628547153713393314, -5.876774720514418959, 20.50654586986123817 ) ) ;
#81195 = CARTESIAN_POINT ( 'NONE',  ( -79.60030546162484200, -23.73766607897669800, -1.055555164236459564 ) ) ;
#81196 = CARTESIAN_POINT ( 'NONE',  ( 17.76913753361954562, 8.601950719843506121, 11.49999999999999645 ) ) ;
#81197 = DIRECTION ( 'NONE',  ( 0.000000000000000000, -0.000000000000000000, -1.000000000000000000 ) ) ;
#81198 = CARTESIAN_POINT ( 'NONE',  ( -67.58021307568701275, -24.65952944569304961, 1.056160979905700570 ) ) ;
#81199 = ORIENTED_EDGE ( 'NONE', *, *, #92120, .T. ) ;
#81200 = ADVANCED_FACE ( 'NONE', ( #58978 ), #11295, .T. ) ;
#81201 = DIRECTION ( 'NONE',  ( -3.773278334453080206E-23, 0.9999999999976377785, 2.173523156925979975E-06 ) ) ;
#81202 = FACE_OUTER_BOUND ( 'NONE', #98753, .T. ) ;
#81203 = CARTESIAN_POINT ( 'NONE',  ( -101.1692196971220312, -25.12268517087270325, 6.877671137330668039 ) ) ;
#81204 = CARTESIAN_POINT ( 'NONE',  ( -19.28869470675124731, 9.786980993800005635, -1.500000000000002220 ) ) ;
#81205 = CARTESIAN_POINT ( 'NONE',  ( 5.101312121039179637, 3.305285905532577839, -27.56070534847060571 ) ) ;
#81206 = CARTESIAN_POINT ( 'NONE',  ( -19.23900614489824079, 2.250179475969715348, -1.500000000000002220 ) ) ;
#81207 = ADVANCED_FACE ( 'NONE', ( #43748 ), #40265, .T. ) ;
#81208 = CARTESIAN_POINT ( 'NONE',  ( -10.23894677657808749, -4.339657088724310441, 29.22408179085893210 ) ) ;
#81209 = CARTESIAN_POINT ( 'NONE',  ( -85.62287095715002749, -25.00182538069145011, 7.747789668545099317 ) ) ;
#81210 = CARTESIAN_POINT ( 'NONE',  ( -12.15653940608521566, -15.58205587995076868, 11.49999999999998934 ) ) ;
#81211 = CIRCLE ( 'NONE', #50422, 28.96799999999999642 ) ;
#81212 = B_SPLINE_CURVE_WITH_KNOTS ( 'NONE', 3,
 ( #2079, #33513, #19275, #17284 ),
 .UNSPECIFIED., .F., .F.,
 ( 4, 4 ),
 ( 0.000000000000000000, 9.999999999998897304E-05 ),
 .UNSPECIFIED. ) ;
#81213 = ORIENTED_EDGE ( 'NONE', *, *, #72999, .F. ) ;
#81214 = CARTESIAN_POINT ( 'NONE',  ( -2.356373108420451334, 20.14613781377289214, 11.49999999999999645 ) ) ;
#81215 = CARTESIAN_POINT ( 'NONE',  ( 11.29837800214456855, 4.960377205085137575, -27.59811486027058436 ) ) ;
#81216 = B_SPLINE_CURVE_WITH_KNOTS ( 'NONE', 3,
 ( #64198, #29094, #21966, #82386 ),
 .UNSPECIFIED., .F., .F.,
 ( 4, 4 ),
 ( 0.000000000000000000, 0.0001000000000000028644 ),
 .UNSPECIFIED. ) ;
#81217 = B_SPLINE_CURVE_WITH_KNOTS ( 'NONE', 3,
 ( #19904, #20900, #27539, #4699, #67111, #65622, #82311, #58496, #67602, #96539 ),
 .UNSPECIFIED., .F., .F.,
 ( 4, 2, 2, 2, 4 ),
 ( 1.844036349440735311E-17, 0.0001572768558401152516, 0.0003145537116802120717, 0.0004718305675203088648, 0.0006291074233604057120 ),
 .UNSPECIFIED. ) ;
#81218 = VERTEX_POINT ( 'NONE', #74197 ) ;
#81219 = CARTESIAN_POINT ( 'NONE',  ( -99.54045094251550552, -25.27399224497114005, 4.126029246454620214 ) ) ;
#81220 = LINE ( 'NONE', #28417, #50961 ) ;
#81221 = DIRECTION ( 'NONE',  ( -0.000000000000000000, -1.000000000000000000, 0.000000000000000000 ) ) ;
#81222 = DIRECTION ( 'NONE',  ( 1.000000000000000000, 0.000000000000000000, 0.000000000000000000 ) ) ;
#81223 = LINE ( 'NONE', #99429, #62507 ) ;
#81224 = CARTESIAN_POINT ( 'NONE',  ( 12.62869658624171976, -15.57725692549414376, -1.500000000000002220 ) ) ;
#81225 = CARTESIAN_POINT ( 'NONE',  ( -51.55620429048339304, -23.47596703998600276, 11.44779298504227505 ) ) ;
#81226 = ORIENTED_EDGE ( 'NONE', *, *, #92274, .T. ) ;
#81227 = EDGE_CURVE ( 'NONE', #76458, #31435, #90773, .T. ) ;
#81228 = CARTESIAN_POINT ( 'NONE',  ( -90.55620429048339304, -23.47596703998600631, 11.44779298504227683 ) ) ;
#81229 = DIRECTION ( 'NONE',  ( 0.000000000000000000, 0.000000000000000000, 1.000000000000000000 ) ) ;
#81230 = LINE ( 'NONE', #11707, #71130 ) ;
#81231 = DIRECTION ( 'NONE',  ( -3.773278334453079030E-23, 0.9999999999976377785, 2.173523156925979128E-06 ) ) ;
#81232 = CARTESIAN_POINT ( 'NONE',  ( -73.54978490721288154, -24.15543982623907127, -0.2315651400026654816 ) ) ;
#81233 = CARTESIAN_POINT ( 'NONE',  ( 15.12110981444426372, 4.119741627009140927, -28.36351442485845453 ) ) ;
#81234 = EDGE_CURVE ( 'NONE', #69616, #53302, #98805, .T. ) ;
#81235 = DIRECTION ( 'NONE',  ( -0.6392559695863496705, -6.845827386180411947E-16, -0.7689940216596069522 ) ) ;
#81236 = ORIENTED_EDGE ( 'NONE', *, *, #36844, .T. ) ;
#81237 = CARTESIAN_POINT ( 'NONE',  ( 18.91379238805564356, 7.493326543281090935, -1.500000000000002220 ) ) ;
#81238 = ORIENTED_EDGE ( 'NONE', *, *, #59749, .T. ) ;
#81239 = CARTESIAN_POINT ( 'NONE',  ( -14.16064136294604303, -18.02537036913223290, -1.500000000000002220 ) ) ;
#81240 = CARTESIAN_POINT ( 'NONE',  ( 31.68084058116266988, 4.801908866063379300, 29.09855526763849198 ) ) ;
#81241 = EDGE_LOOP ( 'NONE', ( #70549, #50870, #82536, #65338 ) ) ;
#81242 = CARTESIAN_POINT ( 'NONE',  ( -49.10646091633891075, -25.26830347608276028, 4.049788970800419996 ) ) ;
#81243 = CARTESIAN_POINT ( 'NONE',  ( -76.52287095715006160, -24.33832256527049154, 0.1851278514138614828 ) ) ;
#81244 = CARTESIAN_POINT ( 'NONE',  ( -74.58953762381673869, -23.47593901973091235, -1.443836447539006196 ) ) ;
#81245 = CARTESIAN_POINT ( 'NONE',  ( 9.480266252741309074, -18.97159823121752709, 11.49999999999999645 ) ) ;
#81246 = CARTESIAN_POINT ( 'NONE',  ( -21.14524153552446606, 6.695245452574716261, -1.500000000000002220 ) ) ;
#81247 = CIRCLE ( 'NONE', #14813, 4.300000000000000711 ) ;
#81248 = CARTESIAN_POINT ( 'NONE',  ( 4.697267095454844998, -20.06606415395816967, 11.49999999999998934 ) ) ;
#81249 = EDGE_CURVE ( 'NONE', #30827, #53562, #81453, .T. ) ;
#81250 = ORIENTED_EDGE ( 'NONE', *, *, #34073, .T. ) ;
#81251 = CARTESIAN_POINT ( 'NONE',  ( -41.64113970441989920, -24.15543982623907127, -0.2315651400026566831 ) ) ;
#81252 = ORIENTED_EDGE ( 'NONE', *, *, #63537, .T. ) ;
#81253 = FACE_OUTER_BOUND ( 'NONE', #80327, .T. ) ;
#81254 = CARTESIAN_POINT ( 'NONE',  ( -77.52287095715010423, -23.47593901973090524, -1.443836447538997092 ) ) ;
#81255 = VERTEX_POINT ( 'NONE', #61971 ) ;
#81256 = ORIENTED_EDGE ( 'NONE', *, *, #61494, .F. ) ;
#81257 = VERTEX_POINT ( 'NONE', #22871 ) ;
#81258 = FACE_OUTER_BOUND ( 'NONE', #27937, .T. ) ;
#81259 = CARTESIAN_POINT ( 'NONE',  ( -28.59442033382131854, -23.99963963181664539, 10.23563545308467049 ) ) ;
#81260 = DIRECTION ( 'NONE',  ( 0.000000000000000000, 0.000000000000000000, 1.000000000000000000 ) ) ;
#81261 = CARTESIAN_POINT ( 'NONE',  ( 13.57807927624399902, 15.74560944506941951, -1.500000000000002220 ) ) ;
#81262 = CARTESIAN_POINT ( 'NONE',  ( 12.82194709444435077, -17.51738216156474337, 11.49999999999999645 ) ) ;
#81263 = ORIENTED_EDGE ( 'NONE', *, *, #76568, .T. ) ;
#81264 = EDGE_CURVE ( 'NONE', #73710, #59693, #52851, .T. ) ;
#81265 = PLANE ( 'NONE',  #19139 ) ;
#81266 = CARTESIAN_POINT ( 'NONE',  ( -122.5228709571500616, -24.64898659630368272, 1.056161002820833028 ) ) ;
#81267 = CARTESIAN_POINT ( 'NONE',  ( 17.77913403553526805, 13.70458096452923691, -1.500000000000002220 ) ) ;
#81268 = EDGE_CURVE ( 'NONE', #60537, #90130, #22374, .T. ) ;
#81269 = ADVANCED_FACE ( 'NONE', ( #62468 ), #68627, .T. ) ;
#81270 = LINE ( 'NONE', #4655, #12446 ) ;
#81271 = CARTESIAN_POINT ( 'NONE',  ( -28.98875734969026396, -5.965225279485572685, -0.08597719988137648983 ) ) ;
#81272 = ORIENTED_EDGE ( 'NONE', *, *, #45308, .T. ) ;
#81273 = CARTESIAN_POINT ( 'NONE',  ( -98.52287095715007581, -24.33927499327855415, 9.819080762295810061 ) ) ;
#81274 = VECTOR ( 'NONE', #85708, 1000.000000000000000 ) ;
#81275 = CARTESIAN_POINT ( 'NONE',  ( -129.5228709571500758, -24.64898659630529920, 1.056161002820834804 ) ) ;
#81277 = EDGE_CURVE ( 'NONE', #84725, #73156, #14771, .T. ) ;
#81276 = APPROVAL_PERSON_ORGANIZATION ( #61744, #47005, #23141 ) ;
#81278 = ORIENTED_EDGE ( 'NONE', *, *, #69819, .T. ) ;
#81279 = ORIENTED_EDGE ( 'NONE', *, *, #72243, .F. ) ;
#81280 = FACE_OUTER_BOUND ( 'NONE', #14452, .T. ) ;
#81281 = VERTEX_POINT ( 'NONE', #44746 ) ;
#81282 = CARTESIAN_POINT ( 'NONE',  ( 13.65650298889772962, 16.33668418983593185, -1.500000000000002220 ) ) ;
#81283 = VERTEX_POINT ( 'NONE', #30502 ) ;
#81284 = CARTESIAN_POINT ( 'NONE',  ( -100.7110842131079522, -25.12685321106879144, 7.079481877294677261 ) ) ;
#81285 = CARTESIAN_POINT ( 'NONE',  ( 21.83365961380331655, 0.8745889840297637052, -1.500000000000002220 ) ) ;
#81286 = CARTESIAN_POINT ( 'NONE',  ( -45.62287095715004881, -23.48783264082478084, -1.443836473390070374 ) ) ;
#81287 = CARTESIAN_POINT ( 'NONE',  ( 2.978076788109338402, -22.46882643481310282, 11.49999999999998934 ) ) ;
#81288 = CARTESIAN_POINT ( 'NONE',  ( -41.17181748269097596, -25.18430928094562660, 3.555109957723386671 ) ) ;
#81289 = CARTESIAN_POINT ( 'NONE',  ( 5.326923076923078426, -5.876774720514419847, 20.76772836538461320 ) ) ;
#81290 = CARTESIAN_POINT ( 'NONE',  ( -19.20277006422315225, 10.48866939257135833, -1.500000000000002220 ) ) ;
#81291 = CARTESIAN_POINT ( 'NONE',  ( 7.081057417352553784, -5.876774720514423400, 21.11453472826393352 ) ) ;
#81292 = EDGE_LOOP ( 'NONE', ( #71534, #19372, #18623, #80163 ) ) ;
#81293 = DIRECTION ( 'NONE',  ( 0.000000000000000000, 0.000000000000000000, -1.000000000000000000 ) ) ;
#81295 = EDGE_CURVE ( 'NONE', #13356, #54341, #10100, .T. ) ;
#81294 = CARTESIAN_POINT ( 'NONE',  ( -126.5228709571500616, -24.65952944569305316, 1.056160979905707675 ) ) ;
#81296 = EDGE_CURVE ( 'NONE', #50699, #39987, #23370, .T. ) ;
#81297 = EDGE_LOOP ( 'NONE', ( #49738, #21706, #35775, #14110 ) ) ;
#81298 = CARTESIAN_POINT ( 'NONE',  ( -30.58447015329645069, -25.11083922187778583, 7.243003598645814556 ) ) ;
#81299 = VERTEX_POINT ( 'NONE', #38114 ) ;
#81300 = CARTESIAN_POINT ( 'NONE',  ( -27.86046284349297864, -6.376774720514426953, -8.091963836038765123 ) ) ;
#81301 = CARTESIAN_POINT ( 'NONE',  ( -0.04484292967123595236, -22.46947303600939705, 1.633150109380534509 ) ) ;
#81302 = CARTESIAN_POINT ( 'NONE',  ( 13.48273455363431772, -16.43370779934446801, 11.49999999999998934 ) ) ;
#81303 = DIRECTION ( 'NONE',  ( 3.773278334444166432E-23, -1.000000000000000000, 0.000000000000000000 ) ) ;
#81304 = CARTESIAN_POINT ( 'NONE',  ( -26.48766330312332684, -24.97064563520116920, 3.017960392606179543 ) ) ;
#81305 = B_SPLINE_CURVE_WITH_KNOTS ( 'NONE', 3,
 ( #81656, #95873, #17754, #80654, #80154, #12127 ),
 .UNSPECIFIED., .F., .F.,
 ( 4, 2, 4 ),
 ( 1.570887131794952276E-05, 0.001396322306279763675, 0.002776935741241577573 ),
 .UNSPECIFIED. ) ;
#81306 = ADVANCED_FACE ( 'NONE', ( #15274 ), #60973, .T. ) ;
#81307 = CARTESIAN_POINT ( 'NONE',  ( -85.56476876785632157, -23.48783264082476308, -1.443836473390098796 ) ) ;
#81308 = CARTESIAN_POINT ( 'NONE',  ( -68.60258773187044312, -23.73766607897669445, -1.055555164236457788 ) ) ;
#81309 = AXIS2_PLACEMENT_3D ( 'NONE', #79659, #10159, #37986 ) ;
#81310 = CARTESIAN_POINT ( 'NONE',  ( -117.5545740405765684, -24.15620529776629510, 10.23563542870659582 ) ) ;
#81311 = ORIENTED_EDGE ( 'NONE', *, *, #98676, .F. ) ;
#81312 = CARTESIAN_POINT ( 'NONE',  ( -19.37596289572233488, 2.755671585415585767, 11.49999999999999645 ) ) ;
#81313 = CARTESIAN_POINT ( 'NONE',  ( -95.55620429048337883, -23.48783264082478439, -1.443836473390061492 ) ) ;
#81314 = CARTESIAN_POINT ( 'NONE',  ( -28.07520560075130334, -24.67782888724788748, 8.218989154575222500 ) ) ;
#81315 = ORIENTED_EDGE ( 'NONE', *, *, #81113, .F. ) ;
#81316 = EDGE_CURVE ( 'NONE', #21767, #3088, #77167, .T. ) ;
#81317 = CARTESIAN_POINT ( 'NONE',  ( -46.62287095715004881, -29.50248528299804818, 1.056150453629033370 ) ) ;
#81318 = CARTESIAN_POINT ( 'NONE',  ( 2.100208336950355914, 2.204364238465233111E-16, -1.249999999999996003 ) ) ;
#81320 = EDGE_CURVE ( 'NONE', #77260, #99983, #77667, .T. ) ;
#81319 = PLANE ( 'NONE',  #76309 ) ;
#81321 = CARTESIAN_POINT ( 'NONE',  ( -81.52676753278062449, -25.24813894920551505, 7.119670133019518232 ) ) ;
#81322 = CARTESIAN_POINT ( 'NONE',  ( 15.15379598424239838, -12.58889634127381640, -1.500000000000002220 ) ) ;
#81323 = EDGE_CURVE ( 'NONE', #67443, #60922, #22121, .T. ) ;
#81324 = ORIENTED_EDGE ( 'NONE', *, *, #99352, .F. ) ;
#81325 = B_SPLINE_CURVE_WITH_KNOTS ( 'NONE', 3,
 ( #96312, #11075, #34914, #41532 ),
 .UNSPECIFIED., .F., .F.,
 ( 4, 4 ),
 ( 0.000000000000000000, 0.0001000000000000028644 ),
 .UNSPECIFIED. ) ;
#81326 = VECTOR ( 'NONE', #28926, 1000.000000000000114 ) ;
#81327 = CARTESIAN_POINT ( 'NONE',  ( 19.57151214508649772, 3.625915217019311583E-15, 0.5000000000000000000 ) ) ;
#81328 = CARTESIAN_POINT ( 'NONE',  ( 2.955024617976266033, -5.876774720514416295, 20.58370193283586858 ) ) ;
#81330 = ADVANCED_FACE ( 'NONE', ( #68081 ), #21876, .F. ) ;
#81329 = APPROVAL_STATUS ( 'not_yet_approved' ) ;
#81331 = ORIENTED_EDGE ( 'NONE', *, *, #72302, .F. ) ;
#81332 = CARTESIAN_POINT ( 'NONE',  ( 8.071512145086501278, -0.8690767389352472838, 3.741933809627420171 ) ) ;
#81333 = CARTESIAN_POINT ( 'NONE',  ( -103.5228709571500474, -24.66019654487200441, 8.947790411086119278 ) ) ;
#81334 = DIRECTION ( 'NONE',  ( -3.773278334453079618E-23, 0.9999999999976377785, 2.173523156925979975E-06 ) ) ;
#81335 = CARTESIAN_POINT ( 'NONE',  ( -84.62287095715008434, -23.47596703998600631, 11.44779298504227860 ) ) ;
#81336 = CARTESIAN_POINT ( 'NONE',  ( -119.5228709571501184, -24.33832256527049154, 0.1851278514138659792 ) ) ;
#81337 = CARTESIAN_POINT ( 'NONE',  ( -23.62875734969026453, 6.143225279485574397, 24.50402280011862288 ) ) ;
#81338 = CARTESIAN_POINT ( 'NONE',  ( -50.62287095715004881, -24.51163499207175178, 0.6490370598554262571 ) ) ;
#81339 = CARTESIAN_POINT ( 'NONE',  ( -17.52048005523606022, -9.576713672051738513, 11.49999999999998934 ) ) ;
#81340 = CARTESIAN_POINT ( 'NONE',  ( -59.62287095715005592, -24.50216790748100237, 0.6166512839513628164 ) ) ;
#81341 = CARTESIAN_POINT ( 'NONE',  ( -0.004567304949753520950, -22.99087264824203913, 3.851531674744869349 ) ) ;
#81342 = CARTESIAN_POINT ( 'NONE',  ( 19.23997954701083657, -5.074110557352235595, -1.500000000000002220 ) ) ;
#81343 = ORIENTED_EDGE ( 'NONE', *, *, #13716, .T. ) ;
#81344 = CARTESIAN_POINT ( 'NONE',  ( -74.55620429048342146, -24.64898659630528854, 1.056161002820828143 ) ) ;
#81345 = B_SPLINE_CURVE_WITH_KNOTS ( 'NONE', 3,
 ( #43380, #74318, #28641, #14897, #92523, #37746, #62592, #91529, #85412, #54979, #31125, #77785 ),
 .UNSPECIFIED., .F., .F.,
 ( 4, 2, 2, 2, 2, 4 ),
 ( 0.000000000000000000, 0.0004005021043489182409, 0.0008010042086978364818, 0.001201506313046754723, 0.001401757365221215036, 0.001602008417395675349 ),
 .UNSPECIFIED. ) ;
#81347 =( NAMED_UNIT ( * ) PLANE_ANGLE_UNIT ( ) SI_UNIT ( $, .RADIAN. ) );
#81346 = APPROVAL_PERSON_ORGANIZATION ( #63122, #85348, #78806 ) ;
#81348 = CARTESIAN_POINT ( 'NONE',  ( 29.68479148105952348, 4.772774720514425972, -9.431263391055120238 ) ) ;
#81349 = CARTESIAN_POINT ( 'NONE',  ( 6.783277369150963132, -3.316774720515097030, -28.31678455703255892 ) ) ;
#81350 = CARTESIAN_POINT ( 'NONE',  ( -16.26442346200556344, 12.93145763113255775, 11.49999999999999645 ) ) ;
#81351 = DIRECTION ( 'NONE',  ( 0.000000000000000000, 0.000000000000000000, -1.000000000000000000 ) ) ;
#81352 = CARTESIAN_POINT ( 'NONE',  ( -36.52287095715006870, -23.47593901973090169, -1.443836447538997314 ) ) ;
#81353 = CARTESIAN_POINT ( 'NONE',  ( -62.62287095715004881, -23.47596703998600276, 11.44779298504227505 ) ) ;
#81354 = VERTEX_POINT ( 'NONE', #94408 ) ;
#81355 = DIRECTION ( 'NONE',  ( -3.773278334453079618E-23, 0.9999999999976377785, 2.173523156925979975E-06 ) ) ;
#81356 = CARTESIAN_POINT ( 'NONE',  ( -127.6238341232833164, -24.34968618360935011, 0.1864209137778924386 ) ) ;
#81357 = ORIENTED_EDGE ( 'NONE', *, *, #52793, .F. ) ;
#81358 = CARTESIAN_POINT ( 'NONE',  ( -11.13811422090317294, 16.88724661786912762, 11.49999999999998934 ) ) ;
#81359 = B_SPLINE_CURVE_WITH_KNOTS ( 'NONE', 3,
 ( #61672, #38307, #30194, #92097, #13474, #84487, #54057, #249, #14466, #23067, #98711, #83988, #91102, #67793, #100182, #76362, #31191, #84982, #45448, #6865, #21577, #99689, #77358, #52550, #44947, #62165, #93089 ),
 .UNSPECIFIED., .F., .F.,
 ( 4, 1, 1, 1, 1, 1, 1, 1, 1, 1, 1, 1, 1, 1, 1, 1, 1, 1, 1, 1, 1, 1, 1, 1, 4 ),
 ( 0.000000000000000000, 0.06859462225874299324, 0.1332460424433017654, 0.1943125864682570259, 0.2512792231169669877, 0.3045134392563472181, 0.3542349066533249102, 0.4004805887739895653, 0.4434107549384915803, 0.4840148686163446845, 0.5232523007732032827, 0.5610423727283604389, 0.5979002393643996216, 0.6335184888561951055, 0.6683143511696515437, 0.7024956712863811292, 0.7366853535134582076, 0.7702931693607886210, 0.8034372550192486750, 0.8359129516660284143, 0.8684602457892908189, 0.9008465382431825041, 0.9334665246307077835, 0.9662575752981232835, 1.000000000000000000 ),
 .UNSPECIFIED. ) ;
#81360 = DIRECTION ( 'NONE',  ( -3.773278334453079030E-23, 0.9999999999976377785, 2.173523156925979128E-06 ) ) ;
#81361 = CARTESIAN_POINT ( 'NONE',  ( -129.6228709571500417, -24.64898659630367916, 1.056161002820834804 ) ) ;
#81362 = CARTESIAN_POINT ( 'NONE',  ( -109.6228709571500559, -23.47593901973091235, -1.443836447538999312 ) ) ;
#81363 = VERTEX_POINT ( 'NONE', #24891 ) ;
#81364 = CARTESIAN_POINT ( 'NONE',  ( -46.62287095715004881, -23.47596703998600276, 11.44779298504227505 ) ) ;
#81365 = CARTESIAN_POINT ( 'NONE',  ( -121.6228709571500417, -29.50250786944525672, 11.44777988621622811 ) ) ;
#81366 = CARTESIAN_POINT ( 'NONE',  ( -4.446071851354966853, 19.53225066162704948, -1.500000000000002220 ) ) ;
#81367 = CARTESIAN_POINT ( 'NONE',  ( -14.15979099334852798, -15.53166555317341135, 11.49999999999999645 ) ) ;
#81368 = LINE ( 'NONE', #58052, #76119 ) ;
#81369 = CARTESIAN_POINT ( 'NONE',  ( -70.61333134823995294, -23.48786465467241058, 11.44779295918254824 ) ) ;
#81370 = CARTESIAN_POINT ( 'NONE',  ( -17.20036718215007099, 13.84871166177648583, 11.49999999999998934 ) ) ;
#81371 = CARTESIAN_POINT ( 'NONE',  ( -47.52287095715007581, -23.47593901973090169, -1.443836447538997092 ) ) ;
#81372 = VECTOR ( 'NONE', #86536, 1000.000000000000000 ) ;
#81373 = EDGE_CURVE ( 'NONE', #22334, #13993, #12425, .T. ) ;
#81374 = CARTESIAN_POINT ( 'NONE',  ( -7.749999999999996447, 24.84999999999999787, 2.100000000000000089 ) ) ;
#81375 = CARTESIAN_POINT ( 'NONE',  ( -118.5895376238167245, -24.64898659630368627, 1.056161002820390937 ) ) ;
#81376 = CARTESIAN_POINT ( 'NONE',  ( -70.34543693012690824, -25.04307398257883577, 7.563174194274490780 ) ) ;
#81377 = CARTESIAN_POINT ( 'NONE',  ( -114.5228709571500616, -24.64965694238408034, 8.947790433994192938 ) ) ;
#81378 = ADVANCED_FACE ( 'NONE', ( #87806 ), #32514, .F. ) ;
#81379 = VERTEX_POINT ( 'NONE', #48250 ) ;
#81380 = ADVANCED_FACE ( 'NONE', ( #95414 ), #16783, .F. ) ;
#81381 = ORIENTED_EDGE ( 'NONE', *, *, #10028, .F. ) ;
#81382 = DIRECTION ( 'NONE',  ( 0.000000000000000000, 1.000000000000000000, 0.000000000000000000 ) ) ;
#81383 = CARTESIAN_POINT ( 'NONE',  ( -80.92287095715006728, -23.47596703998600631, 11.44779298504227860 ) ) ;
#81384 = CARTESIAN_POINT ( 'NONE',  ( -58.62287095715006302, -24.65952944569304250, 1.056160979905695463 ) ) ;
#81385 = CARTESIAN_POINT ( 'NONE',  ( -3.210669876418242197, 20.33209092710186638, -1.500000000000002220 ) ) ;
#81386 = EDGE_CURVE ( 'NONE', #17142, #78402, #54861, .T. ) ;
#81387 = CARTESIAN_POINT ( 'NONE',  ( -7.320277434469578459, 20.25297033093062282, 11.49999999999999645 ) ) ;
#81388 = ORIENTED_EDGE ( 'NONE', *, *, #22285, .F. ) ;
#81389 = DIRECTION ( 'NONE',  ( -3.773278334453080206E-23, 0.9999999999976377785, 2.173523156925979975E-06 ) ) ;
#81390 = CARTESIAN_POINT ( 'NONE',  ( 15.00000000000000533, 2.363568322354391830E-15, -19.30000000000000071 ) ) ;
#81391 = DIRECTION ( 'NONE',  ( 0.000000000000000000, 0.9999999999976377785, 2.173523156925979975E-06 ) ) ;
#81392 = CARTESIAN_POINT ( 'NONE',  ( 8.793911523065595759, -20.50603677605392150, -1.500000000000002220 ) ) ;
#81393 = EDGE_CURVE ( 'NONE', #72031, #15988, #82510, .T. ) ;
#81394 = EDGE_CURVE ( 'NONE', #75155, #32857, #74609, .T. ) ;
#81395 = CARTESIAN_POINT ( 'NONE',  ( -41.32836283488544638, -4.132774720514426292, 39.26872235229541985 ) ) ;
#81396 = CARTESIAN_POINT ( 'NONE',  ( -58.62287095715007013, -23.47596703998600276, 11.44779298504227683 ) ) ;
#81397 = ORIENTED_EDGE ( 'NONE', *, *, #73194, .F. ) ;
#81398 = CARTESIAN_POINT ( 'NONE',  ( -101.6228709571501128, -24.34917612406837861, 0.1852690917426677852 ) ) ;
#81399 = DIRECTION ( 'NONE',  ( 0.000000000000000000, 0.000000000000000000, 1.000000000000000000 ) ) ;
#81400 = VECTOR ( 'NONE', #95799, 1000.000000000000114 ) ;
#81401 = CARTESIAN_POINT ( 'NONE',  ( 8.688630223215852766, -18.96179456382524364, 11.49999999999998934 ) ) ;
#81402 = VECTOR ( 'NONE', #95077, 1000.000000000000000 ) ;
#81403 = VERTEX_POINT ( 'NONE', #55871 ) ;
#81405 = ORIENTED_EDGE ( 'NONE', *, *, #98851, .T. ) ;
#81404 = CARTESIAN_POINT ( 'NONE',  ( -39.73230706801754764, -25.13992894415259016, 3.001193081787598693 ) ) ;
#81406 = B_SPLINE_CURVE_WITH_KNOTS ( 'NONE', 3,
 ( #79899, #782, #278, #31734, #93120, #71807 ),
 .UNSPECIFIED., .F., .F.,
 ( 4, 2, 4 ),
 ( 6.391158118963033063E-06, 0.001387004593080784194, 0.002767618028042605031 ),
 .UNSPECIFIED. ) ;
#81407 = EDGE_LOOP ( 'NONE', ( #44492, #32249, #97951, #33082 ) ) ;
#81408 = FACE_OUTER_BOUND ( 'NONE', #491, .T. ) ;
#81409 = CARTESIAN_POINT ( 'NONE',  ( -19.68365937621761219, -7.520201837432793468, -1.500000000000002220 ) ) ;
#81410 = EDGE_LOOP ( 'NONE', ( #64345, #92600, #23725, #19796 ) ) ;
#81411 = DIRECTION ( 'NONE',  ( 0.9496245541219264785, 0.000000000000000000, 0.3133898629642195011 ) ) ;
#81412 = CARTESIAN_POINT ( 'NONE',  ( -98.52287095715006160, -23.48783264082477018, -1.443836473390087916 ) ) ;
#81413 = CARTESIAN_POINT ( 'NONE',  ( -105.5562042904833788, -25.00182538069145721, 7.747789668545099317 ) ) ;
#81414 = CARTESIAN_POINT ( 'NONE',  ( 8.971512145086528278, -9.528487854913501920, 6.500000000000001776 ) ) ;
#81415 = CARTESIAN_POINT ( 'NONE',  ( -49.15081903914613548, -25.23404858129530126, 3.683285954327154332 ) ) ;
#81416 = CARTESIAN_POINT ( 'NONE',  ( -17.03913561245058261, -13.47071831616118942, -1.500000000000002220 ) ) ;
#81417 = CARTESIAN_POINT ( 'NONE',  ( -81.35928118207723969, -25.12224291375864027, 6.638486925961360363 ) ) ;
#81419 = ORIENTED_EDGE ( 'NONE', *, *, #48972, .T. ) ;
#81418 = CARTESIAN_POINT ( 'NONE',  ( -7.755428854246955161, -20.87388092083558888, 11.49999999999999645 ) ) ;
#81420 = CARTESIAN_POINT ( 'NONE',  ( -50.41832839342763606, -25.24728723697485577, 5.198500959637132546 ) ) ;
#81421 = CARTESIAN_POINT ( 'NONE',  ( 14.61581676225028126, 3.316774720514426456, -27.35847991880135766 ) ) ;
#81422 = EDGE_CURVE ( 'NONE', #68434, #93569, #41369, .T. ) ;
#81423 = DIRECTION ( 'NONE',  ( -3.773278334453079030E-23, 0.9999999999976377785, 2.173523156925979128E-06 ) ) ;
#81424 = ORIENTED_EDGE ( 'NONE', *, *, #11460, .F. ) ;
#81426 = ORIENTED_EDGE ( 'NONE', *, *, #348, .T. ) ;
#81425 = CARTESIAN_POINT ( 'NONE',  ( -53.62287095715005592, -23.47593901973091235, -1.443836447539009749 ) ) ;
#81427 = CIRCLE ( 'NONE', #37658, 1.499999999999999556 ) ;
#81428 = EDGE_CURVE ( 'NONE', #75155, #54393, #61668, .T. ) ;
#81429 = ORIENTED_EDGE ( 'NONE', *, *, #55002, .T. ) ;
#81430 = CC_DESIGN_SECURITY_CLASSIFICATION ( #44192, ( #100423 ) ) ;
#81431 = CARTESIAN_POINT ( 'NONE',  ( -117.5228709571500758, -23.48786465467241769, 11.44779295918253759 ) ) ;
#81432 = DIRECTION ( 'NONE',  ( -7.960204194457801640E-17, -1.000000000000000000, -4.336808689942018722E-16 ) ) ;
#81434 = CARTESIAN_POINT ( 'NONE',  ( 31.52563388547018874, 4.132774720514424516, -1.605328387144967728 ) ) ;
#81433 = VECTOR ( 'NONE', #33777, 1000.000000000000000 ) ;
#81435 = FACE_OUTER_BOUND ( 'NONE', #15000, .T. ) ;
#81436 = EDGE_LOOP ( 'NONE', ( #84361, #68916, #4917, #37987 ) ) ;
#81437 = CARTESIAN_POINT ( 'NONE',  ( -13.57581083383196940, -5.876774720514426953, 20.21213203435597094 ) ) ;
#81438 = CARTESIAN_POINT ( 'NONE',  ( -21.16806448877717628, 7.570426553894726851, -1.500000000000002220 ) ) ;
#81439 = AXIS2_PLACEMENT_3D ( 'NONE', #91634, #100228, #46977 ) ;
#81440 = B_SPLINE_CURVE_WITH_KNOTS ( 'NONE', 3,
 ( #42567, #51162, #97824, #58775 ),
 .UNSPECIFIED., .F., .F.,
 ( 4, 4 ),
 ( 0.000000000000000000, 9.999999999998897304E-05 ),
 .UNSPECIFIED. ) ;
#81441 = VERTEX_POINT ( 'NONE', #71084 ) ;
#81442 = CARTESIAN_POINT ( 'NONE',  ( 22.02124265030973760, 6.143225279485574397, 16.20402280011862217 ) ) ;
#81443 = FACE_OUTER_BOUND ( 'NONE', #29105, .T. ) ;
#81444 = CARTESIAN_POINT ( 'NONE',  ( 7.732492003039795669, 3.316774720515257791, -27.16032169665734486 ) ) ;
#81445 = CARTESIAN_POINT ( 'NONE',  ( -116.5228709571500900, -23.72747288104470442, -1.053458166803225460 ) ) ;
#81446 = B_SPLINE_CURVE_WITH_KNOTS ( 'NONE', 3,
 ( #8892, #61203, #37845, #69796 ),
 .UNSPECIFIED., .F., .F.,
 ( 4, 4 ),
 ( 6.938893903907228378E-18, 0.0001000000000000028644 ),
 .UNSPECIFIED. ) ;
#81448 = EDGE_CURVE ( 'NONE', #42451, #48335, #37762, .T. ) ;
#81447 = CARTESIAN_POINT ( 'NONE',  ( -63.92072118931277203, -24.75152770810919733, 1.363349870542269082 ) ) ;
#81449 = CARTESIAN_POINT ( 'NONE',  ( -0.6043519431218743465, -19.59835197619436187, -1.500000000000002220 ) ) ;
#81450 = B_SPLINE_SURFACE_WITH_KNOTS ( 'NONE', 3, 3, ( 
 ( #70010, #87622, #72904, #46178 ),
 ( #3400, #18594, #18105, #31448 ),
 ( #57192, #93336, #79999, #78105 ),
 ( #65314, #33828, #1007, #495 ),
 ( #23320, #25711, #54303, #10486 ),
 ( #64815, #95730, #85231, #84730 ),
 ( #80501, #15718, #62411, #77107 ) ),
 .UNSPECIFIED., .F., .F., .F.,
 ( 4, 3, 4 ),
 ( 4, 4 ),
 ( 0.7945040050992244751, 0.8970133687736506767, 0.9995227324480768782 ),
 ( 0.7596870442490788466, 0.7610504907558764964 ),
 .UNSPECIFIED. ) ;
#81451 = CARTESIAN_POINT ( 'NONE',  ( -46.66195802986739949, -23.48783264082476663, -1.443836473390096575 ) ) ;
#81452 = VERTEX_POINT ( 'NONE', #9678 ) ;
#81453 = B_SPLINE_CURVE_WITH_KNOTS ( 'NONE', 3,
 ( #76660, #92898, #93397, #99994, #76169, #61474, #31005, #30001 ),
 .UNSPECIFIED., .F., .F.,
 ( 4, 2, 2, 4 ),
 ( 0.000000000000000000, 0.002001098010032688855, 0.003001647015049033283, 0.004002196020065377710 ),
 .UNSPECIFIED. ) ;
#81454 = CARTESIAN_POINT ( 'NONE',  ( 11.68953838083566588, 18.09531432177502808, -1.500000000000002220 ) ) ;
#81455 = CARTESIAN_POINT ( 'NONE',  ( -12.65407072091356433, 5.965225279485572685, -26.15404995688568590 ) ) ;
#81456 = CARTESIAN_POINT ( 'NONE',  ( -80.88693734264360558, -25.31572658427561962, 5.024145845486627238 ) ) ;
#81457 = CARTESIAN_POINT ( 'NONE',  ( -100.5895376238167245, -23.48783264082478794, -1.443836473390061936 ) ) ;
#81458 = EDGE_CURVE ( 'NONE', #56886, #95847, #78166, .T. ) ;
#81459 = LINE ( 'NONE', #58130, #71508 ) ;
#81460 = CARTESIAN_POINT ( 'NONE',  ( 16.94363762160741516, 15.55198921429254533, -1.500000000000002220 ) ) ;
#81461 = AXIS2_PLACEMENT_3D ( 'NONE', #82302, #58486, #44253 ) ;
#81462 = COORDINATED_UNIVERSAL_TIME_OFFSET ( 0, 0, .AHEAD. ) ;
#81463 = CARTESIAN_POINT ( 'NONE',  ( -101.6430330839730374, -25.27307239909451653, 3.986250617436227550 ) ) ;
#81464 = FACE_OUTER_BOUND ( 'NONE', #100326, .T. ) ;
#81465 = CARTESIAN_POINT ( 'NONE',  ( 19.44710440357065551, 5.058846670610233076, 11.49999999999999645 ) ) ;
#81466 = CARTESIAN_POINT ( 'NONE',  ( 17.51792015816173986, -5.965225279485572685, 29.01255224319336889 ) ) ;
#81467 = CARTESIAN_POINT ( 'NONE',  ( -81.88534077628074215, -25.23679622552714363, 6.293943003980942308 ) ) ;
#81468 = PRODUCT_DEFINITION_SHAPE ( 'NONE', 'NONE',  #100433 ) ;
#81469 = DIRECTION ( 'NONE',  ( -3.773278334444166432E-23, 1.000000000000000000, 0.000000000000000000 ) ) ;
#81470 = CARTESIAN_POINT ( 'NONE',  ( -65.62287095715002749, -24.91544648472619983, 1.928969306349235691 ) ) ;
#81471 = CARTESIAN_POINT ( 'NONE',  ( -125.6228709571500559, -29.50248528299804818, 1.056150453629047137 ) ) ;
#81472 = CARTESIAN_POINT ( 'NONE',  ( -18.24115112668064853, 7.888873183027880209, 11.49999999999998934 ) ) ;
#81473 = CARTESIAN_POINT ( 'NONE',  ( -113.6244797112919400, -24.51314013834316086, 0.6176544820404182845 ) ) ;
#81474 = CARTESIAN_POINT ( 'NONE',  ( 15.21843288076463629, 12.49332292251147614, -1.500000000000002220 ) ) ;
#81475 = DIRECTION ( 'NONE',  ( -1.000000000000000000, -0.000000000000000000, -0.000000000000000000 ) ) ;
#81476 = CONTEXT_DEPENDENT_SHAPE_REPRESENTATION ( #6405, #81468 ) ;
#81477 = VECTOR ( 'NONE', #14423, 1000.000000000000000 ) ;
#81478 = CARTESIAN_POINT ( 'NONE',  ( -57.52287095715005449, -24.64965694238407323, 8.947790433994201820 ) ) ;
#81479 = CARTESIAN_POINT ( 'NONE',  ( 13.10664265030973930, -5.965225279485574461, -28.64597719988137570 ) ) ;
#81480 = CARTESIAN_POINT ( 'NONE',  ( 1.582324178664715975, -20.54890914157308401, 11.49999999999999645 ) ) ;
#81481 = CARTESIAN_POINT ( 'NONE',  ( -128.5228709571501042, -23.73934037231758154, 11.05740245334327732 ) ) ;
#81482 = CARTESIAN_POINT ( 'NONE',  ( 21.95517018727266390, 5.574673621280945568, 11.49999999999999645 ) ) ;
#81483 = ORIENTED_EDGE ( 'NONE', *, *, #93228, .F. ) ;
#81484 = LINE ( 'NONE', #11958, #28107 ) ;
#81485 = CARTESIAN_POINT ( 'NONE',  ( -42.62287095715006302, -23.47596703998600276, 11.44779298504227505 ) ) ;
#81486 = CARTESIAN_POINT ( 'NONE',  ( -110.5228709571500900, -23.85196035786901092, -0.8779234886475162369 ) ) ;
#81487 = CARTESIAN_POINT ( 'NONE',  ( -2.656471864501908975, -6.376774720514411854, 19.66116880005639800 ) ) ;
#81488 = ORIENTED_EDGE ( 'NONE', *, *, #49638, .T. ) ;
#81489 = ORIENTED_EDGE ( 'NONE', *, *, #93611, .F. ) ;
#81490 = VECTOR ( 'NONE', #100391, 1000.000000000000114 ) ;
#81491 = FACE_OUTER_BOUND ( 'NONE', #91355, .T. ) ;
#81492 = CARTESIAN_POINT ( 'NONE',  ( 13.72848742581335912, -18.28091200367991576, 11.49999999999998934 ) ) ;
#81493 = DIRECTION ( 'NONE',  ( 1.000000000000000000, 0.000000000000000000, 0.000000000000000000 ) ) ;
#81494 = CARTESIAN_POINT ( 'NONE',  ( 21.32721141102669193, -3.434809268862642817, -1.500000000000002220 ) ) ;
#81495 = CARTESIAN_POINT ( 'NONE',  ( -113.6255546038343596, -24.35071581493543746, 9.817618358456018157 ) ) ;
#81496 = DIRECTION ( 'NONE',  ( -3.773278334453080206E-23, 0.9999999999976377785, 2.173523156925979975E-06 ) ) ;
#81497 = ORGANIZATION ( 'NAUO-ORG6', 'UNSPECIFIED', 'UNSPECIFIED' ) ;
#81498 = CARTESIAN_POINT ( 'NONE',  ( 8.566404662457630437, 20.85315857434707709, 11.49999999999999645 ) ) ;
#81499 = VERTEX_POINT ( 'NONE', #87296 ) ;
#81500 = DIRECTION ( 'NONE',  ( 1.000000000000000000, 0.000000000000000000, -1.743630241030147277E-15 ) ) ;
#81501 = CARTESIAN_POINT ( 'NONE',  ( 6.372119535971386917, -21.01724095701019479, -1.500000000000002220 ) ) ;
#81502 = CARTESIAN_POINT ( 'NONE',  ( -111.5905792267520127, -24.15543982623907482, -0.2315651400026575712 ) ) ;
#81503 = LINE ( 'NONE', #41953, #36293 ) ;
#81504 = AXIS2_PLACEMENT_3D ( 'NONE', #50268, #63119, #41664 ) ;
#81506 = ORIENTED_EDGE ( 'NONE', *, *, #95888, .F. ) ;
#81505 = EDGE_CURVE ( 'NONE', #60621, #63171, #13042, .T. ) ;
#81507 = DIRECTION ( 'NONE',  ( 0.000000000000000000, 0.000000000000000000, 1.000000000000000000 ) ) ;
#81508 = CARTESIAN_POINT ( 'NONE',  ( -0.2200237740140755516, -5.876774720514408301, 19.17724329193115551 ) ) ;
#81509 = ORIENTED_EDGE ( 'NONE', *, *, #24053, .F. ) ;
#81510 = CARTESIAN_POINT ( 'NONE',  ( -121.6228709571500417, -29.50250243563736774, 8.947779886222134493 ) ) ;
#81511 = EDGE_CURVE ( 'NONE', #7991, #89948, #24396, .T. ) ;
#81512 = ORIENTED_EDGE ( 'NONE', *, *, #83075, .T. ) ;
#81513 = VERTEX_POINT ( 'NONE', #72093 ) ;
#81514 = AXIS2_PLACEMENT_3D ( 'NONE', #86530, #95651, #17016 ) ;
#81515 = ORIENTED_EDGE ( 'NONE', *, *, #27057, .F. ) ;
#81516 = DIRECTION ( 'NONE',  ( 0.000000000000000000, -1.000000000000000000, 0.000000000000000000 ) ) ;
#81517 = DIRECTION ( 'NONE',  ( 1.000000000000000000, -2.209838822900391329E-16, 0.000000000000000000 ) ) ;
#81518 = CARTESIAN_POINT ( 'NONE',  ( 14.79186724892429439, 4.799335165223686417, -27.67512533972776723 ) ) ;
#81519 = CARTESIAN_POINT ( 'NONE',  ( 14.56535739210195857, -14.21638276092092745, -1.500000000000002220 ) ) ;
#81520 = ADVANCED_FACE ( 'NONE', ( #55364 ), #78307, .T. ) ;
#81521 = ORIENTED_EDGE ( 'NONE', *, *, #90780, .T. ) ;
#81522 = LINE ( 'NONE', #96246, #68782 ) ;
#81523 = CARTESIAN_POINT ( 'NONE',  ( -88.62287095715004170, -24.51283580621365132, 0.6167428607019744824 ) ) ;
#81524 = EDGE_CURVE ( 'NONE', #93008, #80349, #43630, .T. ) ;
#81525 = CARTESIAN_POINT ( 'NONE',  ( -105.5100292654264393, -24.73486907724918993, 1.287355809206962576 ) ) ;
#81526 = CARTESIAN_POINT ( 'NONE',  ( -71.66734858977571321, -25.03149629803908738, 6.551008863527044035 ) ) ;
#81527 = EDGE_LOOP ( 'NONE', ( #81606, #97732 ) ) ;
#81528 = DIRECTION ( 'NONE',  ( -3.773278334453080206E-23, 0.9999999999976377785, 2.173523156925979975E-06 ) ) ;
#81529 = CARTESIAN_POINT ( 'NONE',  ( -104.5228709571500758, -24.64965694238407323, 8.947790433994194714 ) ) ;
#81530 = EDGE_CURVE ( 'NONE', #100069, #89719, #43132, .T. ) ;
#81531 = ORIENTED_EDGE ( 'NONE', *, *, #89096, .T. ) ;
#81532 = EDGE_CURVE ( 'NONE', #22199, #13524, #60783, .T. ) ;
#81533 = CARTESIAN_POINT ( 'NONE',  ( -20.46667790307254009, -3.548193229090686796, -1.500000000000002220 ) ) ;
#81534 = ORIENTED_EDGE ( 'NONE', *, *, #52710, .T. ) ;
#81536 = EDGE_LOOP ( 'NONE', ( #6583, #66626, #6794, #9828, #28976 ) ) ;
#81535 = CARTESIAN_POINT ( 'NONE',  ( -13.89275734969026388, 5.965225279485572685, 31.02402280011862246 ) ) ;
#81537 = B_SPLINE_SURFACE_WITH_KNOTS ( 'NONE', 3, 1, ( 
 ( #84816, #54888 ),
 ( #70603, #91932 ),
 ( #15805, #83821 ),
 ( #62496, #46770 ),
 ( #77690, #14300 ),
 ( #30533, #6695 ),
 ( #585, #31031 ),
 ( #37649, #99528 ),
 ( #84316, #30026 ),
 ( #31532, #77192 ),
 ( #93425, #23918 ),
 ( #53387, #14798 ),
 ( #45764, #2111 ),
 ( #41165, #64026 ),
 ( #71615, #94941 ) ),
 .UNSPECIFIED., .F., .F., .F.,
 ( 4, 1, 1, 1, 1, 1, 1, 1, 1, 1, 1, 1, 4 ),
 ( 2, 2 ),
 ( 0.000000000000000000, 0.07964825118022765549, 0.1589216764181120567, 0.2396194947370321737, 0.3226094298185629428, 0.4060346366179267696, 0.4876020954923867556, 0.5696846265959313316, 0.6530361450088354447, 0.7374357177222916615, 0.8224778158555117180, 0.9097476551184092708, 1.000000000000000000 ),
 ( 0.000000000000000000, 1.000000000000000000 ),
 .UNSPECIFIED. ) ;
#81538 = CARTESIAN_POINT ( 'NONE',  ( -86.62287095715008434, -23.96127896941632685, -0.6493128931037817075 ) ) ;
#81539 = CARTESIAN_POINT ( 'NONE',  ( -97.52287095715009002, -24.51387760970724372, 9.387446482453396968 ) ) ;
#81540 = ORIENTED_EDGE ( 'NONE', *, *, #40806, .F. ) ;
#81541 = ORIENTED_EDGE ( 'NONE', *, *, #32476, .F. ) ;
#81542 = DIRECTION ( 'NONE',  ( 0.000000000000000000, 0.000000000000000000, -1.000000000000000000 ) ) ;
#81543 = LINE ( 'NONE', #27748, #90209 ) ;
#81544 = CARTESIAN_POINT ( 'NONE',  ( -5.023036858974361252, -5.876774720514410077, 19.14743589743590846 ) ) ;
#81545 = CARTESIAN_POINT ( 'NONE',  ( -71.24017339641436308, -25.31201710090048707, 5.863458149974889011 ) ) ;
#81547 = ORIENTED_EDGE ( 'NONE', *, *, #13559, .T. ) ;
#81546 = CARTESIAN_POINT ( 'NONE',  ( 14.53198226072946220, 16.64418356588832992, 11.49999999999999645 ) ) ;
#81548 = CARTESIAN_POINT ( 'NONE',  ( -113.5228709571500616, -24.64898659630368627, 1.056161002820831474 ) ) ;
#81549 = AXIS2_PLACEMENT_3D ( 'NONE', #77877, #29227, #60195 ) ;
#81550 = CARTESIAN_POINT ( 'NONE',  ( -22.51868310087907687, -2.221351303042197411, -1.500000000000002220 ) ) ;
#81552 = ORIENTED_EDGE ( 'NONE', *, *, #25976, .F. ) ;
#81551 = CARTESIAN_POINT ( 'NONE',  ( -115.6256581184850774, -24.63419186844613051, 9.035850630976923981 ) ) ;
#81553 = CIRCLE ( 'NONE', #31344, 0.2500000000000011102 ) ;
#81554 = ORIENTED_EDGE ( 'NONE', *, *, #728, .F. ) ;
#81555 = DIRECTION ( 'NONE',  ( 0.000000000000000000, 0.000000000000000000, 1.000000000000000000 ) ) ;
#81556 = CARTESIAN_POINT ( 'NONE',  ( -57.63243796231297722, -24.35071581493543036, 9.817618358456028815 ) ) ;
#81557 = VERTEX_POINT ( 'NONE', #88308 ) ;
#81558 = CARTESIAN_POINT ( 'NONE',  ( -6.202713861520617655, -20.23501359363181962, -1.500000000000002220 ) ) ;
#81559 = FACE_OUTER_BOUND ( 'NONE', #44369, .T. ) ;
#81560 = LINE ( 'NONE', #12035, #17902 ) ;
#81561 = CARTESIAN_POINT ( 'NONE',  ( 13.23790625878087468, -17.95846084735695314, -1.500000000000002220 ) ) ;
#81562 = CARTESIAN_POINT ( 'NONE',  ( -46.62287095715004881, -23.47593901973091235, -1.443836447539009749 ) ) ;
#81563 = ORIENTED_EDGE ( 'NONE', *, *, #96779, .F. ) ;
#81564 = CARTESIAN_POINT ( 'NONE',  ( -5.382328594919684406, -6.376774720514413630, 19.61227901093090864 ) ) ;
#81565 = CARTESIAN_POINT ( 'NONE',  ( 13.10664265030973930, 5.965225279485574461, -27.62597719988137612 ) ) ;
#81566 = CARTESIAN_POINT ( 'NONE',  ( -111.5562042904833788, -24.65952944569305316, 1.056160979905704567 ) ) ;
#81567 = CARTESIAN_POINT ( 'NONE',  ( 0.000000000000000000, -5.876774720514426953, 0.000000000000000000 ) ) ;
#81568 = VECTOR ( 'NONE', #56284, 1000.000000000000000 ) ;
#81569 = CARTESIAN_POINT ( 'NONE',  ( -16.16875682573952133, 10.94412424577950915, 11.49999999999998934 ) ) ;
#81570 = CARTESIAN_POINT ( 'NONE',  ( 2.169945595249806125, 21.32849103866527329, -1.500000000000002220 ) ) ;
#81571 = CARTESIAN_POINT ( 'NONE',  ( -26.36451126669314604, -24.92774786267114351, 2.180457190752079999 ) ) ;
#81572 = CARTESIAN_POINT ( 'NONE',  ( -60.62287095715004881, -29.50250786944525672, 11.44777988621623876 ) ) ;
#81573 = CARTESIAN_POINT ( 'NONE',  ( -77.64774600778000035, -23.48783264082476663, -1.443836473390097241 ) ) ;
#81574 = ADVANCED_FACE ( 'NONE', ( #19772 ), #42647, .F. ) ;
#81575 = CARTESIAN_POINT ( 'NONE',  ( -18.62658236799572720, 13.20813282334384553, -1.500000000000002220 ) ) ;
#81576 = VECTOR ( 'NONE', #81967, 1000.000000000000114 ) ;
#81577 = EDGE_CURVE ( 'NONE', #1598, #77838, #8652, .T. ) ;
#81578 = DIRECTION ( 'NONE',  ( -1.000000000000000000, -9.044818380534024011E-19, 3.498155517982143549E-15 ) ) ;
#81579 = CARTESIAN_POINT ( 'NONE',  ( -106.6282279683493357, -24.15620529776629510, 10.23563542870659582 ) ) ;
#81580 = CARTESIAN_POINT ( 'NONE',  ( -17.64648606763744354, -5.965225279485594001, -23.04404205923972526 ) ) ;
#81581 = CARTESIAN_POINT ( 'NONE',  ( 1.402406813841059030, 19.88454085074057076, 11.49999999999999645 ) ) ;
#81582 = CARTESIAN_POINT ( 'NONE',  ( -104.5872775516450162, -24.51314013834316796, 0.6176544820404187286 ) ) ;
#81583 = VECTOR ( 'NONE', #38620, 1000.000000000000000 ) ;
#81584 = CARTESIAN_POINT ( 'NONE',  ( -88.88918693012689687, -25.27880950044345454, 5.947789066509454159 ) ) ;
#81585 = CARTESIAN_POINT ( 'NONE',  ( -101.6228709571500559, -23.47593901973091235, -1.443836447539001089 ) ) ;
#81586 = ORIENTED_EDGE ( 'NONE', *, *, #33541, .F. ) ;
#81587 = CARTESIAN_POINT ( 'NONE',  ( 16.89397143409390623, -5.876774720514426953, 16.89397143409405899 ) ) ;
#81588 = CARTESIAN_POINT ( 'NONE',  ( -62.62287095715004881, -23.72773821059535848, 11.05748984161097503 ) ) ;
#81589 = CARTESIAN_POINT ( 'NONE',  ( -1.268225406894735396, -21.67698866206750097, -1.500000000000002220 ) ) ;
#81590 = CARTESIAN_POINT ( 'NONE',  ( -1.877194073982709988, 8.794404527355018431, -9.000000000000000000 ) ) ;
#81591 = CARTESIAN_POINT ( 'NONE',  ( -19.30006219055749739, -3.230038287793697283, -1.500000000000002220 ) ) ;
#81592 = FACE_OUTER_BOUND ( 'NONE', #13091, .T. ) ;
#81593 = DIRECTION ( 'NONE',  ( -1.889676989081488347E-15, 0.000000000000000000, -1.000000000000000000 ) ) ;
#81594 = CARTESIAN_POINT ( 'NONE',  ( 20.25987197511681259, 2.754759976156288204, 11.49999999999999645 ) ) ;
#81595 = CARTESIAN_POINT ( 'NONE',  ( -50.37830952628070946, -25.30401792888237367, 5.197789011716579033 ) ) ;
#81596 = ADVANCED_FACE ( 'NONE', ( #51745 ), #51237, .F. ) ;
#81597 = CARTESIAN_POINT ( 'NONE',  ( -108.8968792378191921, -29.50249817218807635, 6.986241424688308221 ) ) ;
#81598 = B_SPLINE_CURVE_WITH_KNOTS ( 'NONE', 3,
 ( #71041, #41094, #32978, #9128 ),
 .UNSPECIFIED., .F., .F.,
 ( 4, 4 ),
 ( 0.000000000000000000, 0.0001000000000000028644 ),
 .UNSPECIFIED. ) ;
#81599 = ORIENTED_EDGE ( 'NONE', *, *, #93430, .F. ) ;
#81600 = CARTESIAN_POINT ( 'NONE',  ( -5.366453405989236813, 2.265596578422603396E-15, -18.50000000000000000 ) ) ;
#81601 = DIRECTION ( 'NONE',  ( 1.000000000000000000, 3.773278334444167608E-23, 8.201307833595939069E-29 ) ) ;
#81602 = FACE_OUTER_BOUND ( 'NONE', #1117, .T. ) ;
#81603 = B_SPLINE_CURVE_WITH_KNOTS ( 'NONE', 3,
 ( #42986, #51091, #82035, #44476, #5901, #74420, #81544 ),
 .UNSPECIFIED., .F., .F.,
 ( 4, 1, 1, 1, 4 ),
 ( 0.000000000000000000, 0.2537340756906634187, 0.5030351201318574716, 0.7500135973308806880, 1.000000000000000000 ),
 .UNSPECIFIED. ) ;
#81604 = PLANE ( 'NONE',  #87305 ) ;
#81605 = AXIS2_PLACEMENT_3D ( 'NONE', #90765, #22231, #44597 ) ;
#81606 = ORIENTED_EDGE ( 'NONE', *, *, #93858, .T. ) ;
#81607 = CARTESIAN_POINT ( 'NONE',  ( -79.11611000704996854, -25.14083923594767001, 2.947789366383933185 ) ) ;
#81608 = CARTESIAN_POINT ( 'NONE',  ( -5.582908757718670678, 22.30220962497079285, 11.49999999999999645 ) ) ;
#81609 = CARTESIAN_POINT ( 'NONE',  ( -0.9122204482399535186, 22.77315974801211240, -1.500000000000002220 ) ) ;
#81610 = CARTESIAN_POINT ( 'NONE',  ( -70.70614159023084255, -25.05208580739551039, 7.521011471076567645 ) ) ;
#81611 = AXIS2_PLACEMENT_3D ( 'NONE', #3397, #50062, #12973 ) ;
#81612 = CARTESIAN_POINT ( 'NONE',  ( -40.52287095715004028, -24.82558206586148941, 1.605769216559624457 ) ) ;
#81613 = FACE_OUTER_BOUND ( 'NONE', #42833, .T. ) ;
#81614 = CARTESIAN_POINT ( 'NONE',  ( -78.62287095715004170, -23.48786465467241413, 11.44779295918254469 ) ) ;
#81615 = DIRECTION ( 'NONE',  ( 0.7071067811865474617, 0.000000000000000000, 0.7071067811865474617 ) ) ;
#81616 = CARTESIAN_POINT ( 'NONE',  ( -21.85961425739535358, 0.8689724601130633941, -1.500000000000002220 ) ) ;
#81617 = PLANE ( 'NONE',  #68911 ) ;
#81618 = CARTESIAN_POINT ( 'NONE',  ( -67.62287095715005592, -29.50250786944525672, 11.44777988621623699 ) ) ;
#81619 = CARTESIAN_POINT ( 'NONE',  ( -71.50915260164352105, -25.29966242988960090, 5.397575489595221931 ) ) ;
#81620 = CARTESIAN_POINT ( 'NONE',  ( 11.05000000000000426, -2.000000000000000888, 24.00000000000000000 ) ) ;
#81621 = ORIENTED_EDGE ( 'NONE', *, *, #53351, .F. ) ;
#81622 = CARTESIAN_POINT ( 'NONE',  ( 12.15263457413992576, -16.39098610538439615, -1.500000000000002220 ) ) ;
#81623 = ORIENTED_EDGE ( 'NONE', *, *, #89891, .F. ) ;
#81624 = ORIENTED_EDGE ( 'NONE', *, *, #91146, .T. ) ;
#81625 = ORIENTED_EDGE ( 'NONE', *, *, #81320, .T. ) ;
#81626 = EDGE_LOOP ( 'NONE', ( #247, #81839, #67710, #12014 ) ) ;
#81627 = B_SPLINE_CURVE_WITH_KNOTS ( 'NONE', 3,
 ( #77729, #86367, #16851, #8244 ),
 .UNSPECIFIED., .F., .F.,
 ( 4, 4 ),
 ( 0.000000000000000000, 0.0001000000000000167422 ),
 .UNSPECIFIED. ) ;
#81628 = CARTESIAN_POINT ( 'NONE',  ( -11.96207688724106610, 19.68918167733909641, -1.500000000000002220 ) ) ;
#81629 = DIRECTION ( 'NONE',  ( -3.773278334453080206E-23, 0.9999999999976377785, 2.173523156925979975E-06 ) ) ;
#81630 = CARTESIAN_POINT ( 'NONE',  ( 20.19498477198788322, 0.2509159868347127231, -1.500000000000002220 ) ) ;
#81631 = EDGE_CURVE ( 'NONE', #47607, #16500, #26805, .T. ) ;
#81632 = ORIENTED_EDGE ( 'NONE', *, *, #58068, .F. ) ;
#81633 = CARTESIAN_POINT ( 'NONE',  ( -69.55620429048340725, -23.47596703998600276, 11.44779298504227505 ) ) ;
#81634 = CARTESIAN_POINT ( 'NONE',  ( -34.55620429048339304, -24.64965694238574656, 8.947790433994203596 ) ) ;
#81635 = DIRECTION ( 'NONE',  ( 0.000000000000000000, -2.173523156925979552E-06, 0.9999999999976378895 ) ) ;
#81636 = LINE ( 'NONE', #19716, #88550 ) ;
#81638 = ORIENTED_EDGE ( 'NONE', *, *, #99818, .T. ) ;
#81637 = CARTESIAN_POINT ( 'NONE',  ( 20.27498964588844643, 6.839650151297337999, 11.49999999999999645 ) ) ;
#81639 = PLANE ( 'NONE',  #11169 ) ;
#81640 = ADVANCED_FACE ( 'NONE', ( #5059 ), #44129, .F. ) ;
#81641 = ORIENTED_EDGE ( 'NONE', *, *, #26756, .T. ) ;
#81642 = CARTESIAN_POINT ( 'NONE',  ( 10.43072250204971851, -19.66636941823637841, -1.500000000000002220 ) ) ;
#81643 = EDGE_CURVE ( 'NONE', #84023, #34094, #92207, .T. ) ;
#81644 = CARTESIAN_POINT ( 'NONE',  ( -17.26476610439243231, 11.37957233835482818, -1.500000000000002220 ) ) ;
#81646 = ORIENTED_EDGE ( 'NONE', *, *, #3748, .T. ) ;
#81645 = AXIS2_PLACEMENT_3D ( 'NONE', #43141, #81698, #12170 ) ;
#81647 = CARTESIAN_POINT ( 'NONE',  ( 13.91401389203221406, 5.965225279485572685, 27.75920385068456042 ) ) ;
#81648 = EDGE_LOOP ( 'NONE', ( #49559, #45952, #33655, #30579 ) ) ;
#81649 = LINE ( 'NONE', #34974, #34812 ) ;
#81650 = ORIENTED_EDGE ( 'NONE', *, *, #90702, .T. ) ;
#81651 = AXIS2_PLACEMENT_3D ( 'NONE', #29894, #38009, #60372 ) ;
#81652 = CARTESIAN_POINT ( 'NONE',  ( -10.40290173325841216, -6.376774720514426953, 27.45402280011861862 ) ) ;
#81653 = CARTESIAN_POINT ( 'NONE',  ( -12.66259425867894350, -16.64798919286708667, -1.500000000000002220 ) ) ;
#81654 = EDGE_CURVE ( 'NONE', #18679, #78997, #49760, .T. ) ;
#81655 = CARTESIAN_POINT ( 'NONE',  ( -12.72821696145241255, -17.84489267850806726, 11.49999999999999645 ) ) ;
#81656 = CARTESIAN_POINT ( 'NONE',  ( -107.6228709571500701, -24.66019654487199730, 8.947790411086124607 ) ) ;
#81657 = CARTESIAN_POINT ( 'NONE',  ( 3.368619518803146029, -22.26131067175759881, -1.500000000000002220 ) ) ;
#81658 = CARTESIAN_POINT ( 'NONE',  ( 19.95448254803897115, -6.385634049875297258, -1.500000000000002220 ) ) ;
#81659 = CARTESIAN_POINT ( 'NONE',  ( -38.53901505288835239, -24.34968618360933590, 0.1864209137778850278 ) ) ;
#81660 = CARTESIAN_POINT ( 'NONE',  ( 29.68479148105952348, -4.772774720514425972, -9.431263391055123790 ) ) ;
#81661 = CARTESIAN_POINT ( 'NONE',  ( -119.6256459593364383, -24.15620529776629510, 10.23563542870659582 ) ) ;
#81662 = CARTESIAN_POINT ( 'NONE',  ( -32.50560602629348494, -24.87219037988797865, 1.747789950295646877 ) ) ;
#81663 = VERTEX_POINT ( 'NONE', #65494 ) ;
#81664 = VERTEX_POINT ( 'NONE', #83676 ) ;
#81665 = EDGE_LOOP ( 'NONE', ( #90048, #55742, #11332, #18974 ) ) ;
#81666 = CARTESIAN_POINT ( 'NONE',  ( -44.52287095715008292, -23.96177878511308990, 10.65340807706330395 ) ) ;
#81667 = ORIENTED_EDGE ( 'NONE', *, *, #64019, .T. ) ;
#81668 = CARTESIAN_POINT ( 'NONE',  ( 18.29419249859179786, 11.19154738541161365, -1.500000000000002220 ) ) ;
#81669 = CARTESIAN_POINT ( 'NONE',  ( -95.58953762381672448, -23.47593901973091235, -1.443836447539001089 ) ) ;
#81670 = VERTEX_POINT ( 'NONE', #61861 ) ;
#81671 = CARTESIAN_POINT ( 'NONE',  ( 20.99878002148846790, -2.064974809011826729, -1.500000000000002220 ) ) ;
#81672 = CARTESIAN_POINT ( 'NONE',  ( -92.55620429048339304, -24.64965694238574656, 8.947790433994201820 ) ) ;
#81673 = CARTESIAN_POINT ( 'NONE',  ( 2.589743589743596086, -6.376774720514415407, 20.00140224358974095 ) ) ;
#81674 = CARTESIAN_POINT ( 'NONE',  ( -50.60991402953558804, -23.85049219812685095, 10.88485053497527133 ) ) ;
#81675 = LINE ( 'NONE', #96898, #58843 ) ;
#81676 = CARTESIAN_POINT ( 'NONE',  ( -109.4926097204045163, -25.31342473612490096, 4.739357423808571390 ) ) ;
#81677 = CARTESIAN_POINT ( 'NONE',  ( -12.21066354923914865, 18.40238043084326591, -1.500000000000002220 ) ) ;
#81678 = ORIENTED_EDGE ( 'NONE', *, *, #6286, .F. ) ;
#81679 = LINE ( 'NONE', #52726, #42190 ) ;
#81680 = B_SPLINE_CURVE_WITH_KNOTS ( 'NONE', 3,
 ( #38364, #30752, #8915, #92643 ),
 .UNSPECIFIED., .F., .F.,
 ( 4, 4 ),
 ( 0.000000000000000000, 9.999999999997510880E-05 ),
 .UNSPECIFIED. ) ;
#81681 = VECTOR ( 'NONE', #49936, 1000.000000000000114 ) ;
#81682 = CARTESIAN_POINT ( 'NONE',  ( -51.90278039571972357, -25.31633292683138237, 5.898133778068365807 ) ) ;
#81683 = CARTESIAN_POINT ( 'NONE',  ( -40.53889064818358889, -25.31624741514509935, 5.542732875838958684 ) ) ;
#81684 = EDGE_CURVE ( 'NONE', #64573, #36349, #28895, .T. ) ;
#81685 = CARTESIAN_POINT ( 'NONE',  ( -25.51311700692786388, -24.74886220813050031, 2.662461283694073089 ) ) ;
#81686 = AXIS2_PLACEMENT_3D ( 'NONE', #56437, #48313, #8242 ) ;
#81687 = CARTESIAN_POINT ( 'NONE',  ( -63.52287095715010423, -23.96127896941632329, -0.6493128931038021356 ) ) ;
#81688 = CARTESIAN_POINT ( 'NONE',  ( 13.79380260783658407, 16.28676726024703214, -1.500000000000002220 ) ) ;
#81689 = CARTESIAN_POINT ( 'NONE',  ( -26.25113031250881690, -24.91578880384921391, 6.269870734223003339 ) ) ;
#81690 = CARTESIAN_POINT ( 'NONE',  ( -50.91630580738321754, -25.32724633150699489, 4.398074151685129607 ) ) ;
#81691 = EDGE_CURVE ( 'NONE', #93833, #70270, #54664, .T. ) ;
#81692 = CARTESIAN_POINT ( 'NONE',  ( -86.62287095715004170, -24.64898659630528854, 1.056161002820827921 ) ) ;
#81693 = DIRECTION ( 'NONE',  ( -1.000000000000000000, -3.773278334444167608E-23, -8.201307833595939069E-29 ) ) ;
#81694 = CARTESIAN_POINT ( 'NONE',  ( 17.19246737676917292, 14.74310579602587090, -1.500000000000002220 ) ) ;
#81695 = CARTESIAN_POINT ( 'NONE',  ( -32.92287095715006018, -23.47596703998600276, 11.44779298504227683 ) ) ;
#81696 = VERTEX_POINT ( 'NONE', #52737 ) ;
#81697 = CARTESIAN_POINT ( 'NONE',  ( 12.20502328318355545, 3.316774720514426011, -28.10533714397569582 ) ) ;
#81698 = DIRECTION ( 'NONE',  ( 0.000000000000000000, 1.000000000000000000, -0.000000000000000000 ) ) ;
#81699 = CARTESIAN_POINT ( 'NONE',  ( -18.42202159362721048, -7.168033771007030097, 11.49999999999999645 ) ) ;
#81700 = CARTESIAN_POINT ( 'NONE',  ( -122.5228709571500616, -24.66019654487200441, 8.947790411086112172 ) ) ;
#81701 = CARTESIAN_POINT ( 'NONE',  ( -32.07722060962682775, -25.11010177581465186, 2.831122766525584478 ) ) ;
#81702 = VERTEX_POINT ( 'NONE', #60861 ) ;
#81703 = FACE_OUTER_BOUND ( 'NONE', #73067, .T. ) ;
#81704 = CARTESIAN_POINT ( 'NONE',  ( -28.91304442625643034, -24.60093986950708356, 2.072904486375534816 ) ) ;
#81705 = CARTESIAN_POINT ( 'NONE',  ( -113.5895376238167245, -24.64898659630368627, 1.056161002820388717 ) ) ;
#81706 = CARTESIAN_POINT ( 'NONE',  ( -20.67203406374276398, -6.343553224398504220, 11.49999999999998934 ) ) ;
#81707 = CARTESIAN_POINT ( 'NONE',  ( -106.5228709571500758, -24.65952944569305316, 1.056160979905704123 ) ) ;
#81708 = CARTESIAN_POINT ( 'NONE',  ( -19.35591191756920892, -0.7100623379298715010, -1.500000000000002220 ) ) ;
#81709 = DIRECTION ( 'NONE',  ( 0.000000000000000000, 1.000000000000000000, -0.000000000000000000 ) ) ;
#81710 = DIRECTION ( 'NONE',  ( -0.000000000000000000, -0.000000000000000000, -1.000000000000000000 ) ) ;
#81711 = CARTESIAN_POINT ( 'NONE',  ( -14.06767371131996214, 13.90018863433869889, -1.500000000000002220 ) ) ;
#81712 = EDGE_LOOP ( 'NONE', ( #97849, #30428, #22060, #54695 ) ) ;
#81713 = CARTESIAN_POINT ( 'NONE',  ( 20.02926185082240451, -2.967945350358753398, 11.49999999999999645 ) ) ;
#81714 = CARTESIAN_POINT ( 'NONE',  ( -119.5228709571500900, -24.51387760970726148, 9.387446482453405849 ) ) ;
#81715 = CC_DESIGN_PERSON_AND_ORGANIZATION_ASSIGNMENT ( #76931, #8439, ( #21292 ) ) ;
#81716 = LINE ( 'NONE', #58394, #42521 ) ;
#81717 = EDGE_LOOP ( 'NONE', ( #61833, #88149, #96465, #31176 ) ) ;
#81718 = B_SPLINE_SURFACE_WITH_KNOTS ( 'NONE', 3, 3, ( 
 ( #7660, #8165, #71074, #10168 ),
 ( #55857, #32504, #42139, #72083 ),
 ( #87283, #49750, #48747, #33501 ),
 ( #18279, #24880, #86783, #64985 ),
 ( #73079, #3069, #33009, #71577 ),
 ( #56863, #63476, #96401, #9669 ),
 ( #11164, #57365, #88297, #63984 ),
 ( #50238, #95899, #26395, #2565 ),
 ( #1564, #18768, #49251, #26891 ),
 ( #40623, #95402, #57863, #81177 ) ),
 .UNSPECIFIED., .F., .F., .F.,
 ( 4, 3, 3, 4 ),
 ( 4, 4 ),
 ( 0.7022005934544806038, 0.7765311282028795059, 0.8508616629512784080, 0.9995227324480763231 ),
 ( 0.6495723911733531919, 0.6509722519778085026 ),
 .UNSPECIFIED. ) ;
#81719 = CARTESIAN_POINT ( 'NONE',  ( -100.1844657475011218, -25.30123273641313375, 4.676267690568757907 ) ) ;
#81720 = FACE_OUTER_BOUND ( 'NONE', #77624, .T. ) ;
#81721 = DIRECTION ( 'NONE',  ( 0.000000000000000000, -0.000000000000000000, -1.000000000000000000 ) ) ;
#81722 = CARTESIAN_POINT ( 'NONE',  ( -92.62287095715005592, -24.66019654487199730, 8.947790411086124607 ) ) ;
#81723 = LINE ( 'NONE', #74113, #4131 ) ;
#81724 = CARTESIAN_POINT ( 'NONE',  ( 12.62869658624171976, -15.57725692549414376, 11.49999999999998934 ) ) ;
#81725 = DIRECTION ( 'NONE',  ( 0.000000000000000000, -0.000000000000000000, -1.000000000000000000 ) ) ;
#81726 = ORIENTED_EDGE ( 'NONE', *, *, #48405, .F. ) ;
#81727 = EDGE_CURVE ( 'NONE', #84492, #65087, #31640, .T. ) ;
#81728 = CARTESIAN_POINT ( 'NONE',  ( -103.5228709571500758, -24.51387760970725083, 9.387446482453407626 ) ) ;
#81729 = CARTESIAN_POINT ( 'NONE',  ( -82.52287095715006160, -24.65952944569304606, 1.056160979905698794 ) ) ;
#81730 = PLANE ( 'NONE',  #59773 ) ;
#81731 = CARTESIAN_POINT ( 'NONE',  ( -1.044871794871793602, -6.376774720514418959, 20.44941907051282115 ) ) ;
#81732 = AXIS2_PLACEMENT_3D ( 'NONE', #24537, #55506, #64137 ) ;
#81733 = DIRECTION ( 'NONE',  ( 2.910297583984928910E-15, -1.000000000000000000, -3.056206645085457922E-15 ) ) ;
#81734 = CARTESIAN_POINT ( 'NONE',  ( -49.26280096340228454, -25.29440776045719730, 5.833784451200525467 ) ) ;
#81735 = ORIENTED_EDGE ( 'NONE', *, *, #98908, .F. ) ;
#81736 = CARTESIAN_POINT ( 'NONE',  ( 5.487062353440709472, 19.58251264919930534, -1.500000000000002220 ) ) ;
#81737 = EDGE_LOOP ( 'NONE', ( #31328, #36010, #56192, #72112 ) ) ;
#81738 = EDGE_CURVE ( 'NONE', #24018, #85384, #54249, .T. ) ;
#81739 = CARTESIAN_POINT ( 'NONE',  ( -20.69623851537618364, -9.862649113751288610, -1.500000000000002220 ) ) ;
#81740 = CARTESIAN_POINT ( 'NONE',  ( 29.62673903083957683, 5.344535611318891988, 28.45872576146958011 ) ) ;
#81741 = AXIS2_PLACEMENT_3D ( 'NONE', #72032, #70519, #47689 ) ;
#81742 = VERTEX_POINT ( 'NONE', #46129 ) ;
#81743 = CARTESIAN_POINT ( 'NONE',  ( -108.5228709571500758, -24.35013146730204170, 9.818937971375099494 ) ) ;
#81744 = CARTESIAN_POINT ( 'NONE',  ( 15.26487859601603780, 3.572416542244653659, -27.19734615108692211 ) ) ;
#81745 = B_SPLINE_CURVE_WITH_KNOTS ( 'NONE', 3,
 ( #7511, #88152, #2417, #26745, #41989, #18621 ),
 .UNSPECIFIED., .F., .F.,
 ( 4, 2, 4 ),
 ( 0.000000000000000000, 0.001380764517853252720, 0.002761529035706505441 ),
 .UNSPECIFIED. ) ;
#81746 = DIRECTION ( 'NONE',  ( 0.000000000000000000, 0.000000000000000000, -1.000000000000000000 ) ) ;
#81747 = CARTESIAN_POINT ( 'NONE',  ( 16.91677535067316995, -12.78530099663392505, 11.49999999999999645 ) ) ;
#81748 = ADVANCED_FACE ( 'NONE', ( #77552 ), #8055, .T. ) ;
#81749 = CARTESIAN_POINT ( 'NONE',  ( -5.843409716339609261, -21.38298466452703650, -1.500000000000002220 ) ) ;
#81750 = EDGE_CURVE ( 'NONE', #97480, #7329, #1480, .T. ) ;
#81751 = CARTESIAN_POINT ( 'NONE',  ( -7.762539992054180438, 19.06225842855939234, 11.49999999999998934 ) ) ;
#81752 = B_SPLINE_CURVE_WITH_KNOTS ( 'NONE', 3,
 ( #18364, #49332, #26486, #71658, #10757, #2157 ),
 .UNSPECIFIED., .F., .F.,
 ( 4, 2, 4 ),
 ( 1.570755371633856203E-05, 0.001396183895866086235, 0.002776660238015833844 ),
 .UNSPECIFIED. ) ;
#81753 = ORIENTED_EDGE ( 'NONE', *, *, #78139, .F. ) ;
#81754 = ORIENTED_EDGE ( 'NONE', *, *, #99415, .F. ) ;
#81755 = DIRECTION ( 'NONE',  ( -0.000000000000000000, 1.000000000000000000, -0.000000000000000000 ) ) ;
#81756 = CARTESIAN_POINT ( 'NONE',  ( 13.91401389203221406, -5.965225279485572685, 158.0376437107427137 ) ) ;
#81757 = ORIENTED_EDGE ( 'NONE', *, *, #71330, .F. ) ;
#81758 = ORIENTED_EDGE ( 'NONE', *, *, #58768, .F. ) ;
#81759 = ORIENTED_EDGE ( 'NONE', *, *, #51163, .T. ) ;
#81760 = CARTESIAN_POINT ( 'NONE',  ( -116.6228709571500701, -24.50321055353807864, 9.387540953477524042 ) ) ;
#81761 = CARTESIAN_POINT ( 'NONE',  ( -46.52287095715008292, -23.72747288104470442, -1.053458166803227680 ) ) ;
#81762 = LINE ( 'NONE', #97484, #77847 ) ;
#81763 = CARTESIAN_POINT ( 'NONE',  ( 6.705275102110877405, 19.67741782454948662, -1.500000000000002220 ) ) ;
#81764 = EDGE_CURVE ( 'NONE', #86782, #24870, #68958, .T. ) ;
#81765 = CARTESIAN_POINT ( 'NONE',  ( 0.4029737066630413311, -21.70969715354747009, 11.49999999999999645 ) ) ;
#81766 = VERTEX_POINT ( 'NONE', #7056 ) ;
#81767 = DIRECTION ( 'NONE',  ( 0.000000000000000000, 0.000000000000000000, -1.000000000000000000 ) ) ;
#81768 = CARTESIAN_POINT ( 'NONE',  ( -115.5200949002220767, -23.85016227208580730, -0.8807180028928282001 ) ) ;
#81769 = CARTESIAN_POINT ( 'NONE',  ( -10.09097066620046235, 20.03973272787133553, 11.49999999999998934 ) ) ;
#81770 = CARTESIAN_POINT ( 'NONE',  ( -33.55620429048339304, -24.64965694238574656, 8.947790433994208925 ) ) ;
#81771 = CARTESIAN_POINT ( 'NONE',  ( -27.83739072329610664, 5.965225279485592225, -8.084349702057698650 ) ) ;
#81772 = ORIENTED_EDGE ( 'NONE', *, *, #64232, .T. ) ;
#81773 = DIRECTION ( 'NONE',  ( 0.9685340172660600322, 0.000000000000000000, -0.2488812114211667315 ) ) ;
#81774 = DIRECTION ( 'NONE',  ( 0.000000000000000000, -0.9999999999976377785, -2.173523156925979128E-06 ) ) ;
#81775 = AXIS2_PLACEMENT_3D ( 'NONE', #37408, #84066, #45027 ) ;
#81776 = ORIENTED_EDGE ( 'NONE', *, *, #29611, .T. ) ;
#81777 = ORIENTED_EDGE ( 'NONE', *, *, #61904, .T. ) ;
#81778 = FACE_OUTER_BOUND ( 'NONE', #74302, .T. ) ;
#81779 = EDGE_LOOP ( 'NONE', ( #31927, #84147, #94855, #93218 ) ) ;
#81780 = B_SPLINE_CURVE_WITH_KNOTS ( 'NONE', 3,
 ( #78647, #61956, #79165, #71574 ),
 .UNSPECIFIED., .F., .F.,
 ( 4, 4 ),
 ( 0.000000000000000000, 9.999999999998897304E-05 ),
 .UNSPECIFIED. ) ;
#81781 = B_SPLINE_CURVE_WITH_KNOTS ( 'NONE', 3,
 ( #87747, #1010, #24339, #85740, #31955, #71026 ),
 .UNSPECIFIED., .F., .F.,
 ( 4, 2, 4 ),
 ( 6.391158118970788496E-06, 0.001387004593080793302, 0.002767618028042615873 ),
 .UNSPECIFIED. ) ;
#81782 = CARTESIAN_POINT ( 'NONE',  ( -3.453506354162970915, -21.03206338698385736, -1.500000000000002220 ) ) ;
#81783 = ORIENTED_EDGE ( 'NONE', *, *, #53212, .F. ) ;
#81784 = CARTESIAN_POINT ( 'NONE',  ( -88.59478540386743362, -23.96119346886881019, -0.6495511937832099125 ) ) ;
#81785 = CARTESIAN_POINT ( 'NONE',  ( -5.042499505632127565, 21.24692939306837758, 11.49999999999998934 ) ) ;
#81786 = LINE ( 'NONE', #74175, #64388 ) ;
#81787 = CARTESIAN_POINT ( 'NONE',  ( 22.03932947713327906, 5.445304565557160359, 11.49999999999998934 ) ) ;
#81788 = CARTESIAN_POINT ( 'NONE',  ( -41.44993916608342488, -25.28892577674693598, 4.009750349030761107 ) ) ;
#81789 = CARTESIAN_POINT ( 'NONE',  ( -35.62287095715005592, -24.99132157543083821, 2.256160258750667502 ) ) ;
#81790 = CARTESIAN_POINT ( 'NONE',  ( 18.54397492014093984, 11.73900455106235086, -1.500000000000002220 ) ) ;
#81791 = CARTESIAN_POINT ( 'NONE',  ( 7.136624701378261548, -6.376774720514420736, 20.99078681144753844 ) ) ;
#81792 = ORIENTED_EDGE ( 'NONE', *, *, #40624, .F. ) ;
#81793 = CARTESIAN_POINT ( 'NONE',  ( -122.5545124863704416, -24.35071581493544102, 9.817618358456019934 ) ) ;
#81794 = CARTESIAN_POINT ( 'NONE',  ( -49.00533630786537032, -25.12782636286262417, 6.749866211151510420 ) ) ;
#81795 = ORIENTED_EDGE ( 'NONE', *, *, #92711, .T. ) ;
#81796 = CARTESIAN_POINT ( 'NONE',  ( -99.62287095715001328, -24.33927499327854704, 9.819080762295815390 ) ) ;
#81797 = ORIENTED_EDGE ( 'NONE', *, *, #34311, .T. ) ;
#81798 = LINE ( 'NONE', #81300, #75099 ) ;
#81799 = CARTESIAN_POINT ( 'NONE',  ( -0.02086824871851778590, -22.77984412121519142, 2.712351064733613537 ) ) ;
#81800 = CARTESIAN_POINT ( 'NONE',  ( 19.37530031839547107, -8.734557088507903799, -1.500000000000002220 ) ) ;
#81801 = CARTESIAN_POINT ( 'NONE',  ( -112.5952074097005209, -23.48783264082478794, -1.443836473390061492 ) ) ;
#81802 = CARTESIAN_POINT ( 'NONE',  ( -26.63407156546748311, -24.75186084215640037, 2.799621796061711798 ) ) ;
#81803 = VECTOR ( 'NONE', #61013, 1000.000000000000000 ) ;
#81804 = CARTESIAN_POINT ( 'NONE',  ( -85.49558519425330871, -25.00158670708911046, 2.256160236439219702 ) ) ;
#81805 = B_SPLINE_CURVE_WITH_KNOTS ( 'NONE', 3,
 ( #44708, #89878, #36093, #13737 ),
 .UNSPECIFIED., .F., .F.,
 ( 4, 4 ),
 ( 0.000000000000000000, 0.0001000000000000028644 ),
 .UNSPECIFIED. ) ;
#81806 = CARTESIAN_POINT ( 'NONE',  ( -84.62287095715004170, -24.51387760970723662, 9.387446482453407626 ) ) ;
#81807 = EDGE_CURVE ( 'NONE', #63342, #46359, #17914, .T. ) ;
#81808 = CARTESIAN_POINT ( 'NONE',  ( -117.5936860851973762, -23.48786465467241769, 11.44779295918253581 ) ) ;
#81809 = ORIENTED_EDGE ( 'NONE', *, *, #45791, .T. ) ;
#81810 = CARTESIAN_POINT ( 'NONE',  ( -9.542874777335924819, 17.09510996321218101, 11.49999999999999645 ) ) ;
#81811 = CARTESIAN_POINT ( 'NONE',  ( 13.57581083383196940, -6.376774720514426953, 20.21213203435597094 ) ) ;
#81812 = CARTESIAN_POINT ( 'NONE',  ( -79.37931354260665273, -25.24055654816928396, 6.260468804161273937 ) ) ;
#81813 = B_SPLINE_CURVE_WITH_KNOTS ( 'NONE', 3,
 ( #9104, #53411, #84336, #40063, #53910, #45790 ),
 .UNSPECIFIED., .F., .F.,
 ( 4, 2, 4 ),
 ( 0.000000000000000000, 0.001380764517854761930, 0.002761529035709523860 ),
 .UNSPECIFIED. ) ;
#81814 = ORIENTED_EDGE ( 'NONE', *, *, #34733, .F. ) ;
#81815 = AXIS2_PLACEMENT_3D ( 'NONE', #61928, #61432, #38074 ) ;
#81816 = CARTESIAN_POINT ( 'NONE',  ( 3.825380556292953482, -6.376774720514427841, 21.83927723428477208 ) ) ;
#81817 = CARTESIAN_POINT ( 'NONE',  ( -44.58953762381671027, -24.65952944569304250, 1.056160979905695463 ) ) ;
#81818 = CARTESIAN_POINT ( 'NONE',  ( -116.5562042904833930, -23.48783264082479150, -1.443836473390057940 ) ) ;
#81819 = B_SPLINE_CURVE_WITH_KNOTS ( 'NONE', 3,
 ( #20657, #65878, #20163, #88196 ),
 .UNSPECIFIED., .F., .F.,
 ( 4, 4 ),
 ( 0.000000000000000000, 1.000000000000000000 ),
 .UNSPECIFIED. ) ;
#81820 = CARTESIAN_POINT ( 'NONE',  ( -106.6228709571500559, -23.48783264082479150, -1.443836473390060382 ) ) ;
#81821 = CARTESIAN_POINT ( 'NONE',  ( 18.28535361393070957, 7.309334553982634652, -1.500000000000002220 ) ) ;
#81822 = ORIENTED_EDGE ( 'NONE', *, *, #12205, .T. ) ;
#81823 = CARTESIAN_POINT ( 'NONE',  ( 10.54812756816019892, 3.634129942730893070, -27.00766266717979747 ) ) ;
#81824 = CARTESIAN_POINT ( 'NONE',  ( -56.52287095715006870, -29.50250243563736774, 8.947779886222145151 ) ) ;
#81825 = ADVANCED_FACE ( 'NONE', ( #83170 ), #29893, .T. ) ;
#81826 = APPROVAL_ROLE ( '' ) ;
#81827 = ORIENTED_EDGE ( 'NONE', *, *, #75686, .T. ) ;
#81828 = CARTESIAN_POINT ( 'NONE',  ( -48.62287095715004881, -23.47593901973091235, -1.443836447539009749 ) ) ;
#81829 = CARTESIAN_POINT ( 'NONE',  ( -125.6228709571500559, -23.47593901973091235, -1.443836447538995760 ) ) ;
#81830 = CARTESIAN_POINT ( 'NONE',  ( -69.62287095715005592, -24.64898659630528854, 1.056161002820824368 ) ) ;
#81831 = CARTESIAN_POINT ( 'NONE',  ( -118.5523306988183521, -24.65952944569305316, 1.056160979905708119 ) ) ;
#81832 = CARTESIAN_POINT ( 'NONE',  ( -31.62287095715005236, -24.33927499327853639, 9.819080762295824272 ) ) ;
#81833 = EDGE_CURVE ( 'NONE', #62812, #71428, #19612, .T. ) ;
#81834 = CARTESIAN_POINT ( 'NONE',  ( 33.61456970919605425, -3.316774720514426900, -11.35828564741663449 ) ) ;
#81835 = CARTESIAN_POINT ( 'NONE',  ( -50.62287095715004170, -24.14321612903114556, -0.2833117244521691780 ) ) ;
#81836 = CARTESIAN_POINT ( 'NONE',  ( 19.59856454566043382, -3.714209461170434157, -1.500000000000002220 ) ) ;
#81837 = DIRECTION ( 'NONE',  ( 0.000000000000000000, 1.155373159085149695E-17, 1.000000000000000000 ) ) ;
#81838 = CARTESIAN_POINT ( 'NONE',  ( -0.06129594755597236877, -22.25647579004533583, 0.6535302041569640563 ) ) ;
#81839 = ORIENTED_EDGE ( 'NONE', *, *, #56467, .T. ) ;
#81840 = EDGE_CURVE ( 'NONE', #24865, #52488, #70484, .T. ) ;
#81841 = CARTESIAN_POINT ( 'NONE',  ( -112.6228709571500701, -23.48783264082479150, -1.443836473390060160 ) ) ;
#81842 = CARTESIAN_POINT ( 'NONE',  ( 4.453188626415028217, -5.876774720514421624, 21.07953283331298167 ) ) ;
#81843 = EDGE_CURVE ( 'NONE', #35617, #62726, #57211, .T. ) ;
#81844 = EDGE_CURVE ( 'NONE', #53767, #17423, #42641, .T. ) ;
#81845 = VECTOR ( 'NONE', #74224, 1000.000000000000114 ) ;
#81846 = CARTESIAN_POINT ( 'NONE',  ( 10.93823315965619791, -6.376774720514427841, -24.99764212866241309 ) ) ;
#81847 = CARTESIAN_POINT ( 'NONE',  ( -49.62287095715005592, -24.51387760970723662, 9.387446482453421837 ) ) ;
#81848 = CARTESIAN_POINT ( 'NONE',  ( -63.62287095715004881, -29.50248528299804818, 1.056150453629034924 ) ) ;
#81849 = CARTESIAN_POINT ( 'NONE',  ( -26.19271238903531085, -24.92001040704539250, 3.794289475298080028 ) ) ;
#81850 = CARTESIAN_POINT ( 'NONE',  ( -88.62287095715002749, -24.50216790748099527, 0.6166512839513722533 ) ) ;
#81851 = ORIENTED_EDGE ( 'NONE', *, *, #57124, .T. ) ;
#81852 = PLANE ( 'NONE',  #47883 ) ;
#81853 = CARTESIAN_POINT ( 'NONE',  ( -46.52287095715007581, -23.47593901973090524, -1.443836447538997314 ) ) ;
#81854 = ORIENTED_EDGE ( 'NONE', *, *, #37639, .F. ) ;
#81855 = B_SPLINE_CURVE_WITH_KNOTS ( 'NONE', 3,
 ( #62023, #76712, #9220, #41702, #41190, #72645, #94464, #24945 ),
 .UNSPECIFIED., .F., .F.,
 ( 4, 2, 2, 4 ),
 ( -0.001224873891641419139, -0.0002244903592271050262, 0.0007758931731872090870, 0.002776660238015837313 ),
 .UNSPECIFIED. ) ;
#81856 = CARTESIAN_POINT ( 'NONE',  ( 2.165584020960389822, 20.11889322763239107, -1.500000000000002220 ) ) ;
#81857 = EDGE_CURVE ( 'NONE', #70350, #15460, #8200, .T. ) ;
#81858 = LINE ( 'NONE', #4739, #63052 ) ;
#81859 = LINE ( 'NONE', #11839, #46393 ) ;
#81860 = DIRECTION ( 'NONE',  ( 0.000000000000000000, 0.000000000000000000, 1.000000000000000000 ) ) ;
#81861 = ORIENTED_EDGE ( 'NONE', *, *, #29975, .F. ) ;
#81862 = CARTESIAN_POINT ( 'NONE',  ( -79.76923701135288525, -25.31526207978247811, 5.130284102396473145 ) ) ;
#81863 = LINE ( 'NONE', #6227, #53551 ) ;
#81864 = CARTESIAN_POINT ( 'NONE',  ( -0.1815635828756200498, -20.05798930676971636, -1.500000000000002220 ) ) ;
#81865 = CARTESIAN_POINT ( 'NONE',  ( 2.184583272949580213, -20.89682302726931340, 11.49999999999999645 ) ) ;
#81866 = DIRECTION ( 'NONE',  ( -1.000000000000000000, 0.000000000000000000, 0.000000000000000000 ) ) ;
#81867 = DIRECTION ( 'NONE',  ( -0.000000000000000000, -0.000000000000000000, -1.000000000000000000 ) ) ;
#81868 = CARTESIAN_POINT ( 'NONE',  ( -19.11006845027251799, 11.06304553819242642, 11.49999999999998934 ) ) ;
#81869 = EDGE_CURVE ( 'NONE', #50913, #58306, #64378, .T. ) ;
#81870 = CARTESIAN_POINT ( 'NONE',  ( -53.58953762381671737, -24.64965694238574656, 8.947790433994201820 ) ) ;
#81871 = CARTESIAN_POINT ( 'NONE',  ( -107.6228709571500701, -24.64965695001469115, 8.947790433994176951 ) ) ;
#81872 = CARTESIAN_POINT ( 'NONE',  ( -50.10737344585005815, -25.18440108260957899, 3.323112688921421753 ) ) ;
#81873 = VERTEX_POINT ( 'NONE', #79061 ) ;
#81874 = EDGE_CURVE ( 'NONE', #41093, #71061, #39025, .T. ) ;
#81875 = CARTESIAN_POINT ( 'NONE',  ( -35.52287095715007581, -24.63345952396254290, 9.038047939301508293 ) ) ;
#81876 = CARTESIAN_POINT ( 'NONE',  ( -38.52287095715006870, -29.50250786944525672, 11.44777988621624232 ) ) ;
#81877 = ORIENTED_EDGE ( 'NONE', *, *, #57607, .T. ) ;
#81878 = ORIENTED_EDGE ( 'NONE', *, *, #32391, .T. ) ;
#81879 = CARTESIAN_POINT ( 'NONE',  ( -42.62287095715006302, -23.47596703998600276, 11.44779298504227505 ) ) ;
#81880 = DIRECTION ( 'NONE',  ( -0.000000000000000000, 1.000000000000000000, -0.000000000000000000 ) ) ;
#81881 = CARTESIAN_POINT ( 'NONE',  ( -91.62287095715004170, -24.65952944569304606, 1.056160979905700792 ) ) ;
#81882 = CARTESIAN_POINT ( 'NONE',  ( 6.226698476505521995, -19.64469265145860177, -1.500000000000002220 ) ) ;
#81883 = ADVANCED_FACE ( 'NONE', ( #95297 ), #49143, .F. ) ;
#81884 = CARTESIAN_POINT ( 'NONE',  ( 8.792760106793807040, 19.66521392739144858, 11.49999999999999645 ) ) ;
#81885 = ORIENTED_EDGE ( 'NONE', *, *, #57736, .F. ) ;
#81886 = CARTESIAN_POINT ( 'NONE',  ( 15.29947330337542688, -3.316774720514426456, -27.16854002387010070 ) ) ;
#81887 = LINE ( 'NONE', #59062, #14200 ) ;
#81888 = DIRECTION ( 'NONE',  ( 1.000000000000000000, 0.000000000000000000, -2.216313064514630605E-15 ) ) ;
#81889 = CARTESIAN_POINT ( 'NONE',  ( 13.91197278145025074, 17.48688927191260234, 11.49999999999998934 ) ) ;
#81890 = AXIS2_PLACEMENT_3D ( 'NONE', #9357, #40318, #38807 ) ;
#81891 = EDGE_CURVE ( 'NONE', #47172, #83063, #70463, .T. ) ;
#81892 = DIRECTION ( 'NONE',  ( -0.7512896232466861335, 0.000000000000000000, -0.6599726524651249315 ) ) ;
#81893 = DIRECTION ( 'NONE',  ( 0.000000000000000000, -2.173523156925980399E-06, 0.9999999999976378895 ) ) ;
#81894 = ORIENTED_EDGE ( 'NONE', *, *, #83832, .T. ) ;
#81895 = ADVANCED_FACE ( 'NONE', ( #55252 ), #63373, .T. ) ;
#81896 = DIRECTION ( 'NONE',  ( -1.000000000000000000, 0.000000000000000000, -0.000000000000000000 ) ) ;
#81897 = CARTESIAN_POINT ( 'NONE',  ( 31.35973677934181936, 4.378374783736292741, 0.3342810658314839256 ) ) ;
#81898 = CARTESIAN_POINT ( 'NONE',  ( 11.28189403632909915, 17.58240144430209995, 11.49999999999998934 ) ) ;
#81899 = ORIENTED_EDGE ( 'NONE', *, *, #28939, .T. ) ;
#81901 = VERTEX_POINT ( 'NONE', #71472 ) ;
#81900 = FACE_OUTER_BOUND ( 'NONE', #68777, .T. ) ;
#81902 = ORIENTED_EDGE ( 'NONE', *, *, #61904, .F. ) ;
#81903 = CARTESIAN_POINT ( 'NONE',  ( -100.5937251445320157, -24.15602025860896518, 10.28564288303536856 ) ) ;
#81904 = CARTESIAN_POINT ( 'NONE',  ( -21.11812214938331422, 0.5215410354952813021, -1.500000000000002220 ) ) ;
#81905 = ORIENTED_EDGE ( 'NONE', *, *, #49, .F. ) ;
#81906 = CARTESIAN_POINT ( 'NONE',  ( -37.55620429048340014, -23.47596703998600276, 11.44779298504227505 ) ) ;
#81907 = CARTESIAN_POINT ( 'NONE',  ( 6.424528460793287543, -5.876774720514413630, 19.73230822599986212 ) ) ;
#81908 = CARTESIAN_POINT ( 'NONE',  ( -48.62287095715006302, -23.96177878511307568, 10.65340807706330217 ) ) ;
#81909 = FACE_OUTER_BOUND ( 'NONE', #1047, .T. ) ;
#81910 = CARTESIAN_POINT ( 'NONE',  ( -49.28237063580810684, -25.19919229018893247, 3.391011315159921047 ) ) ;
#81911 = CARTESIAN_POINT ( 'NONE',  ( -3.653784360050144286, 21.42803128968991544, -1.500000000000002220 ) ) ;
#81912 = CARTESIAN_POINT ( 'NONE',  ( -81.35928118207723969, -25.24759704261755289, 6.638486653501257884 ) ) ;
#81914 = ORIENTED_EDGE ( 'NONE', *, *, #22920, .F. ) ;
#81913 = CARTESIAN_POINT ( 'NONE',  ( -7.359855604737914447, 20.98419016808480109, 11.49999999999999645 ) ) ;
#81915 = CARTESIAN_POINT ( 'NONE',  ( -51.50851365739161736, -25.24728896969645220, 5.995695872060372800 ) ) ;
#81916 = DIRECTION ( 'NONE',  ( 0.000000000000000000, 0.000000000000000000, -1.000000000000000000 ) ) ;
#81917 = FACE_OUTER_BOUND ( 'NONE', #91880, .T. ) ;
#81918 = ORIENTED_EDGE ( 'NONE', *, *, #57005, .T. ) ;
#81920 = ORIENTED_EDGE ( 'NONE', *, *, #35907, .T. ) ;
#81919 = CARTESIAN_POINT ( 'NONE',  ( -104.9228709571500673, -23.47596703998600631, 11.44779298504227860 ) ) ;
#81921 = ORIENTED_EDGE ( 'NONE', *, *, #76019, .F. ) ;
#81922 = CIRCLE ( 'NONE', #31725, 3.549999999999999378 ) ;
#81923 = CARTESIAN_POINT ( 'NONE',  ( -75.52287095715007581, -24.15431212366391023, -0.2830839119429213735 ) ) ;
#81924 = CARTESIAN_POINT ( 'NONE',  ( 11.16000000000000014, -9.652339641703484574, 1.628518864987183790 ) ) ;
#81925 = CARTESIAN_POINT ( 'NONE',  ( -32.99388727629348494, -29.50248914092071928, 2.831113219569932227 ) ) ;
#81926 = CARTESIAN_POINT ( 'NONE',  ( -48.62287095715008434, -23.96127896941632329, -0.6493128931037863705 ) ) ;
#81927 = FACE_OUTER_BOUND ( 'NONE', #49551, .T. ) ;
#81928 = ORIENTED_EDGE ( 'NONE', *, *, #81505, .F. ) ;
#81929 = CARTESIAN_POINT ( 'NONE',  ( 8.513215801882951794, -17.43586836189350819, 11.49999999999999645 ) ) ;
#81930 = CARTESIAN_POINT ( 'NONE',  ( 0.7051282051282027341, -6.376774720514408301, 19.19230769230768985 ) ) ;
#81931 = CARTESIAN_POINT ( 'NONE',  ( -15.54266751046811557, -16.22994250641250957, -1.500000000000002220 ) ) ;
#81932 = ORIENTED_EDGE ( 'NONE', *, *, #98102, .T. ) ;
#81933 = CARTESIAN_POINT ( 'NONE',  ( -101.6235504712075226, -24.66019654487200086, 8.947790411086115725 ) ) ;
#81934 = CARTESIAN_POINT ( 'NONE',  ( 5.865642684142210683, 5.356774720514426491, -25.36740469599890702 ) ) ;
#81935 = DIRECTION ( 'NONE',  ( -0.9496245541219268116, 6.454799914155188842E-16, -0.3133898629642187239 ) ) ;
#81936 = CARTESIAN_POINT ( 'NONE',  ( -63.91063125405472789, -25.14081846633246897, 7.291654623549837844 ) ) ;
#81937 = CARTESIAN_POINT ( 'NONE',  ( 19.11985901488480621, -4.296470200863222288, 11.49999999999998934 ) ) ;
#81938 = CARTESIAN_POINT ( 'NONE',  ( -119.9228709571500531, -23.47596703998600631, 11.44779298504227860 ) ) ;
#81939 = ORIENTED_EDGE ( 'NONE', *, *, #26109, .T. ) ;
#81940 = CARTESIAN_POINT ( 'NONE',  ( -21.45671390985790694, -1.711987587955616119, 11.49999999999998934 ) ) ;
#81941 = CARTESIAN_POINT ( 'NONE',  ( -125.5228709571500616, -24.99132157543084531, 2.256160258750667502 ) ) ;
#81942 = DIRECTION ( 'NONE',  ( -1.000000000000000000, 0.000000000000000000, 0.000000000000000000 ) ) ;
#81943 = CARTESIAN_POINT ( 'NONE',  ( -100.5228709571500616, -29.50247984919015209, -1.443849546365050029 ) ) ;
#81944 = CARTESIAN_POINT ( 'NONE',  ( -99.78454658038423020, -25.27473267031680493, 3.502964407505847699 ) ) ;
#81945 = CARTESIAN_POINT ( 'NONE',  ( -7.281717392095591102, 21.80608952751712692, -1.500000000000002220 ) ) ;
#81946 = VECTOR ( 'NONE', #15334, 1000.000000000000114 ) ;
#81947 = EDGE_CURVE ( 'NONE', #67714, #85130, #16664, .T. ) ;
#81948 = DATE_TIME_ROLE ( 'classification_date' ) ;
#81949 = FACE_OUTER_BOUND ( 'NONE', #57354, .T. ) ;
#81950 = DIRECTION ( 'NONE',  ( -0.7512896232465888779, 8.688531644690855961E-16, -0.6599726524652355097 ) ) ;
#81951 = CARTESIAN_POINT ( 'NONE',  ( -17.93149374516376682, -9.230432107326475233, 11.49999999999999645 ) ) ;
#81952 = CARTESIAN_POINT ( 'NONE',  ( -108.9756736452620771, -25.10927630203814331, 3.908685950094584083 ) ) ;
#81953 = CARTESIAN_POINT ( 'NONE',  ( -32.65034022602505104, -23.96169478059712787, 10.65365249895719124 ) ) ;
#81954 = VECTOR ( 'NONE', #44237, 1000.000000000000114 ) ;
#81956 = CARTESIAN_POINT ( 'NONE',  ( -4.968349358974361252, -5.876774720514412742, 19.46153846153847056 ) ) ;
#81955 = TOROIDAL_SURFACE ( 'NONE', #57866, 3.060000000000000053, 3.060000000000000053 ) ;
#81957 = CARTESIAN_POINT ( 'NONE',  ( 14.78484767477523576, 3.316774720514427344, -28.43034250232788551 ) ) ;
#81958 = B_SPLINE_CURVE_WITH_KNOTS ( 'NONE', 3,
 ( #82345, #38156, #69109, #74723, #5225, #36181 ),
 .UNSPECIFIED., .F., .F.,
 ( 4, 2, 4 ),
 ( 0.000000000000000000, 0.001380901958385381606, 0.002761803916770763211 ),
 .UNSPECIFIED. ) ;
#81959 = CARTESIAN_POINT ( 'NONE',  ( -126.5895376238167245, -23.48786465467242124, 11.44779295918253403 ) ) ;
#81960 = CARTESIAN_POINT ( 'NONE',  ( -13.56193660873917395, -14.51407242162769151, 11.49999999999998934 ) ) ;
#81961 = CIRCLE ( 'NONE', #68991, 1.399999999999999911 ) ;
#81963 = EDGE_CURVE ( 'NONE', #98627, #13349, #77851, .T. ) ;
#81962 = CARTESIAN_POINT ( 'NONE',  ( -47.62287095715004881, -24.66019654487199020, 8.947790411086133489 ) ) ;
#81964 = CARTESIAN_POINT ( 'NONE',  ( -10.60818629614422370, 16.63341085705455669, -1.500000000000002220 ) ) ;
#81965 = ADVANCED_FACE ( 'NONE', ( #78551 ), #9056, .F. ) ;
#81966 = AXIS2_PLACEMENT_3D ( 'NONE', #96978, #90363, #29454 ) ;
#81967 = DIRECTION ( 'NONE',  ( -3.773278334453079030E-23, 0.9999999999976377785, 2.173523156925979128E-06 ) ) ;
#81968 = ADVANCED_FACE ( 'NONE', ( #80070 ), #69375, .T. ) ;
#81969 = EDGE_CURVE ( 'NONE', #9400, #1176, #34398, .T. ) ;
#81970 = CARTESIAN_POINT ( 'NONE',  ( -1.044639546681034536, -6.376774720514417183, 20.34213149456667580 ) ) ;
#81971 = CARTESIAN_POINT ( 'NONE',  ( -48.62287095715004881, -23.48786465467241058, 11.44779295918254824 ) ) ;
#81972 = CARTESIAN_POINT ( 'NONE',  ( -15.36756058500021282, 13.76162614515376426, 11.49999999999999645 ) ) ;
#81973 = CARTESIAN_POINT ( 'NONE',  ( -113.6228709571500559, -23.47593901973091235, -1.443836447538999312 ) ) ;
#81974 = CARTESIAN_POINT ( 'NONE',  ( 31.62034159138974232, 4.397688677369781196, -2.670054032269984834 ) ) ;
#81975 = CARTESIAN_POINT ( 'NONE',  ( -18.74212433040710479, 12.77821124017617649, 11.49999999999999645 ) ) ;
#81976 = ORIENTED_EDGE ( 'NONE', *, *, #80151, .F. ) ;
#81977 = CARTESIAN_POINT ( 'NONE',  ( 3.106028565906091998, -5.876774720514426953, 3.106028565906120864 ) ) ;
#81978 = CARTESIAN_POINT ( 'NONE',  ( 29.73620800866979863, 5.101103159685075106, 27.18593991345460381 ) ) ;
#81979 = ADVANCED_FACE ( 'NONE', ( #33895 ), #64881, .T. ) ;
#81980 = DIRECTION ( 'NONE',  ( 0.000000000000000000, 0.000000000000000000, -1.000000000000000000 ) ) ;
#81981 = CARTESIAN_POINT ( 'NONE',  ( -45.62287095715004881, -25.00158670708908915, 2.256160236439166855 ) ) ;
#81982 = ORIENTED_EDGE ( 'NONE', *, *, #98851, .F. ) ;
#81983 = ORIENTED_EDGE ( 'NONE', *, *, #94816, .F. ) ;
#81984 = EDGE_CURVE ( 'NONE', #30953, #48655, #19496, .T. ) ;
#81985 = CARTESIAN_POINT ( 'NONE',  ( -99.61095392075885968, -25.16913655607350009, 6.819335884888137578 ) ) ;
#81986 = CARTESIAN_POINT ( 'NONE',  ( 20.41593879258296695, -10.28030303932802880, -1.500000000000002220 ) ) ;
#81987 = CARTESIAN_POINT ( 'NONE',  ( -74.62287095715008434, -23.96127896941632685, -0.6493128931037843721 ) ) ;
#81988 = CARTESIAN_POINT ( 'NONE',  ( -21.01953065494444317, -4.859126342152997324, -1.500000000000002220 ) ) ;
#81989 = CARTESIAN_POINT ( 'NONE',  ( -113.5881221940176005, -24.51419770103157347, 9.386484678747168076 ) ) ;
#81990 = CARTESIAN_POINT ( 'NONE',  ( -89.81226385320383088, -25.05712135967894838, 7.447789548357302891 ) ) ;
#81991 = CARTESIAN_POINT ( 'NONE',  ( 18.83488669200175281, -12.41447709603701632, 11.49999999999999645 ) ) ;
#81992 = ORIENTED_EDGE ( 'NONE', *, *, #24748, .T. ) ;
#81993 = CARTESIAN_POINT ( 'NONE',  ( -70.22848692110255797, -25.24754246103700694, 4.852864574778647189 ) ) ;
#81994 = B_SPLINE_CURVE_WITH_KNOTS ( 'NONE', 3,
 ( #13462, #66287, #5860, #50542, #5364, #36318, #42449, #67278 ),
 .UNSPECIFIED., .F., .F.,
 ( 4, 2, 2, 4 ),
 ( 6.384118678609026632E-06, 0.002007151183507258855, 0.003007534715921582075, 0.004007918248335905730 ),
 .UNSPECIFIED. ) ;
#81995 = CARTESIAN_POINT ( 'NONE',  ( -13.73438224071023761, 17.16576579689093762, -1.500000000000002220 ) ) ;
#81996 = EDGE_CURVE ( 'NONE', #60911, #49715, #78993, .T. ) ;
#81997 = CARTESIAN_POINT ( 'NONE',  ( -44.50616043664086163, -23.96169478059713143, 10.65365249895718414 ) ) ;
#81998 = CARTESIAN_POINT ( 'NONE',  ( 27.86270917940689174, 5.965225279485572685, 29.49402280011862487 ) ) ;
#81999 = ORIENTED_EDGE ( 'NONE', *, *, #35807, .T. ) ;
#82000 = LINE ( 'NONE', #97719, #13577 ) ;
#82001 = CARTESIAN_POINT ( 'NONE',  ( -0.4909855769230799249, -6.376774720514410077, 19.14743589743590491 ) ) ;
#82002 = ORIENTED_EDGE ( 'NONE', *, *, #65073, .F. ) ;
#82003 = CARTESIAN_POINT ( 'NONE',  ( 12.92500000000000426, 1.999999999999999556, 18.24068255301867936 ) ) ;
#82004 = VERTEX_POINT ( 'NONE', #88190 ) ;
#82005 = ORIENTED_EDGE ( 'NONE', *, *, #82760, .F. ) ;
#82006 = ORIENTED_EDGE ( 'NONE', *, *, #16327, .F. ) ;
#82007 = CARTESIAN_POINT ( 'NONE',  ( -110.6228709571500843, -23.47596703998600631, 11.44779298504227860 ) ) ;
#82008 = CARTESIAN_POINT ( 'NONE',  ( -104.5228709571501327, -23.96127896941634106, -0.6493128931037958074 ) ) ;
#82009 = CARTESIAN_POINT ( 'NONE',  ( -57.48876574585108301, -24.65952944569304606, 1.056160979905698571 ) ) ;
#82010 = CARTESIAN_POINT ( 'NONE',  ( 18.82465703714932204, -7.861812626244089053, -1.500000000000002220 ) ) ;
#82011 = EDGE_LOOP ( 'NONE', ( #73100, #31862, #54206, #83841 ) ) ;
#82012 = DIRECTION ( 'NONE',  ( 0.000000000000000000, 0.9999999999976377785, 2.173523156925979128E-06 ) ) ;
#82013 = CARTESIAN_POINT ( 'NONE',  ( -27.96875734969026084, 6.475225279485573360, -0.08597719988137648983 ) ) ;
#82014 = EDGE_CURVE ( 'NONE', #82863, #17858, #76192, .T. ) ;
#82015 = CARTESIAN_POINT ( 'NONE',  ( -5.891025641025639636, -5.876774720514419847, 20.75510817307693046 ) ) ;
#82016 = CARTESIAN_POINT ( 'NONE',  ( -35.58953762381672448, -23.47593901973091235, -1.443836447539011525 ) ) ;
#82017 = VERTEX_POINT ( 'NONE', #28274 ) ;
#82018 = CARTESIAN_POINT ( 'NONE',  ( 13.10664265030973930, 0.3587747205144256601, -27.62597719988137612 ) ) ;
#82019 = CARTESIAN_POINT ( 'NONE',  ( -33.62287095715005592, -24.65952944569304250, 1.056160979905690356 ) ) ;
#82020 = ORIENTED_EDGE ( 'NONE', *, *, #36031, .T. ) ;
#82021 = CARTESIAN_POINT ( 'NONE',  ( 8.872108392497455753, -18.76566404461018678, 11.49999999999998934 ) ) ;
#82022 = EDGE_CURVE ( 'NONE', #85000, #41774, #26783, .T. ) ;
#82023 = VERTEX_POINT ( 'NONE', #3954 ) ;
#82025 = EDGE_LOOP ( 'NONE', ( #77886, #59493, #91356, #14017 ) ) ;
#82024 = DIRECTION ( 'NONE',  ( 0.000000000000000000, 0.000000000000000000, 1.000000000000000000 ) ) ;
#82026 = VECTOR ( 'NONE', #22680, 1000.000000000000000 ) ;
#82027 = FACE_OUTER_BOUND ( 'NONE', #57896, .T. ) ;
#82028 = DIRECTION ( 'NONE',  ( -0.7512896232465892110, 0.000000000000000000, -0.6599726524652350657 ) ) ;
#82029 = ORIENTED_EDGE ( 'NONE', *, *, #19522, .T. ) ;
#82030 = EDGE_LOOP ( 'NONE', ( #15050, #82514, #34008, #8969 ) ) ;
#82031 = AXIS2_PLACEMENT_3D ( 'NONE', #87002, #86502, #40828 ) ;
#82032 = CARTESIAN_POINT ( 'NONE',  ( -79.55620429048339304, -24.65952944569304961, 1.056160979905700348 ) ) ;
#82033 = DIRECTION ( 'NONE',  ( 0.000000000000000000, -2.173523156925980399E-06, 0.9999999999976378895 ) ) ;
#82034 = AXIS2_PLACEMENT_3D ( 'NONE', #75200, #45758, #38132 ) ;
#82035 = CARTESIAN_POINT ( 'NONE',  ( -4.620655831143558601, -5.876774720514410966, 19.21747685089457036 ) ) ;
#82036 = CARTESIAN_POINT ( 'NONE',  ( -71.29000553066028090, -25.31201746252870421, 6.029836970080467040 ) ) ;
#82038 = ORIENTED_EDGE ( 'NONE', *, *, #5458, .F. ) ;
#82037 = CARTESIAN_POINT ( 'NONE',  ( 1.153593019990587942, -22.03401787307112869, 11.49999999999999645 ) ) ;
#82039 = AXIS2_PLACEMENT_3D ( 'NONE', #84295, #14781, #7681 ) ;
#82040 = DIRECTION ( 'NONE',  ( 0.000000000000000000, -2.173523156925979552E-06, 0.9999999999976378895 ) ) ;
#82041 = CARTESIAN_POINT ( 'NONE',  ( -21.41681981171885951, -7.298096547245328303, -1.500000000000002220 ) ) ;
#82042 = VECTOR ( 'NONE', #91694, 1000.000000000000000 ) ;
#82044 = ORIENTED_EDGE ( 'NONE', *, *, #26200, .T. ) ;
#82043 = CARTESIAN_POINT ( 'NONE',  ( -115.6270093773762397, -24.40133493613050675, 9.663955038902797057 ) ) ;
#82045 = ORIENTED_EDGE ( 'NONE', *, *, #12443, .F. ) ;
#82046 = CARTESIAN_POINT ( 'NONE',  ( -78.62287095715007013, -24.66019654487199375, 8.947790411086124607 ) ) ;
#82047 = CARTESIAN_POINT ( 'NONE',  ( -57.55991801598921853, -23.73791477778911840, 11.05961554403170588 ) ) ;
#82048 = ORIENTED_EDGE ( 'NONE', *, *, #4640, .T. ) ;
#82049 = CARTESIAN_POINT ( 'NONE',  ( -20.37118330240554087, -5.769015352940915164, -1.500000000000002220 ) ) ;
#82050 = B_SPLINE_CURVE_WITH_KNOTS ( 'NONE', 3,
 ( #83833, #100032, #51902, #14808, #84324, #21419 ),
 .UNSPECIFIED., .F., .F.,
 ( 4, 2, 4 ),
 ( 6.384118678609746610E-06, 0.001386860460828373250, 0.002767336802978136688 ),
 .UNSPECIFIED. ) ;
#82051 = CARTESIAN_POINT ( 'NONE',  ( -103.5895376238167245, -24.64965694238575011, 8.947790433994194714 ) ) ;
#82052 = CARTESIAN_POINT ( 'NONE',  ( 0.6114060112162268412, -22.25658958135186793, -1.500000000000002220 ) ) ;
#82053 = B_SPLINE_CURVE_WITH_KNOTS ( 'NONE', 3,
 ( #37240, #38724, #46344, #83401 ),
 .UNSPECIFIED., .F., .F.,
 ( 4, 4 ),
 ( 0.6009291087672576914, 0.6099355400393732252 ),
 .UNSPECIFIED. ) ;
#82054 = CARTESIAN_POINT ( 'NONE',  ( -46.62287095715006302, -23.94994826722515313, -0.6494450866351717533 ) ) ;
#82055 = VERTEX_POINT ( 'NONE', #43016 ) ;
#82056 = CARTESIAN_POINT ( 'NONE',  ( -74.52287095715007581, -23.47596703998600631, 11.44779298504228748 ) ) ;
#82057 = CARTESIAN_POINT ( 'NONE',  ( 31.27206728860909024, 4.132774720514318822, -3.930752063305056332 ) ) ;
#82058 = VECTOR ( 'NONE', #66008, 1000.000000000000114 ) ;
#82059 = DIRECTION ( 'NONE',  ( -3.773278334453079030E-23, 0.9999999999976377785, 2.173523156925979128E-06 ) ) ;
#82060 = CARTESIAN_POINT ( 'NONE',  ( -116.5562042904834072, -24.64898659630528854, 1.056161002820835249 ) ) ;
#82061 = CARTESIAN_POINT ( 'NONE',  ( 9.662506626059768067, -16.94115208737379774, 11.49999999999998934 ) ) ;
#82062 = CARTESIAN_POINT ( 'NONE',  ( 18.29419249859179786, 11.19154738541161365, -1.500000000000002220 ) ) ;
#82063 = CARTESIAN_POINT ( 'NONE',  ( -26.72449842520168062, -24.92774724699053124, 1.897193310600636007 ) ) ;
#82064 = FACE_OUTER_BOUND ( 'NONE', #66940, .T. ) ;
#82065 = DIRECTION ( 'NONE',  ( 1.000000000000000000, 3.773278334444167608E-23, 8.201307833595939069E-29 ) ) ;
#82066 = CARTESIAN_POINT ( 'NONE',  ( -0.9063223138645676302, -22.79912562917415997, -1.500000000000002220 ) ) ;
#82067 = COORDINATED_UNIVERSAL_TIME_OFFSET ( 0, 0, .AHEAD. ) ;
#82068 = CARTESIAN_POINT ( 'NONE',  ( -106.5926167309080768, -23.96169478059714564, 10.65365249895717170 ) ) ;
#82069 = LINE ( 'NONE', #42031, #68674 ) ;
#82070 = CARTESIAN_POINT ( 'NONE',  ( 19.87125486832220744, 0.9792442318621276121, 11.49999999999999645 ) ) ;
#82071 = CARTESIAN_POINT ( 'NONE',  ( -104.6286256937127206, -24.15543982623907482, -0.2315651400026580709 ) ) ;
#82072 = EDGE_CURVE ( 'NONE', #68025, #78274, #87354, .T. ) ;
#82073 = B_SPLINE_CURVE_WITH_KNOTS ( 'NONE', 3,
 ( #7599, #77100, #47176, #87222 ),
 .UNSPECIFIED., .F., .F.,
 ( 4, 4 ),
 ( 0.000000000000000000, 9.999999999998897304E-05 ),
 .UNSPECIFIED. ) ;
#82074 = EDGE_CURVE ( 'NONE', #20580, #12021, #4943, .T. ) ;
#82075 = CARTESIAN_POINT ( 'NONE',  ( -0.6401674778748456252, 0.5172663018436739479, -2.677392948487098267E-15 ) ) ;
#82076 = DIRECTION ( 'NONE',  ( -1.000000000000000000, -0.000000000000000000, -0.000000000000000000 ) ) ;
#82077 = VERTEX_POINT ( 'NONE', #20651 ) ;
#82078 = CARTESIAN_POINT ( 'NONE',  ( -25.67538399529471249, -24.84156714063196958, 3.473377010405353182 ) ) ;
#82079 = CARTESIAN_POINT ( 'NONE',  ( -7.999999999999996447, -6.376774720514426953, 22.50000000000000355 ) ) ;
#82080 = EDGE_CURVE ( 'NONE', #38937, #80860, #58242, .T. ) ;
#82081 = CARTESIAN_POINT ( 'NONE',  ( -13.51661872714272405, -17.00040112538478709, 11.49999999999998934 ) ) ;
#82082 = DIRECTION ( 'NONE',  ( 0.000000000000000000, 0.000000000000000000, 1.000000000000000000 ) ) ;
#82083 = CARTESIAN_POINT ( 'NONE',  ( -13.79594968651775666, -13.80015156857029268, -1.500000000000002220 ) ) ;
#82084 = ADVANCED_FACE ( 'NONE', ( #4455 ), #19656, .F. ) ;
#82085 = VECTOR ( 'NONE', #86315, 1000.000000000000000 ) ;
#82086 = LINE ( 'NONE', #59760, #65309 ) ;
#82087 = EDGE_LOOP ( 'NONE', ( #42979, #91737, #87724, #8961 ) ) ;
#82088 = DATE_TIME_ROLE ( 'classification_date' ) ;
#82089 = CARTESIAN_POINT ( 'NONE',  ( 12.16765770914787304, -6.475225279485573360, -27.57618308014988173 ) ) ;
#82090 = CARTESIAN_POINT ( 'NONE',  ( -15.03541999946025243, -13.88573836563254460, 11.49999999999999645 ) ) ;
#82091 = CARTESIAN_POINT ( 'NONE',  ( 5.885012508251304730, -6.475225279485574248, -27.43431635654696521 ) ) ;
#82092 = AXIS2_PLACEMENT_3D ( 'NONE', #73129, #65537, #64542 ) ;
#82093 = CARTESIAN_POINT ( 'NONE',  ( -86.62287095715004170, -24.64965695001468404, 8.947790433994180503 ) ) ;
#82094 = ADVANCED_FACE ( 'NONE', ( #35889 ), #65872, .T. ) ;
#82095 = EDGE_LOOP ( 'NONE', ( #5991, #81252, #83414, #11654, #87993, #75722, #13869, #16454, #98695, #81046, #70927, #52669, #58313, #57314 ) ) ;
#82096 = CARTESIAN_POINT ( 'NONE',  ( -28.62287095715004881, -24.49675894734168580, 8.947790415257339092 ) ) ;
#82097 = CARTESIAN_POINT ( 'NONE',  ( 10.86264265030973952, -5.965225279485574461, -28.64597719988137570 ) ) ;
#82098 = AXIS2_PLACEMENT_3D ( 'NONE', #90623, #100200, #52071 ) ;
#82099 = DIRECTION ( 'NONE',  ( -3.773278334453079030E-23, 0.9999999999976377785, 2.173523156925979128E-06 ) ) ;
#82100 = VECTOR ( 'NONE', #56573, 1000.000000000000114 ) ;
#82101 = DIRECTION ( 'NONE',  ( 0.000000000000000000, 0.000000000000000000, 1.000000000000000000 ) ) ;
#82102 = ORIENTED_EDGE ( 'NONE', *, *, #4947, .F. ) ;
#82103 = CARTESIAN_POINT ( 'NONE',  ( 6.404294203292168142, -6.376774720514415407, 20.09052689972686423 ) ) ;
#82104 = VECTOR ( 'NONE', #2687, 1000.000000000000000 ) ;
#82105 = CARTESIAN_POINT ( 'NONE',  ( -23.02147672596084149, 0.6323230698326208765, 11.49999999999999645 ) ) ;
#82106 = CARTESIAN_POINT ( 'NONE',  ( -9.359374538088376383, 20.77767741201286711, 11.49999999999998934 ) ) ;
#82107 = CARTESIAN_POINT ( 'NONE',  ( -110.6300949696500453, -24.15602025860899360, 10.28564288303534724 ) ) ;
#82108 = DIRECTION ( 'NONE',  ( 0.000000000000000000, 0.000000000000000000, 1.000000000000000000 ) ) ;
#82109 = PLANE ( 'NONE',  #9562 ) ;
#82110 = FACE_OUTER_BOUND ( 'NONE', #85034, .T. ) ;
#82111 = CARTESIAN_POINT ( 'NONE',  ( -110.5150772214216914, -24.40034930558991633, 0.3402023900116072364 ) ) ;
#82112 = CARTESIAN_POINT ( 'NONE',  ( 1.548332177993611225, -21.85883989728069565, -1.500000000000002220 ) ) ;
#82113 = CARTESIAN_POINT ( 'NONE',  ( -46.62287095715004881, -29.50250243563736774, 8.947779886222146928 ) ) ;
#82114 = DIRECTION ( 'NONE',  ( 0.000000000000000000, -2.173523156925980399E-06, 0.9999999999976378895 ) ) ;
#82115 = DIRECTION ( 'NONE',  ( -0.5630016722799275897, 0.000000000000000000, 0.8264557562326038109 ) ) ;
#82116 = CARTESIAN_POINT ( 'NONE',  ( 20.57455539870835537, 2.682774720514426559, -18.22080502500613974 ) ) ;
#82117 = ORIENTED_EDGE ( 'NONE', *, *, #31383, .T. ) ;
#82118 = CARTESIAN_POINT ( 'NONE',  ( 17.38039551199336685, -10.77953091123627694, -1.500000000000002220 ) ) ;
#82119 = ORIENTED_EDGE ( 'NONE', *, *, #41900, .F. ) ;
#82120 = EDGE_LOOP ( 'NONE', ( #2389, #14837, #92613, #35088 ) ) ;
#82121 = VERTEX_POINT ( 'NONE', #96296 ) ;
#82122 = VERTEX_POINT ( 'NONE', #81072 ) ;
#82123 = CARTESIAN_POINT ( 'NONE',  ( 20.16173082093541424, 11.17373015621797627, 11.49999999999998934 ) ) ;
#82124 = CARTESIAN_POINT ( 'NONE',  ( -80.52287095715006160, -24.83602698348159876, 1.605859176311265291 ) ) ;
#82125 = CARTESIAN_POINT ( 'NONE',  ( 5.465678960246475704, -19.50585317057041124, -1.500000000000002220 ) ) ;
#82126 = ORIENTED_EDGE ( 'NONE', *, *, #18605, .F. ) ;
#82127 = AXIS2_PLACEMENT_3D ( 'NONE', #69903, #37460, #53192 ) ;
#82128 = CARTESIAN_POINT ( 'NONE',  ( -69.62287095715005592, -23.47596703998600631, 11.44779298504227683 ) ) ;
#82129 = CARTESIAN_POINT ( 'NONE',  ( -49.62287095715005592, -23.47593901973091235, -1.443836447539009749 ) ) ;
#82130 = CARTESIAN_POINT ( 'NONE',  ( -95.62359478722041217, -25.00158670708911046, 2.256160236439221034 ) ) ;
#82131 = CARTESIAN_POINT ( 'NONE',  ( -53.59317311883835089, -24.15620529776627734, 10.23563542870660825 ) ) ;
#82133 = ORIENTED_EDGE ( 'NONE', *, *, #34197, .T. ) ;
#82132 = CARTESIAN_POINT ( 'NONE',  ( -5.188002292566340934, -20.72503599944539587, 11.49999999999999645 ) ) ;
#82134 = CARTESIAN_POINT ( 'NONE',  ( 7.136624701378261548, -5.876774720514420736, 20.99078681144753844 ) ) ;
#82135 = VERTEX_POINT ( 'NONE', #35407 ) ;
#82136 = AXIS2_PLACEMENT_3D ( 'NONE', #93136, #41881, #32747 ) ;
#82137 = CARTESIAN_POINT ( 'NONE',  ( 22.02009960291501045, 3.200778107580485532, -1.500000000000002220 ) ) ;
#82138 = CARTESIAN_POINT ( 'NONE',  ( -10.41657757243416604, 17.86655067824183618, 11.49999999999998934 ) ) ;
#82139 = EDGE_CURVE ( 'NONE', #88045, #95809, #73043, .T. ) ;
#82140 = ORIENTED_EDGE ( 'NONE', *, *, #18978, .T. ) ;
#82141 = CARTESIAN_POINT ( 'NONE',  ( 3.020285327128866992, -5.876774720514407413, 19.15473963397401391 ) ) ;
#82142 = ORIENTED_EDGE ( 'NONE', *, *, #73888, .T. ) ;
#82143 = CARTESIAN_POINT ( 'NONE',  ( -61.55620429048339304, -24.66019654487199020, 8.947790411086131712 ) ) ;
#82144 = EDGE_LOOP ( 'NONE', ( #96822, #42398, #76400, #83099 ) ) ;
#82145 = CARTESIAN_POINT ( 'NONE',  ( 20.69369447470243628, -3.267675865747468489, -1.500000000000002220 ) ) ;
#82146 = CARTESIAN_POINT ( 'NONE',  ( -19.93956527825925917, 9.129326121205059152, 11.49999999999999645 ) ) ;
#82147 = DIRECTION ( 'NONE',  ( -0.000000000000000000, -1.000000000000000000, -0.000000000000000000 ) ) ;
#82148 = CARTESIAN_POINT ( 'NONE',  ( -18.95691745938505335, -12.16397891629814865, 11.49999999999998934 ) ) ;
#82149 = AXIS2_PLACEMENT_3D ( 'NONE', #23257, #54239, #53235 ) ;
#82150 = CARTESIAN_POINT ( 'NONE',  ( 17.15856466979341377, 12.00972951212132855, -1.500000000000002220 ) ) ;
#82151 = CARTESIAN_POINT ( 'NONE',  ( -92.64087933133858144, -23.48786465467241058, 11.44779295918254469 ) ) ;
#82152 = LINE ( 'NONE', #66464, #1053 ) ;
#82153 = DIRECTION ( 'NONE',  ( -1.000000000000000000, -0.000000000000000000, -0.000000000000000000 ) ) ;
#82154 = DIRECTION ( 'NONE',  ( 0.9978940991575084851, 0.000000000000000000, 0.06486421869277853025 ) ) ;
#82155 = VERTEX_POINT ( 'NONE', #97291 ) ;
#82156 = VERTEX_POINT ( 'NONE', #51120 ) ;
#82157 = ORIENTED_EDGE ( 'NONE', *, *, #42383, .F. ) ;
#82158 = CARTESIAN_POINT ( 'NONE',  ( -66.54418166932423162, -24.34968618360933235, 0.1864209137778773950 ) ) ;
#82159 = AXIS2_PLACEMENT_3D ( 'NONE', #64805, #57182, #50057 ) ;
#82160 = CARTESIAN_POINT ( 'NONE',  ( -20.86232423683148340, -5.086641213604358391, -1.500000000000002220 ) ) ;
#82161 = CARTESIAN_POINT ( 'NONE',  ( -80.62287095715005592, -29.50247984919015209, -1.443849546365053582 ) ) ;
#82163 = ORIENTED_EDGE ( 'NONE', *, *, #27740, .T. ) ;
#82162 = AXIS2_PLACEMENT_3D ( 'NONE', #83016, #60208, #75402 ) ;
#82164 = CARTESIAN_POINT ( 'NONE',  ( -11.11193726737652199, 17.91617163517716804, 11.49999999999998934 ) ) ;
#82165 = CARTESIAN_POINT ( 'NONE',  ( -1.714505518806294145E-16, -5.876774720514426953, 1.399999999999999911 ) ) ;
#82166 = CARTESIAN_POINT ( 'NONE',  ( 29.68479148105952348, -4.772774720514425972, -9.431263391055123790 ) ) ;
#82167 = CARTESIAN_POINT ( 'NONE',  ( -50.48970033773105115, -24.52399227489126687, 9.353111116836522854 ) ) ;
#82168 = AXIS2_PLACEMENT_3D ( 'NONE', #96507, #41745, #42255 ) ;
#82169 = CARTESIAN_POINT ( 'NONE',  ( 5.851028665930490646, -6.475225279485576024, -27.43979700150094558 ) ) ;
#82170 = PLANE ( 'NONE',  #69757 ) ;
#82171 = CARTESIAN_POINT ( 'NONE',  ( 21.00647827173414939, 6.864759178008983831, -1.500000000000002220 ) ) ;
#82172 = CARTESIAN_POINT ( 'NONE',  ( 11.05000000000000426, -2.000000000000000888, 24.00000000000000000 ) ) ;
#82173 = CARTESIAN_POINT ( 'NONE',  ( -3.035630128403670192, -6.376774720514413630, 19.71630089903357685 ) ) ;
#82174 = DIRECTION ( 'NONE',  ( 0.06283980576413539243, 0.000000000000000000, 0.9980236263794188822 ) ) ;
#82175 = ADVANCED_FACE ( 'NONE', ( #82064 ), #12548, .F. ) ;
#82176 = FACE_OUTER_BOUND ( 'NONE', #25337, .T. ) ;
#82177 = CARTESIAN_POINT ( 'NONE',  ( 12.02608574658498597, -17.65016651952024063, -1.500000000000002220 ) ) ;
#82178 = CARTESIAN_POINT ( 'NONE',  ( -66.52287095715006160, -23.48783264082476663, -1.443836473390092134 ) ) ;
#82179 = FACE_BOUND ( 'NONE', #94722, .T. ) ;
#82180 = CARTESIAN_POINT ( 'NONE',  ( -86.55620429048336462, -24.64898659630528854, 1.056161002820825923 ) ) ;
#82181 = DIRECTION ( 'NONE',  ( -0.000000000000000000, 1.000000000000000000, -0.000000000000000000 ) ) ;
#82182 = CARTESIAN_POINT ( 'NONE',  ( 3.115699594417459473, -22.39947108414558485, -1.500000000000002220 ) ) ;
#82183 = ORIENTED_EDGE ( 'NONE', *, *, #44167, .T. ) ;
#82184 = CARTESIAN_POINT ( 'NONE',  ( -109.5228709571500474, -24.66019654487200086, 8.947790411086119278 ) ) ;
#82185 = DIRECTION ( 'NONE',  ( 1.000000000000000000, 3.773278334444166432E-23, 8.201307841325785021E-29 ) ) ;
#82186 = CARTESIAN_POINT ( 'NONE',  ( -19.76903914530799966, 0.2396048511829373395, 11.49999999999999645 ) ) ;
#82187 = FACE_OUTER_BOUND ( 'NONE', #59444, .T. ) ;
#82188 = EDGE_CURVE ( 'NONE', #5380, #91850, #10555, .T. ) ;
#82189 = CARTESIAN_POINT ( 'NONE',  ( -67.49335235930752219, -24.65952944569304606, 1.056160979905700570 ) ) ;
#82190 = ORIENTED_EDGE ( 'NONE', *, *, #12897, .T. ) ;
#82191 = LINE ( 'NONE', #42163, #13391 ) ;
#82192 = CARTESIAN_POINT ( 'NONE',  ( -29.71166344112055668, -24.60094320703244364, 3.608441551108168444 ) ) ;
#82193 = EDGE_CURVE ( 'NONE', #35568, #14950, #5054, .T. ) ;
#82194 = CARTESIAN_POINT ( 'NONE',  ( 5.202077965628057576, -2.038091937962834166, -2.869745073849994963E-16 ) ) ;
#82195 = CARTESIAN_POINT ( 'NONE',  ( 15.46703529437019853, -15.08741104398349187, 11.49999999999998934 ) ) ;
#82196 = AXIS2_PLACEMENT_3D ( 'NONE', #65595, #12761, #96511 ) ;
#82197 = CARTESIAN_POINT ( 'NONE',  ( -49.88732701573676565, -25.10935145987042105, 2.919595231271752134 ) ) ;
#82198 = CARTESIAN_POINT ( 'NONE',  ( -18.68205546197936684, -5.105407162728520021, -1.500000000000002220 ) ) ;
#82199 = EDGE_CURVE ( 'NONE', #86774, #20204, #7426, .T. ) ;
#82200 = CARTESIAN_POINT ( 'NONE',  ( -10.21507754268103696, -3.584423063163226786, 29.48076484700401068 ) ) ;
#82201 = DIRECTION ( 'NONE',  ( 0.06975647374412546897, 0.9975640502598241977, 0.000000000000000000 ) ) ;
#82202 = CARTESIAN_POINT ( 'NONE',  ( -17.91562471463183570, -8.470225615102204841, 11.49999999999998934 ) ) ;
#82203 = ORIENTED_EDGE ( 'NONE', *, *, #93765, .T. ) ;
#82204 = ADVANCED_FACE ( 'NONE', ( #38379 ), #43998, .F. ) ;
#82205 = CARTESIAN_POINT ( 'NONE',  ( 12.36038202409810438, -16.04522380935875248, 11.49999999999999645 ) ) ;
#82206 = DIRECTION ( 'NONE',  ( -0.000000000000000000, -1.000000000000000000, -0.000000000000000000 ) ) ;
#82207 = EDGE_CURVE ( 'NONE', #44485, #59914, #46208, .T. ) ;
#82208 = CARTESIAN_POINT ( 'NONE',  ( 6.110660513271839456, -5.876774720514421624, 21.43053473047838509 ) ) ;
#82209 = ORIENTED_EDGE ( 'NONE', *, *, #58212, .F. ) ;
#82210 = FACE_OUTER_BOUND ( 'NONE', #16466, .T. ) ;
#82211 = CARTESIAN_POINT ( 'NONE',  ( -102.6228709571500275, -23.48783264082478794, -1.443836473390062158 ) ) ;
#82212 = PLANE ( 'NONE',  #100172 ) ;
#82213 = DIRECTION ( 'NONE',  ( 0.000000000000000000, 0.000000000000000000, -1.000000000000000000 ) ) ;
#82214 = DIRECTION ( 'NONE',  ( -3.773278334453079030E-23, 0.9999999999976377785, 2.173523156925979128E-06 ) ) ;
#82215 = CARTESIAN_POINT ( 'NONE',  ( -1.415466703587968667, 19.98303252902060834, -1.500000000000002220 ) ) ;
#82216 = ADVANCED_FACE ( 'NONE', ( #29272 ), #45014, .T. ) ;
#82217 = DIRECTION ( 'NONE',  ( 0.000000000000000000, -1.000000000000000000, 0.000000000000000000 ) ) ;
#82218 = ORIENTED_EDGE ( 'NONE', *, *, #24340, .F. ) ;
#82219 = VECTOR ( 'NONE', #33025, 1000.000000000000000 ) ;
#82220 = CYLINDRICAL_SURFACE ( 'NONE', #37247, 2.249999999999998668 ) ;
#82221 = DIRECTION ( 'NONE',  ( 0.000000000000000000, 0.000000000000000000, -1.000000000000000000 ) ) ;
#82222 = LINE ( 'NONE', #44172, #55138 ) ;
#82223 = CARTESIAN_POINT ( 'NONE',  ( -113.5228709571500616, -23.72747288104470087, -1.053458166803225238 ) ) ;
#82224 = VECTOR ( 'NONE', #81867, 1000.000000000000000 ) ;
#82225 = DIRECTION ( 'NONE',  ( -1.000000000000000000, -0.000000000000000000, -0.000000000000000000 ) ) ;
#82226 = CARTESIAN_POINT ( 'NONE',  ( 26.74698519091204574, -4.772774720514425972, -10.98683230472874151 ) ) ;
#82227 = VERTEX_POINT ( 'NONE', #53628 ) ;
#82228 = VECTOR ( 'NONE', #76777, 1000.000000000000000 ) ;
#82229 = CARTESIAN_POINT ( 'NONE',  ( 13.61570878652767291, 15.11107311891478666, -1.500000000000002220 ) ) ;
#82230 = VERTEX_POINT ( 'NONE', #29773 ) ;
#82231 = EDGE_CURVE ( 'NONE', #88368, #98147, #83552, .T. ) ;
#82232 = CARTESIAN_POINT ( 'NONE',  ( 21.75294195941402364, -7.338126679257295670, 11.49999999999998934 ) ) ;
#82233 = CARTESIAN_POINT ( 'NONE',  ( 29.60459817610514932, 4.854569207680477838, 28.81138945959710185 ) ) ;
#82234 = ORIENTED_EDGE ( 'NONE', *, *, #12563, .T. ) ;
#82235 = CARTESIAN_POINT ( 'NONE',  ( -89.62287095715002749, -23.48783264082478439, -1.443836473390063713 ) ) ;
#82237 = EDGE_CURVE ( 'NONE', #65949, #52778, #91169, .T. ) ;
#82236 = CARTESIAN_POINT ( 'NONE',  ( -49.44941220326682441, -25.12215325162356905, 6.666982529036616256 ) ) ;
#82238 = CARTESIAN_POINT ( 'NONE',  ( -125.6228709571500559, -29.50248789122583659, 2.256150453626215580 ) ) ;
#82240 = ORIENTED_EDGE ( 'NONE', *, *, #4546, .T. ) ;
#82239 = CARTESIAN_POINT ( 'NONE',  ( 16.79009078985406234, 12.93418496121567252, 11.49999999999999645 ) ) ;
#82241 = EDGE_LOOP ( 'NONE', ( #64061, #32070, #36258, #32864 ) ) ;
#82242 = CARTESIAN_POINT ( 'NONE',  ( -0.8124730928778809425, -22.15030348749839817, -1.500000000000002220 ) ) ;
#82243 = CARTESIAN_POINT ( 'NONE',  ( 17.30552477474510908, -11.17933342135444086, -1.500000000000002220 ) ) ;
#82244 = VERTEX_POINT ( 'NONE', #92657 ) ;
#82245 = ORIENTED_EDGE ( 'NONE', *, *, #23512, .T. ) ;
#82246 = DIRECTION ( 'NONE',  ( -3.773278334453079618E-23, 0.9999999999976377785, 2.173523156925979975E-06 ) ) ;
#82247 = ADVANCED_FACE ( 'NONE', ( #23137 ), #45513, .F. ) ;
#82248 = CARTESIAN_POINT ( 'NONE',  ( -87.62287095715004170, -29.50248528299804818, 1.056150453629040253 ) ) ;
#82249 = ORIENTED_EDGE ( 'NONE', *, *, #34085, .F. ) ;
#82250 = VERTEX_POINT ( 'NONE', #44506 ) ;
#82251 =( REPRESENTATION_RELATIONSHIP ('NONE','NONE', #96270, #50921 ) REPRESENTATION_RELATIONSHIP_WITH_TRANSFORMATION ( #36907 )SHAPE_REPRESENTATION_RELATIONSHIP( ) );
#82252 =( BOUNDED_CURVE ( )  B_SPLINE_CURVE ( 3, ( #17716, #48685, #11098, #72512 ),
 .UNSPECIFIED., .F., .F. ) 
 B_SPLINE_CURVE_WITH_KNOTS ( ( 4, 4 ),
 ( 4.603180203402792436, 4.712388980384689674 ),
 .UNSPECIFIED. ) 
 CURVE ( )  GEOMETRIC_REPRESENTATION_ITEM ( )  RATIONAL_B_SPLINE_CURVE ( ( 1.000000000000000000, 0.9990063671772055898, 0.9990063671772055898, 1.000000000000000000 ) ) 
 REPRESENTATION_ITEM ( '' )  );
#82253 = ORIENTED_EDGE ( 'NONE', *, *, #71566, .F. ) ;
#82254 = CARTESIAN_POINT ( 'NONE',  ( -49.52287095715006160, -24.64965694238406613, 8.947790433994203596 ) ) ;
#82255 = CARTESIAN_POINT ( 'NONE',  ( -28.52198423978972741, -23.32371265842308716, 11.44779300624184160 ) ) ;
#82256 = CARTESIAN_POINT ( 'NONE',  ( -119.6228709571500559, -23.48783264082479150, -1.443836473390058384 ) ) ;
#82257 = CARTESIAN_POINT ( 'NONE',  ( -12.88759680649768136, 16.30154091734715749, -1.500000000000002220 ) ) ;
#82259 = ADVANCED_FACE ( 'NONE', ( #75934 ), #82556, .F. ) ;
#82258 = CARTESIAN_POINT ( 'NONE',  ( -18.02536786162489335, -12.12045427182966861, 11.49999999999999645 ) ) ;
#82260 = VERTEX_POINT ( 'NONE', #15037 ) ;
#82261 = CARTESIAN_POINT ( 'NONE',  ( -51.93149462243456327, -25.24900417239232908, 6.174051150523328424 ) ) ;
#82262 = DIRECTION ( 'NONE',  ( 0.000000000000000000, 1.000000000000000000, 5.204170427930421283E-15 ) ) ;
#82263 = VECTOR ( 'NONE', #96141, 1000.000000000000000 ) ;
#82264 = CARTESIAN_POINT ( 'NONE',  ( -115.5168712054073410, -24.40034930558990567, 0.3402023900116066257 ) ) ;
#82265 = CARTESIAN_POINT ( 'NONE',  ( -19.61019785865472542, -10.87575402790796453, 11.49999999999998934 ) ) ;
#82266 = CARTESIAN_POINT ( 'NONE',  ( -50.56373716527822637, -25.31296762218556395, 4.723080049254409829 ) ) ;
#82267 = PLANE ( 'NONE',  #88622 ) ;
#82268 = VERTEX_POINT ( 'NONE', #30262 ) ;
#82269 = CARTESIAN_POINT ( 'NONE',  ( -75.52287095715006160, -23.84047902841601285, -0.8780736468305737619 ) ) ;
#82270 = CARTESIAN_POINT ( 'NONE',  ( 13.12137440454564796, -3.706387542726002682, -28.15098661896695376 ) ) ;
#82271 = B_SPLINE_CURVE_WITH_KNOTS ( 'NONE', 3,
 ( #95694, #87077, #79463, #82332, #50898, #9955 ),
 .UNSPECIFIED., .F., .F.,
 ( 4, 2, 4 ),
 ( 6.391158118955278476E-06, 0.001387004593080777256, 0.002767618028042598960 ),
 .UNSPECIFIED. ) ;
#82272 = B_SPLINE_SURFACE_WITH_KNOTS ( 'NONE', 3, 3, ( 
 ( #44084, #45590, #98854, #92246 ),
 ( #51699, #82632, #60321, #91248 ),
 ( #45091, #90255, #97854, #21721 ),
 ( #52695, #68915, #84635, #36462 ),
 ( #6519, #37471, #98352, #5018 ),
 ( #83634, #14116, #29850, #22717 ),
 ( #60821, #74526, #20730, #67427 ) ),
 .UNSPECIFIED., .F., .F., .F.,
 ( 4, 3, 4 ),
 ( 4, 4 ),
 ( 0.0004767420375739903028, 0.1029714262224254440, 0.2054661104072768862 ),
 ( 0.06486343431056791620, 0.06976593829091715104 ),
 .UNSPECIFIED. ) ;
#82273 = ORIENTED_EDGE ( 'NONE', *, *, #6382, .F. ) ;
#82274 = ORIENTED_EDGE ( 'NONE', *, *, #18217, .T. ) ;
#82275 = FACE_OUTER_BOUND ( 'NONE', #80267, .T. ) ;
#82276 = APPROVAL ( #5197, 'UNSPECIFIED' ) ;
#82277 = ORIENTED_EDGE ( 'NONE', *, *, #9814, .T. ) ;
#82278 = CARTESIAN_POINT ( 'NONE',  ( 14.64190796094839264, -15.47823801613018269, -1.500000000000002220 ) ) ;
#82279 = ORIENTED_EDGE ( 'NONE', *, *, #6844, .T. ) ;
#82280 = CARTESIAN_POINT ( 'NONE',  ( -58.62287095715004881, -24.64898659630367916, 1.056161002820822592 ) ) ;
#82281 = CARTESIAN_POINT ( 'NONE',  ( 19.20967809413044236, -10.42350525531561978, -1.500000000000002220 ) ) ;
#82282 = CARTESIAN_POINT ( 'NONE',  ( -124.5562042904833930, -23.47596703998600631, 11.44779298504227683 ) ) ;
#82283 = CARTESIAN_POINT ( 'NONE',  ( 2.290073164716609710, 22.57640404599860418, -1.500000000000002220 ) ) ;
#82284 = DIRECTION ( 'NONE',  ( -3.773278334453079618E-23, 0.9999999999976377785, 2.173523156925979975E-06 ) ) ;
#82285 = DIRECTION ( 'NONE',  ( -0.000000000000000000, -1.000000000000000000, -0.000000000000000000 ) ) ;
#82286 = CARTESIAN_POINT ( 'NONE',  ( 18.32745805453730981, -11.99952526121574259, -1.500000000000002220 ) ) ;
#82287 = LINE ( 'NONE', #20877, #2581 ) ;
#82288 = ORIENTED_EDGE ( 'NONE', *, *, #52422, .F. ) ;
#82289 = CARTESIAN_POINT ( 'NONE',  ( -122.5913845940917213, -23.73791477778912551, 11.05961554403169878 ) ) ;
#82290 = FACE_OUTER_BOUND ( 'NONE', #94498, .T. ) ;
#82291 = AXIS2_PLACEMENT_3D ( 'NONE', #74827, #91055, #11938 ) ;
#82292 = ORIENTED_EDGE ( 'NONE', *, *, #77598, .F. ) ;
#82293 = CARTESIAN_POINT ( 'NONE',  ( -105.5228709571500758, -29.50250243563736774, 8.947779886222136270 ) ) ;
#82294 = CARTESIAN_POINT ( 'NONE',  ( 8.255033872309153864, 6.475225279485571583, -27.10684724722607442 ) ) ;
#82295 = CARTESIAN_POINT ( 'NONE',  ( -0.07188169300783608939, -22.11943499646449141, 0.5637492489085879077 ) ) ;
#82296 = CARTESIAN_POINT ( 'NONE',  ( -21.25539211000977957, 0.9166567589900279645, 11.49999999999998934 ) ) ;
#82297 = CARTESIAN_POINT ( 'NONE',  ( -55.62287095715007013, -24.92604778743017491, 8.074972756849359001 ) ) ;
#82298 = CARTESIAN_POINT ( 'NONE',  ( -26.21213932664330670, -24.97064719818860468, 3.737063582475403933 ) ) ;
#82299 = CARTESIAN_POINT ( 'NONE',  ( -85.63840790987890728, -24.15503026093914229, -0.2815557561904377115 ) ) ;
#82300 = AXIS2_PLACEMENT_3D ( 'NONE', #90375, #58937, #75146 ) ;
#82301 = FACE_OUTER_BOUND ( 'NONE', #87402, .T. ) ;
#82302 = CARTESIAN_POINT ( 'NONE',  ( 7.160000000000000142, -6.754662360505032659, 7.925641719537454222 ) ) ;
#82303 = EDGE_LOOP ( 'NONE', ( #87982, #89775, #86820, #59288, #79132, #36819 ) ) ;
#82304 = CARTESIAN_POINT ( 'NONE',  ( 6.866622826037362515, -18.30913693658520103, 11.49999999999999645 ) ) ;
#82305 = CARTESIAN_POINT ( 'NONE',  ( -58.62287095715004881, -23.48786465467241769, 11.44779295918254824 ) ) ;
#82306 = CIRCLE ( 'NONE', #98441, 0.2499999999997798983 ) ;
#82307 = EDGE_CURVE ( 'NONE', #5350, #38938, #37394, .T. ) ;
#82308 = LINE ( 'NONE', #36139, #28563 ) ;
#82309 = ORIENTED_EDGE ( 'NONE', *, *, #57848, .F. ) ;
#82310 = CARTESIAN_POINT ( 'NONE',  ( 3.879810481058463711, -5.876774720514426953, 21.83835767234735670 ) ) ;
#82311 = CARTESIAN_POINT ( 'NONE',  ( -99.46521863968663979, -25.31559379708168223, 5.025132061053519728 ) ) ;
#82312 = CARTESIAN_POINT ( 'NONE',  ( -31.62287095715005236, -24.50216790748098461, 0.6166512839513674793 ) ) ;
#82313 = CARTESIAN_POINT ( 'NONE',  ( -40.62287095715004170, -24.99156045073392463, 7.747789690856161648 ) ) ;
#82314 = CARTESIAN_POINT ( 'NONE',  ( 14.14096853472169535, -13.71769858867784464, -1.500000000000002220 ) ) ;
#82315 = AXIS2_PLACEMENT_3D ( 'NONE', #92550, #31153, #85435 ) ;
#82316 = ORIENTED_EDGE ( 'NONE', *, *, #85917, .T. ) ;
#82317 = ADVANCED_FACE ( 'NONE', ( #67852 ), #99275, .F. ) ;
#82318 = DIRECTION ( 'NONE',  ( -0.4771587602595986910, -0.8788171126619707119, 0.000000000000000000 ) ) ;
#82319 = CARTESIAN_POINT ( 'NONE',  ( 30.93860345374796594, -6.475225279485573360, 13.17908622612278613 ) ) ;
#82320 = ADVANCED_FACE ( 'NONE', ( #30769 ), #74931, .F. ) ;
#82321 = PERSON_AND_ORGANIZATION_ROLE ( 'design_owner' ) ;
#82322 = ORIENTED_EDGE ( 'NONE', *, *, #64753, .T. ) ;
#82323 = CARTESIAN_POINT ( 'NONE',  ( 0.3910256410256383042, -6.376774720514408301, 19.19230769230768985 ) ) ;
#82324 = CARTESIAN_POINT ( 'NONE',  ( -45.62287095715004881, -24.52323809116984421, 9.355190652339420154 ) ) ;
#82325 = CARTESIAN_POINT ( 'NONE',  ( -55.64837685101972653, -24.15503026093915295, -0.2815557561904505901 ) ) ;
#82326 = DIRECTION ( 'NONE',  ( 1.000000000000000000, 3.773278334444166432E-23, 8.201307841325785021E-29 ) ) ;
#82327 = CARTESIAN_POINT ( 'NONE',  ( -31.62287095715005236, -23.72773821059535493, 11.05748984161097503 ) ) ;
#82328 = CARTESIAN_POINT ( 'NONE',  ( -32.07722060962682775, -24.86441978397624553, 8.247789967200544581 ) ) ;
#82329 = CARTESIAN_POINT ( 'NONE',  ( -107.6262949015405042, -24.34968618360934300, 0.1864209137778969627 ) ) ;
#82330 = CARTESIAN_POINT ( 'NONE',  ( 18.23660095519748481, -8.086948576924280374, -1.500000000000002220 ) ) ;
#82331 = EDGE_CURVE ( 'NONE', #99388, #63165, #28776, .T. ) ;
#82332 = CARTESIAN_POINT ( 'NONE',  ( -54.52287095715005449, -24.35013146730203815, 9.818937971375104823 ) ) ;
#82333 = CARTESIAN_POINT ( 'NONE',  ( -0.001635060676233153704, -23.02883285463877527, 4.281990464225436277 ) ) ;
#82334 = ORIENTED_EDGE ( 'NONE', *, *, #69592, .F. ) ;
#82335 = LINE ( 'NONE', #43293, #41089 ) ;
#82336 = CARTESIAN_POINT ( 'NONE',  ( 4.628547153713393314, -5.876774720514418071, 20.50654586986123817 ) ) ;
#82337 = SHAPE_REPRESENTATION_RELATIONSHIP ( 'NONE' , 'NONE' ,  #91803, #508 ) ;
#82338 = CARTESIAN_POINT ( 'NONE',  ( -80.50190673274472886, -24.52399227489127043, 9.353111116836524630 ) ) ;
#82339 = DIRECTION ( 'NONE',  ( -1.000000000000000000, -0.000000000000000000, -0.000000000000000000 ) ) ;
#82340 = CARTESIAN_POINT ( 'NONE',  ( -39.56973724660041825, -23.48783264082476308, -1.443836473390098352 ) ) ;
#82341 = CARTESIAN_POINT ( 'NONE',  ( -64.52287095715006160, -24.51283580621364422, 0.6167428607019732612 ) ) ;
#82342 = FACE_OUTER_BOUND ( 'NONE', #67385, .T. ) ;
#82343 = ORIENTED_EDGE ( 'NONE', *, *, #1754, .T. ) ;
#82344 = B_SPLINE_SURFACE_WITH_KNOTS ( 'NONE', 3, 1, ( 
 ( #45724, #69055 ),
 ( #62454, #39099 ),
 ( #8161, #92882 ),
 ( #85272, #16763 ),
 ( #31490, #9154 ),
 ( #32500, #1560 ),
 ( #71070, #63472 ),
 ( #94394, #23361 ),
 ( #70056, #47731 ),
 ( #1054, #78148 ),
 ( #24876, #15763 ) ),
 .UNSPECIFIED., .F., .F., .F.,
 ( 4, 1, 1, 1, 1, 1, 1, 1, 4 ),
 ( 2, 2 ),
 ( 0.000000000000000000, 0.1411571637912756305, 0.2777725246444866514, 0.4092439672982337573, 0.5356759015826428882, 0.6574965059498953934, 0.7754582459464036681, 0.8894116614046648772, 1.000000000000000000 ),
 ( 0.000000000000000000, 1.000000000000000000 ),
 .UNSPECIFIED. ) ;
#82345 = CARTESIAN_POINT ( 'NONE',  ( -37.62287095715007013, -23.47596703998600276, 11.44779298504227505 ) ) ;
#82346 = PLANE ( 'NONE',  #37095 ) ;
#82347 = ORIENTED_EDGE ( 'NONE', *, *, #91709, .T. ) ;
#82348 = CARTESIAN_POINT ( 'NONE',  ( 8.147030896810244727, 18.52525024547675869, -1.500000000000002220 ) ) ;
#82349 = CARTESIAN_POINT ( 'NONE',  ( -6.741682653110981249, 5.965225279485572685, 30.62569541381301619 ) ) ;
#82350 = DIRECTION ( 'NONE',  ( 0.000000000000000000, -1.000000000000000000, 0.000000000000000000 ) ) ;
#82351 = CIRCLE ( 'NONE', #48403, 0.2499999999997798983 ) ;
#82352 = CARTESIAN_POINT ( 'NONE',  ( -82.62287095715007013, -24.66019654487199375, 8.947790411086128159 ) ) ;
#82353 = ORIENTED_EDGE ( 'NONE', *, *, #72599, .F. ) ;
#82355 = EDGE_CURVE ( 'NONE', #37700, #97841, #8434, .T. ) ;
#82354 = CARTESIAN_POINT ( 'NONE',  ( -106.5228709571500758, -23.47596703998600631, 11.44779298504228038 ) ) ;
#82356 = CARTESIAN_POINT ( 'NONE',  ( -2.196420576317535289, -6.376774720514410077, 19.14926908420044782 ) ) ;
#82357 = CARTESIAN_POINT ( 'NONE',  ( 15.05167116458888010, 13.23127732593390959, -1.500000000000002220 ) ) ;
#82358 = CARTESIAN_POINT ( 'NONE',  ( 15.37114825158464271, 14.37155165002682544, 11.49999999999999645 ) ) ;
#82359 = DIRECTION ( 'NONE',  ( -3.773278334453079618E-23, 0.9999999999976377785, 2.173523156925979975E-06 ) ) ;
#82360 = CARTESIAN_POINT ( 'NONE',  ( -32.52287095715006160, -23.48783264083359867, -1.443836473376375329 ) ) ;
#82361 = CARTESIAN_POINT ( 'NONE',  ( -19.90388773112789167, 9.559999800501117306, 11.49999999999998934 ) ) ;
#82362 = ADVANCED_FACE ( 'NONE', ( #38876 ), #86056, .T. ) ;
#82363 = CARTESIAN_POINT ( 'NONE',  ( -66.58953762381673869, -24.66019654487198665, 8.947790411086131712 ) ) ;
#82364 = EDGE_CURVE ( 'NONE', #70394, #3440, #75606, .T. ) ;
#82365 = CARTESIAN_POINT ( 'NONE',  ( -87.52287095715006160, -24.65952944569304606, 1.056160979905700570 ) ) ;
#82366 = CARTESIAN_POINT ( 'NONE',  ( -118.5562042904833930, -24.64898659630529565, 1.056161002820835026 ) ) ;
#82367 = ORIENTED_EDGE ( 'NONE', *, *, #36637, .F. ) ;
#82368 = CARTESIAN_POINT ( 'NONE',  ( -89.40841769935764205, -25.30749613935913089, 3.864043853429952158 ) ) ;
#82369 = CARTESIAN_POINT ( 'NONE',  ( -31.51236532535822832, -23.73766607897669800, -1.055555164236445131 ) ) ;
#82370 = ORIENTED_EDGE ( 'NONE', *, *, #28808, .F. ) ;
#82371 = AXIS2_PLACEMENT_3D ( 'NONE', #71366, #4720, #98043 ) ;
#82372 = ORIENTED_EDGE ( 'NONE', *, *, #55562, .T. ) ;
#82373 = FACE_OUTER_BOUND ( 'NONE', #23511, .T. ) ;
#82374 = CARTESIAN_POINT ( 'NONE',  ( 5.802984775641024662, -6.376774720514402972, 18.35026041666666430 ) ) ;
#82375 = FACE_OUTER_BOUND ( 'NONE', #16355, .T. ) ;
#82376 = CARTESIAN_POINT ( 'NONE',  ( -20.42507745660439156, -2.452541965221147535, -1.500000000000002220 ) ) ;
#82377 = CARTESIAN_POINT ( 'NONE',  ( -15.49073194614445015, 15.02706685249526686, 11.49999999999999645 ) ) ;
#82378 = ORIENTED_EDGE ( 'NONE', *, *, #32774, .F. ) ;
#82379 = CARTESIAN_POINT ( 'NONE',  ( -91.52216445584937787, -23.48783264082477018, -1.443836473390090802 ) ) ;
#82380 = CARTESIAN_POINT ( 'NONE',  ( -99.21406825799371632, -25.29348853684751575, 4.454428177689103485 ) ) ;
#82381 = CARTESIAN_POINT ( 'NONE',  ( -4.141025641025642301, -6.376774720514411854, 19.63681891025641235 ) ) ;
#82382 = CARTESIAN_POINT ( 'NONE',  ( 14.50327815619135308, -17.01817589256642194, 11.49999999999998934 ) ) ;
#82383 = CARTESIAN_POINT ( 'NONE',  ( 29.70264281947218876, -3.584400861594816856, 28.19233905662918005 ) ) ;
#82384 = CARTESIAN_POINT ( 'NONE',  ( -82.58953762381672448, -23.47593901973091235, -1.443836447539004642 ) ) ;
#82385 = ORIENTED_EDGE ( 'NONE', *, *, #65397, .T. ) ;
#82386 = CARTESIAN_POINT ( 'NONE',  ( -50.62287095715005592, -25.00182538069145011, 7.747789668545097541 ) ) ;
#82387 = CARTESIAN_POINT ( 'NONE',  ( -96.52287095715006160, -23.48786465467241769, 11.44779295918254114 ) ) ;
#82388 = CARTESIAN_POINT ( 'NONE',  ( -13.97254113366623152, 15.51630364309664856, 11.49999999999998934 ) ) ;
#82389 = ORIENTED_EDGE ( 'NONE', *, *, #96841, .F. ) ;
#82390 = ADVANCED_FACE ( 'NONE', ( #56129 ), #94161, .T. ) ;
#82392 = VERTEX_POINT ( 'NONE', #46499 ) ;
#82391 = CARTESIAN_POINT ( 'NONE',  ( -39.05155750314200702, -25.26703200855950016, 4.030863154173684570 ) ) ;
#82393 = VERTEX_POINT ( 'NONE', #54615 ) ;
#82394 = CARTESIAN_POINT ( 'NONE',  ( -100.6278523261951676, -24.63419186844610920, 9.035850630976920428 ) ) ;
#82395 = CARTESIAN_POINT ( 'NONE',  ( 14.48694714638828884, 15.39972936300609341, -1.500000000000002220 ) ) ;
#82396 = ORIENTED_EDGE ( 'NONE', *, *, #5274, .F. ) ;
#82397 = CARTESIAN_POINT ( 'NONE',  ( -117.6250645124119103, -24.34968618360934656, 0.1864209137778901626 ) ) ;
#82398 = CARTESIAN_POINT ( 'NONE',  ( -98.55620429048337883, -23.48783264082478084, -1.443836473390061936 ) ) ;
#82399 = CARTESIAN_POINT ( 'NONE',  ( -129.5562042904834072, -23.48786465467241413, 11.44779295918253581 ) ) ;
#82400 = PLANE ( 'NONE',  #12900 ) ;
#82401 = CARTESIAN_POINT ( 'NONE',  ( 7.234974673537251100, -5.876774720514415407, 19.99114326857715795 ) ) ;
#82402 = CARTESIAN_POINT ( 'NONE',  ( -16.45766974254678061, 14.19212061201335473, -1.500000000000002220 ) ) ;
#82403 = CARTESIAN_POINT ( 'NONE',  ( -80.30325611392450469, -25.04485593722630554, 7.554940489935124681 ) ) ;
#82405 = ORIENTED_EDGE ( 'NONE', *, *, #25652, .F. ) ;
#82404 = CARTESIAN_POINT ( 'NONE',  ( -5.491053050139323766, 21.65304554001118120, 11.49999999999999645 ) ) ;
#82406 = DIRECTION ( 'NONE',  ( -3.773278334453079618E-23, 0.9999999999976377785, 2.173523156925979975E-06 ) ) ;
#82407 = CARTESIAN_POINT ( 'NONE',  ( -95.58953762381673869, -23.48786465467241769, 11.44779295918254114 ) ) ;
#82408 = CARTESIAN_POINT ( 'NONE',  ( -31.62287095715005236, -24.64898659630367206, 1.056161002820817485 ) ) ;
#82409 = VERTEX_POINT ( 'NONE', #78933 ) ;
#82410 = EDGE_CURVE ( 'NONE', #22977, #96621, #15534, .T. ) ;
#82411 = ADVANCED_FACE ( 'NONE', ( #69840 ), #78432, .F. ) ;
#82412 = ORIENTED_EDGE ( 'NONE', *, *, #91149, .T. ) ;
#82413 = EDGE_LOOP ( 'NONE', ( #98948, #23215, #79854, #41962 ) ) ;
#82414 = CARTESIAN_POINT ( 'NONE',  ( -33.62287095715005592, -23.47593901973091235, -1.443836447539013301 ) ) ;
#82415 = DIRECTION ( 'NONE',  ( -3.773278334453079030E-23, 0.9999999999976377785, 2.173523156925979128E-06 ) ) ;
#82416 = CARTESIAN_POINT ( 'NONE',  ( 30.61220459279984496, -3.931892516571728446, 27.21038724104498385 ) ) ;
#82417 = CARTESIAN_POINT ( 'NONE',  ( -43.62287095715004170, -23.95044443724992078, 10.65354141964649948 ) ) ;
#82418 = CARTESIAN_POINT ( 'NONE',  ( 31.46635748159467383, 4.132774720514425404, -3.372935991075822759 ) ) ;
#82419 = CARTESIAN_POINT ( 'NONE',  ( -10.34999999999999254, 0.000000000000000000, -2.500000000000001332 ) ) ;
#82420 = ORIENTED_EDGE ( 'NONE', *, *, #53255, .T. ) ;
#82421 = CARTESIAN_POINT ( 'NONE',  ( -8.550378450311910683, 17.38971893761031851, 11.49999999999999645 ) ) ;
#82422 = CARTESIAN_POINT ( 'NONE',  ( 29.80070917940689412, 6.376774720514426953, 27.39560796525321607 ) ) ;
#82423 = AXIS2_PLACEMENT_3D ( 'NONE', #51608, #58718, #89669 ) ;
#82424 = EDGE_CURVE ( 'NONE', #12723, #34128, #70337, .T. ) ;
#82425 = ORIENTED_EDGE ( 'NONE', *, *, #85922, .F. ) ;
#82426 = CARTESIAN_POINT ( 'NONE',  ( 3.085011456917871264, -6.376774720514408301, 19.00082519311127172 ) ) ;
#82427 = CARTESIAN_POINT ( 'NONE',  ( 6.190876379491990988, 5.356774720513712396, -27.38145113946987408 ) ) ;
#82428 = DIRECTION ( 'NONE',  ( -0.000000000000000000, -0.000000000000000000, -1.000000000000000000 ) ) ;
#82429 = VECTOR ( 'NONE', #80342, 1000.000000000000114 ) ;
#82430 = CARTESIAN_POINT ( 'NONE',  ( -36.52287095715006870, -23.48786465467240347, 11.44779295918255180 ) ) ;
#82431 = CARTESIAN_POINT ( 'NONE',  ( 18.62133539762988121, 6.091496293051981148, -1.500000000000002220 ) ) ;
#82432 = CARTESIAN_POINT ( 'NONE',  ( 19.24418710706453339, 0.000000000000000000, -2.153101996372891236 ) ) ;
#82433 = ORIENTED_EDGE ( 'NONE', *, *, #16129, .F. ) ;
#82434 = CARTESIAN_POINT ( 'NONE',  ( 8.794441374123232791, -19.68457759291379716, 11.49999999999998934 ) ) ;
#82435 = VECTOR ( 'NONE', #7316, 999.9999999999998863 ) ;
#82436 = CARTESIAN_POINT ( 'NONE',  ( -33.65006591098492805, -23.96169478059712432, 10.65365249895719124 ) ) ;
#82437 = CARTESIAN_POINT ( 'NONE',  ( -70.42265764498320380, -25.25639600851986089, 7.098707395884841453 ) ) ;
#82438 = CARTESIAN_POINT ( 'NONE',  ( -40.50924942470576440, -23.85016227208580730, -0.8807180028928395243 ) ) ;
#82439 = CARTESIAN_POINT ( 'NONE',  ( -100.1584806888234738, -25.18439341914872287, 3.322325955448823365 ) ) ;
#82440 = CARTESIAN_POINT ( 'NONE',  ( -1.485350438481424895, -22.96994831426971828, -1.500000000000002220 ) ) ;
#82441 = EDGE_CURVE ( 'NONE', #97857, #32699, #63238, .T. ) ;
#82442 = EDGE_CURVE ( 'NONE', #25123, #88484, #79986, .T. ) ;
#82443 = PERSON_AND_ORGANIZATION_ROLE ( 'creator' ) ;
#82444 = CARTESIAN_POINT ( 'NONE',  ( 0.2450472757604422180, -5.405843919193447533, 8.999999999999998224 ) ) ;
#82445 = DIRECTION ( 'NONE',  ( 0.2488812114211667315, 0.000000000000000000, 0.9685340172660600322 ) ) ;
#82446 = CARTESIAN_POINT ( 'NONE',  ( 1.915021276000606454, 20.04344799065331628, 11.49999999999999645 ) ) ;
#82447 = CARTESIAN_POINT ( 'NONE',  ( -92.62287095715005592, -23.47596703998600631, 11.44779298504227860 ) ) ;
#82448 = CARTESIAN_POINT ( 'NONE',  ( -36.62287095715005592, -29.50248528299804818, 1.056150453629031594 ) ) ;
#82449 = VECTOR ( 'NONE', #8341, 1000.000000000000000 ) ;
#82450 = CARTESIAN_POINT ( 'NONE',  ( -94.62287095715005592, -23.48786465467241769, 11.44779295918254114 ) ) ;
#82451 = CARTESIAN_POINT ( 'NONE',  ( 21.57151214508649772, 3.625915217019311583E-15, 0.000000000000000000 ) ) ;
#82452 = CARTESIAN_POINT ( 'NONE',  ( -111.0533842133887390, -25.29779214506538310, 3.566049847669544359 ) ) ;
#82453 = CARTESIAN_POINT ( 'NONE',  ( 10.41257876278241845, -16.90412932818451353, 11.49999999999998934 ) ) ;
#82454 = EDGE_CURVE ( 'NONE', #21831, #88746, #14052, .T. ) ;
#82455 = CARTESIAN_POINT ( 'NONE',  ( -94.52287095715007581, -23.72773821059536203, 11.05748984161097681 ) ) ;
#82456 = CARTESIAN_POINT ( 'NONE',  ( 19.69962056004252560, 1.334664424591413434, -1.500000000000002220 ) ) ;
#82457 = CARTESIAN_POINT ( 'NONE',  ( -42.57643649038576683, -24.65952944569304606, 1.056160979905694353 ) ) ;
#82458 = EDGE_CURVE ( 'NONE', #69448, #57047, #84828, .T. ) ;
#82459 = DESIGN_CONTEXT ( 'detailed design', #35596, 'design' ) ;
#82460 = CARTESIAN_POINT ( 'NONE',  ( 15.99960863614631101, -3.577630190450212577, -27.91116951066581819 ) ) ;
#82461 = CARTESIAN_POINT ( 'NONE',  ( 3.787259615384621636, -6.376774720514404748, 18.51923076923076650 ) ) ;
#82462 = CARTESIAN_POINT ( 'NONE',  ( 20.01179378540625819, 5.277757631783551950, 11.49999999999999645 ) ) ;
#82463 = CARTESIAN_POINT ( 'NONE',  ( -39.53777310077231277, -25.31628728160307062, 5.501674862403532984 ) ) ;
#82464 = B_SPLINE_CURVE_WITH_KNOTS ( 'NONE', 3,
 ( #74404, #97738, #4898, #13492 ),
 .UNSPECIFIED., .F., .F.,
 ( 4, 4 ),
 ( 0.9204431904296468403, 0.9294496217017622630 ),
 .UNSPECIFIED. ) ;
#82465 = CARTESIAN_POINT ( 'NONE',  ( 32.42932432802503939, 5.965225279485572685, -0.2107846672978405389 ) ) ;
#82466 = CLOSED_SHELL ( 'NONE', ( #33239, #56577, #68710, #10740, #65852, #37874, #96050, #68117, #81748, #8762, #22946, #82175, #50090, #21916, #51723, #39729, #27371, #85224, #66326, #613, #46804, #9132, #71430, #4412, #92489, #32031, #93074, #22512, #76168, #70076, #41659, #97912, #62210, #44671, #17706, #37965, #223, #721, #63529, #26069, #48983, #1027, #87861, #68933, #39029, #70061, #46444, #14283, #3341, #32350, #18718, #48903, #82784, #27686, #65276, #29434, #5529, #88965, #79732, #97818, #24256, #48539, #7493, #40068, #13906, #18523, #18613, #36384, #91758, #95046, #56315, #94950, #37068, #89764, #86355, #42457, #32355, #14577, #60999, #83766, #41076, #49486, #22398, #54078, #195, #20424, #50287, #36585, #94009, #94437, #12073, #26428, #30924, #85529, #85571, #83827, #68256, #43401, #57811, #30464, #80190, #51218, #94692, #12029, #29285, #75658, #51416, #11285, #44002, #26980, #69122, #27881, #32870, #67212, #29547, #54816, #100149, #88434, #80546, #41657, #16069, #45224, #75541, #35689, #93195, #60098, #18449, #8356, #84760, #56349, #53878, #81269, #51279, #72249, #42938, #2821, #40162, #57993, #48406, #11675, #90576, #4678, #54949, #84268, #47297, #36272, #27851, #34609, #72446, #85619, #75551, #13030, #53476, #41668, #39802, #28499, #44062, #44094, #17784, #24954, #6027, #16732, #71234, #41004, #91214, #29291, #51102, #30651, #14932, #95709, #43384, #33050, #49801, #93748, #55287, #78040, #33208, #26474, #85659, #15203, #48964, #63625, #1354, #71666, #496, #26548, #49346, #49111, #27699, #59509, #75235, #15737, #62596, #81330, #84025, #67022, #21527, #13782, #61009, #11272, #10722, #53578, #70577, #16218, #98348, #99856, #59935, #41183, #22861, #56337, #33801, #56, #47004, #59881, #66015, #34756, #5914, #49796, #29176, #53944, #63424, #25137, #50719, #95425, #86877, #79029, #97974, #69126, #10401, #72876, #75969, #46118, #45708, #88721, #11515, #9043, #36740, #63998, #27318, #42976, #14260, #83700, #49033, #95464, #4569, #65557, #66100, #1372, #31557, #92401, #44785, #39039, #22890, #72943, #50201, #32401, #5661, #25966, #96125, #88030, #91337, #58497, #30889, #22996, #88163, #21489, #31113, #73144, #63659, #79610, #9069, #78161, #56924, #83235, #56663, #26416, #27909, #88748, #42021, #15384, #90097, #70269, #95611, #19303, #44032, #66578, #68259, #97426, #68568, #48459, #69368, #36625, #24509, #35524, #68818, #25206, #90219, #10434, #48448, #2017, #29141, #42062, #62399, #1934, #8193, #46268, #55400, #61507, #45863, #42336, #67582, #14887, #67643, #2012, #45098, #78023, #58846, #38697, #77241, #20013, #20235, #44993, #72957, #99632, #84830, #16753, #35068, #69477, #25728, #32157, #8426, #66476, #58603, #98955, #51402, #10267, #75637, #90381, #58616, #33673, #34256, #40301, #81142, #13215, #91588, #60201, #78524, #6481, #76629, #52212, #76448, #44651, #8078, #4978, #42527, #26183, #85852, #75616, #97214, #44654, #100388, #16491, #47937, #100024, #96196, #65675, #25590, #66823, #59672, #56153, #6806, #35339, #59181, #66880, #45679, #8074, #87992, #53480, #56799, #37468, #42244, #5774, #63359, #9204, #22321, #85181, #80486, #82320, #730 ) ) ;
#82467 = CARTESIAN_POINT ( 'NONE',  ( 13.37577147909557773, 18.27418014603220442, 11.49999999999999645 ) ) ;
#82468 = ORIENTED_EDGE ( 'NONE', *, *, #30265, .F. ) ;
#82469 = CYLINDRICAL_SURFACE ( 'NONE', #56006, 19.30000000000000071 ) ;
#82470 = CARTESIAN_POINT ( 'NONE',  ( -42.55620429048337883, -23.47596703998600276, 11.44779298504227505 ) ) ;
#82471 = CARTESIAN_POINT ( 'NONE',  ( -54.62287095715005592, -23.48786465467240347, 11.44779295918255180 ) ) ;
#82472 = CARTESIAN_POINT ( 'NONE',  ( -45.58953762381671737, -25.00158670708909270, 2.256160236439164635 ) ) ;
#82473 = VERTEX_POINT ( 'NONE', #39882 ) ;
#82474 = ORIENTED_EDGE ( 'NONE', *, *, #45551, .T. ) ;
#82475 = EDGE_CURVE ( 'NONE', #76238, #23353, #78699, .T. ) ;
#82476 = CARTESIAN_POINT ( 'NONE',  ( -99.29687923781919778, -25.25133594952260552, 6.149712203147405631 ) ) ;
#82477 = CARTESIAN_POINT ( 'NONE',  ( -22.64140897529919272, -3.284158816904186651, 11.49999999999998934 ) ) ;
#82478 = CARTESIAN_POINT ( 'NONE',  ( -29.49551725617323328, -24.06847746220421769, -0.2315648265717072385 ) ) ;
#82479 = CARTESIAN_POINT ( 'NONE',  ( 8.794441374123232791, -19.68457759291379716, -1.500000000000002220 ) ) ;
#82480 = CARTESIAN_POINT ( 'NONE',  ( -113.6312462389022215, -23.48786465467241413, 11.44779295918254292 ) ) ;
#82481 = DIRECTION ( 'NONE',  ( -0.5656310827093756766, -2.995395837334948290E-15, 0.8246584009594636333 ) ) ;
#82482 = CARTESIAN_POINT ( 'NONE',  ( -22.13300264024875119, -4.194623038110560032, 11.49999999999999645 ) ) ;
#82483 = ORIENTED_EDGE ( 'NONE', *, *, #669, .T. ) ;
#82484 = CARTESIAN_POINT ( 'NONE',  ( 30.32108885906865936, -6.376774720514426953, 3.274824222184972822 ) ) ;
#82485 = CARTESIAN_POINT ( 'NONE',  ( 21.11370014442628218, -6.196533921283487345, 11.49999999999998934 ) ) ;
#82486 = CARTESIAN_POINT ( 'NONE',  ( -44.65453377568969273, -23.73791477778911130, 11.05961554403170943 ) ) ;
#82487 = CARTESIAN_POINT ( 'NONE',  ( -40.99321688279000853, -25.29087056432008040, 2.933756326319171936 ) ) ;
#82488 = VERTEX_POINT ( 'NONE', #85550 ) ;
#82489 = CARTESIAN_POINT ( 'NONE',  ( 22.81105451610979173, -1.682774720514426114, -18.46691820600746681 ) ) ;
#82490 = CARTESIAN_POINT ( 'NONE',  ( -90.58763137661625819, -24.63419186844611275, 9.035850630976923981 ) ) ;
#82491 = ORIENTED_EDGE ( 'NONE', *, *, #67647, .F. ) ;
#82492 = DIRECTION ( 'NONE',  ( 1.000000000000000000, 0.000000000000000000, 0.000000000000000000 ) ) ;
#82493 = VECTOR ( 'NONE', #77965, 1000.000000000000000 ) ;
#82494 = ORIENTED_EDGE ( 'NONE', *, *, #7505, .T. ) ;
#82495 = AXIS2_PLACEMENT_3D ( 'NONE', #1376, #71385, #31817 ) ;
#82496 = ORIENTED_EDGE ( 'NONE', *, *, #75431, .T. ) ;
#82497 = CARTESIAN_POINT ( 'NONE',  ( -110.9228709571500673, -23.47596703998600631, 11.44779298504227860 ) ) ;
#82498 = CARTESIAN_POINT ( 'NONE',  ( -72.52287095715007581, -23.47596703998600631, 11.44779298504228748 ) ) ;
#82499 = DIRECTION ( 'NONE',  ( 0.7512896232465892110, -0.000000000000000000, 0.6599726524652350657 ) ) ;
#82500 = CARTESIAN_POINT ( 'NONE',  ( -5.688044216684545518, -19.60349290560521140, -1.500000000000002220 ) ) ;
#82501 = VERTEX_POINT ( 'NONE', #31265 ) ;
#82502 = CARTESIAN_POINT ( 'NONE',  ( 8.971512145086506962, -2.028487854913504584, -6.500000000000000000 ) ) ;
#82503 = VECTOR ( 'NONE', #83264, 1000.000000000000114 ) ;
#82504 = DIRECTION ( 'NONE',  ( 0.1736481776669262511, 0.9848077530122087975, 0.000000000000000000 ) ) ;
#82505 = CARTESIAN_POINT ( 'NONE',  ( -105.6317619491183564, -24.15503026093913164, -0.2815557561904565298 ) ) ;
#82506 = CARTESIAN_POINT ( 'NONE',  ( -60.52287095715006160, -29.50250243563736774, 8.947779886222145151 ) ) ;
#82507 = ORIENTED_EDGE ( 'NONE', *, *, #30972, .F. ) ;
#82508 = DIRECTION ( 'NONE',  ( 0.000000000000000000, -0.8574929257125442073, -0.5144957554275266798 ) ) ;
#82509 = CARTESIAN_POINT ( 'NONE',  ( -28.13918514477506250, -25.26248066575644202, 8.204674103034470534 ) ) ;
#82510 = B_SPLINE_CURVE_WITH_KNOTS ( 'NONE', 3,
 ( #79180, #85802, #86295, #9171 ),
 .UNSPECIFIED., .F., .F.,
 ( 4, 4 ),
 ( 0.000000000000000000, 0.003057692307692316813 ),
 .UNSPECIFIED. ) ;
#82511 = EDGE_LOOP ( 'NONE', ( #46699, #79886, #78637, #47070 ) ) ;
#82512 = CIRCLE ( 'NONE', #67970, 28.96799999999999642 ) ;
#82513 = CARTESIAN_POINT ( 'NONE',  ( 1.081820405348005165, -20.78239343107542680, -1.500000000000002220 ) ) ;
#82514 = ORIENTED_EDGE ( 'NONE', *, *, #22731, .F. ) ;
#82516 = ORIENTED_EDGE ( 'NONE', *, *, #77506, .F. ) ;
#82515 = DIRECTION ( 'NONE',  ( -7.960204194457801640E-17, -1.000000000000000000, 1.571307496355802463E-16 ) ) ;
#82517 = EDGE_CURVE ( 'NONE', #45368, #42245, #85049, .T. ) ;
#82518 = CARTESIAN_POINT ( 'NONE',  ( -68.52287095715009002, -23.72773821059536914, 11.05748984161097503 ) ) ;
#82519 = CARTESIAN_POINT ( 'NONE',  ( -56.62287095715008434, -23.47596703998600276, 11.44779298504227683 ) ) ;
#82520 = ORIENTED_EDGE ( 'NONE', *, *, #88054, .T. ) ;
#82521 = EDGE_LOOP ( 'NONE', ( #44972, #53599, #46671, #32524 ) ) ;
#82522 = CARTESIAN_POINT ( 'NONE',  ( -78.62287095715005592, -23.96127896941632685, -0.6493128931037862595 ) ) ;
#82523 = AXIS2_PLACEMENT_3D ( 'NONE', #26581, #73254, #41300 ) ;
#82524 = CARTESIAN_POINT ( 'NONE',  ( -76.52287095715006160, -24.50321055353806088, 9.387540953477531147 ) ) ;
#82525 = CARTESIAN_POINT ( 'NONE',  ( -86.52287095715006160, -24.64898659630367916, 1.056161002820827921 ) ) ;
#82526 = CARTESIAN_POINT ( 'NONE',  ( -71.30164606794451743, -25.31201765511177726, 6.118441077956825680 ) ) ;
#82528 = VERTEX_POINT ( 'NONE', #62235 ) ;
#82527 = CARTESIAN_POINT ( 'NONE',  ( 13.47465251475156656, -17.59220275312388182, 11.49999999999999645 ) ) ;
#82529 = LINE ( 'NONE', #21120, #7407 ) ;
#82530 = CARTESIAN_POINT ( 'NONE',  ( 3.115699594417459473, -22.39947108414558485, 11.49999999999998934 ) ) ;
#82531 = EDGE_CURVE ( 'NONE', #43485, #10013, #17250, .T. ) ;
#82532 = EDGE_CURVE ( 'NONE', #81122, #95482, #4870, .T. ) ;
#82533 = ADVANCED_FACE ( 'NONE', ( #19540 ), #62953, .T. ) ;
#82535 = ORIENTED_EDGE ( 'NONE', *, *, #24587, .F. ) ;
#82534 = CARTESIAN_POINT ( 'NONE',  ( -119.6228709571500559, -29.50248528299804818, 1.056150453629045360 ) ) ;
#82536 = ORIENTED_EDGE ( 'NONE', *, *, #65712, .T. ) ;
#82537 = EDGE_CURVE ( 'NONE', #4993, #78876, #65256, .T. ) ;
#82538 = CARTESIAN_POINT ( 'NONE',  ( -41.32836283488544638, -2.682774720514426559, 39.26872235229541985 ) ) ;
#82539 = B_SPLINE_SURFACE_WITH_KNOTS ( 'NONE', 3, 3, ( 
 ( #24931, #8720, #33060, #17832 ),
 ( #77704, #47283, #7707, #92935 ),
 ( #23930, #38655, #56414, #64037 ),
 ( #87333, #63020, #47786, #54897 ),
 ( #9205, #31039, #8217, #70613 ),
 ( #55910, #71121, #48797, #78698 ),
 ( #78210, #40167, #39156, #85837 ) ),
 .UNSPECIFIED., .F., .F., .F.,
 ( 4, 3, 4 ),
 ( 4, 4 ),
 ( 0.7945040050992244751, 0.8970133687736503436, 0.9995227324480762121 ),
 ( 0.5096234996380107907, 0.5108715002186055010 ),
 .UNSPECIFIED. ) ;
#82540 = CARTESIAN_POINT ( 'NONE',  ( -57.56702574412142326, -23.48786465467241413, 11.44779295918254647 ) ) ;
#82541 = VERTEX_POINT ( 'NONE', #89065 ) ;
#82542 = CARTESIAN_POINT ( 'NONE',  ( -40.49165087243459737, -25.29345418843569959, 5.543942880831776776 ) ) ;
#82543 = CARTESIAN_POINT ( 'NONE',  ( 18.42719714020066846, 12.55551944762973626, -1.500000000000002220 ) ) ;
#82544 = CARTESIAN_POINT ( 'NONE',  ( 33.69795529655567634, 6.475225279485573360, 20.86760796525322093 ) ) ;
#82545 = EDGE_CURVE ( 'NONE', #69912, #85731, #41906, .T. ) ;
#82546 = ORIENTED_EDGE ( 'NONE', *, *, #92731, .T. ) ;
#82547 = DIRECTION ( 'NONE',  ( -0.000000000000000000, -1.000000000000000000, -0.000000000000000000 ) ) ;
#82548 = CARTESIAN_POINT ( 'NONE',  ( -4.531374827497722357, 4.263680106169587702, 1.700000000000006839 ) ) ;
#82549 = CARTESIAN_POINT ( 'NONE',  ( -27.33464509059021808, -24.58538552835475599, 1.660569724630185151 ) ) ;
#82550 = FACE_OUTER_BOUND ( 'NONE', #97740, .T. ) ;
#82551 = DIRECTION ( 'NONE',  ( -3.773278334453079618E-23, 0.9999999999976377785, 2.173523156925978705E-06 ) ) ;
#82552 = EDGE_CURVE ( 'NONE', #32470, #79556, #73880, .T. ) ;
#82553 = CARTESIAN_POINT ( 'NONE',  ( -12.10551386448753064, 15.32171617432465816, -1.500000000000002220 ) ) ;
#82554 = CARTESIAN_POINT ( 'NONE',  ( -3.867184171070207288, -21.11305558764578194, -1.500000000000002220 ) ) ;
#82555 = CARTESIAN_POINT ( 'NONE',  ( -2.750773227259631692, -6.376774720514413630, 19.84584863393302001 ) ) ;
#82556 = PLANE ( 'NONE',  #62684 ) ;
#82558 = B_SPLINE_CURVE_WITH_KNOTS ( 'NONE', 3,
 ( #91140, #66836, #66339, #59209, #21615, #74426 ),
 .UNSPECIFIED., .F., .F.,
 ( 4, 2, 4 ),
 ( 1.570755371633679342E-05, 0.001396183895866085801, 0.002776660238015834711 ),
 .UNSPECIFIED. ) ;
#82557 = FACE_OUTER_BOUND ( 'NONE', #57709, .T. ) ;
#82559 = CARTESIAN_POINT ( 'NONE',  ( -18.67006117854901959, 13.05921059288911934, -1.500000000000002220 ) ) ;
#82560 = ADVANCED_FACE ( 'NONE', ( #73834 ), #47551, .T. ) ;
#82561 = APPROVAL_STATUS ( 'not_yet_approved' ) ;
#82562 = CARTESIAN_POINT ( 'NONE',  ( -96.62356415693166412, -24.66019654487199375, 8.947790411086115725 ) ) ;
#82563 = CARTESIAN_POINT ( 'NONE',  ( -95.52287095715006160, -29.50250243563736774, 8.947779886222138046 ) ) ;
#82564 = CARTESIAN_POINT ( 'NONE',  ( 11.47056939498152950, -16.38825109899074661, 11.49999999999999645 ) ) ;
#82565 = CARTESIAN_POINT ( 'NONE',  ( -50.52287095715006160, -25.00158670708909270, 2.256160236439166411 ) ) ;
#82566 = VECTOR ( 'NONE', #71276, 1000.000000000000227 ) ;
#82567 = CARTESIAN_POINT ( 'NONE',  ( -74.50328731481324951, -24.35071581493544102, 9.817618358456019934 ) ) ;
#82568 = CARTESIAN_POINT ( 'NONE',  ( 30.93860345374796594, -6.475225279485573360, 19.84760796525321780 ) ) ;
#82569 = VERTEX_POINT ( 'NONE', #39133 ) ;
#82570 = FACE_OUTER_BOUND ( 'NONE', #93627, .T. ) ;
#82571 = CARTESIAN_POINT ( 'NONE',  ( -65.52287095715000476, -24.83620972994591369, 8.398175272781367440 ) ) ;
#82572 = EDGE_CURVE ( 'NONE', #90098, #20858, #93413, .T. ) ;
#82573 = CARTESIAN_POINT ( 'NONE',  ( 10.00111611332133421, -19.26892646806700071, -1.500000000000002220 ) ) ;
#82574 = CARTESIAN_POINT ( 'NONE',  ( -66.62287095715005592, -24.64898659630367916, 1.056161002820824368 ) ) ;
#82575 = AXIS2_PLACEMENT_3D ( 'NONE', #33985, #72554, #73059 ) ;
#82576 = CARTESIAN_POINT ( 'NONE',  ( -17.32436372870746055, -8.985247798433253053, -1.500000000000002220 ) ) ;
#82577 = LINE ( 'NONE', #14560, #45864 ) ;
#82578 = EDGE_CURVE ( 'NONE', #50194, #46174, #27869, .T. ) ;
#82579 = EDGE_CURVE ( 'NONE', #79632, #77615, #37571, .T. ) ;
#82581 = ORIENTED_EDGE ( 'NONE', *, *, #34657, .T. ) ;
#82580 = CIRCLE ( 'NONE', #71216, 3.979149600822063704 ) ;
#82582 = SECURITY_CLASSIFICATION_LEVEL ( 'unclassified' ) ;
#82583 = VECTOR ( 'NONE', #36936, 1000.000000000000114 ) ;
#82585 = CARTESIAN_POINT ( 'NONE',  ( -91.58383516866236107, -24.66019654487199730, 8.947790411086115725 ) ) ;
#82584 = B_SPLINE_CURVE_WITH_KNOTS ( 'NONE', 3,
 ( #49718, #33974, #12122, #97374 ),
 .UNSPECIFIED., .F., .F.,
 ( 4, 4 ),
 ( 0.000000000000000000, 0.0004038461538460880185 ),
 .UNSPECIFIED. ) ;
#82586 = CARTESIAN_POINT ( 'NONE',  ( -104.6228709571500559, -23.48786465467241413, 11.44779295918254114 ) ) ;
#82587 = CARTESIAN_POINT ( 'NONE',  ( 13.99439195134931069, 14.96789054323355828, 11.49999999999999645 ) ) ;
#82588 = FACE_OUTER_BOUND ( 'NONE', #28266, .T. ) ;
#82589 = CARTESIAN_POINT ( 'NONE',  ( -2.768609665556983845, -5.965225279485594001, -29.41086200512614823 ) ) ;
#82590 = VECTOR ( 'NONE', #46843, 1000.000000000000114 ) ;
#82591 = ORIENTED_EDGE ( 'NONE', *, *, #80632, .T. ) ;
#82592 = FACE_BOUND ( 'NONE', #43540, .T. ) ;
#82593 = CARTESIAN_POINT ( 'NONE',  ( -39.44774024104455634, -25.28892609849237161, 4.157779804617712571 ) ) ;
#82594 = CARTESIAN_POINT ( 'NONE',  ( -19.80875734969026425, 0.3587747205144265483, 31.02402280011862246 ) ) ;
#82595 = CARTESIAN_POINT ( 'NONE',  ( -123.5228709571500190, -24.33927499327855415, 9.819080762295801179 ) ) ;
#82596 = ORIENTED_EDGE ( 'NONE', *, *, #61054, .F. ) ;
#82597 = CARTESIAN_POINT ( 'NONE',  ( -61.62287095715004881, -29.50250786944525672, 11.44777988621623876 ) ) ;
#82598 = CARTESIAN_POINT ( 'NONE',  ( -19.45891602060003578, 12.32625358835968576, 11.49999999999999645 ) ) ;
#82599 = CARTESIAN_POINT ( 'NONE',  ( 4.306090731860143350, 22.38281141545218844, -1.500000000000002220 ) ) ;
#82600 = CARTESIAN_POINT ( 'NONE',  ( 3.128267882468583228, -6.376774720514424288, 21.08409277973916218 ) ) ;
#82601 = LINE ( 'NONE', #20194, #96569 ) ;
#82602 = CARTESIAN_POINT ( 'NONE',  ( -59.80072539165945500, -25.13069340115295702, 2.947789388436138580 ) ) ;
#82603 = CARTESIAN_POINT ( 'NONE',  ( -108.8968792378192063, -25.15277794460069316, 6.986250878905963191 ) ) ;
#82604 = CARTESIAN_POINT ( 'NONE',  ( -110.5923969822278963, -24.15503026093913519, -0.2815557561904549755 ) ) ;
#82605 = CARTESIAN_POINT ( 'NONE',  ( 9.607415760296678542, -19.69187540195887465, 11.49999999999998934 ) ) ;
#82606 = DIRECTION ( 'NONE',  ( -0.000000000000000000, 1.000000000000000000, -0.000000000000000000 ) ) ;
#82607 = DIRECTION ( 'NONE',  ( 0.000000000000000000, -0.000000000000000000, -1.000000000000000000 ) ) ;
#82608 = CARTESIAN_POINT ( 'NONE',  ( -94.62287095715005592, -23.48786465467241769, 11.44779295918254114 ) ) ;
#82609 = DIRECTION ( 'NONE',  ( 1.000000000000000000, -0.000000000000000000, 0.000000000000000000 ) ) ;
#82610 = VERTEX_POINT ( 'NONE', #21030 ) ;
#82611 = CARTESIAN_POINT ( 'NONE',  ( 9.418145840992488971, -18.15903486995133065, -1.500000000000002220 ) ) ;
#82612 = ORIENTED_EDGE ( 'NONE', *, *, #45769, .T. ) ;
#82613 = ORIENTED_EDGE ( 'NONE', *, *, #72752, .F. ) ;
#82614 = ORIENTED_EDGE ( 'NONE', *, *, #70217, .T. ) ;
#82615 = ORIENTED_EDGE ( 'NONE', *, *, #48517, .T. ) ;
#82616 = CARTESIAN_POINT ( 'NONE',  ( -22.90524134523018773, 2.401388714834002069, -1.500000000000002220 ) ) ;
#82617 = FACE_OUTER_BOUND ( 'NONE', #63849, .T. ) ;
#82618 = CARTESIAN_POINT ( 'NONE',  ( -2.479824388263708990, 20.08073137130260122, -1.500000000000002220 ) ) ;
#82619 = EDGE_LOOP ( 'NONE', ( #41614, #39521, #95317, #80123 ) ) ;
#82620 = DIRECTION ( 'NONE',  ( 0.000000000000000000, -2.173523156925980399E-06, 0.9999999999976378895 ) ) ;
#82621 = CARTESIAN_POINT ( 'NONE',  ( -46.55620429048340014, -24.64898659630528854, 1.056161002820822370 ) ) ;
#82622 = DIRECTION ( 'NONE',  ( -3.773278334453079618E-23, 0.9999999999976377785, 2.173523156925979975E-06 ) ) ;
#82623 = DIRECTION ( 'NONE',  ( -1.000000000000000000, 0.000000000000000000, 0.000000000000000000 ) ) ;
#82625 = ORIENTED_EDGE ( 'NONE', *, *, #43491, .T. ) ;
#82624 = CARTESIAN_POINT ( 'NONE',  ( 19.99082695160776169, -7.785253749782737209, 11.49999999999999645 ) ) ;
#82626 = DIRECTION ( 'NONE',  ( 0.000000000000000000, -0.9999999999976377785, -2.173523156925979975E-06 ) ) ;
#82627 = ORIENTED_EDGE ( 'NONE', *, *, #28732, .T. ) ;
#82628 = CARTESIAN_POINT ( 'NONE',  ( 18.07686251855496096, -12.98574554580779861, -1.500000000000002220 ) ) ;
#82629 = CARTESIAN_POINT ( 'NONE',  ( 15.29587703590233971, -13.95322596517325664, -1.500000000000002220 ) ) ;
#82630 = VECTOR ( 'NONE', #63367, 1000.000000000000000 ) ;
#82631 = ORIENTED_EDGE ( 'NONE', *, *, #35823, .T. ) ;
#82632 = CARTESIAN_POINT ( 'NONE',  ( -28.61148055913008292, -23.58117181907939752, -1.055554491438110309 ) ) ;
#82633 = EDGE_LOOP ( 'NONE', ( #75159, #7652, #34048, #66913 ) ) ;
#82634 = EDGE_CURVE ( 'NONE', #71054, #99388, #92019, .T. ) ;
#82635 = DIRECTION ( 'NONE',  ( 0.000000000000000000, 1.000000000000000000, 0.000000000000000000 ) ) ;
#82636 = ORIENTED_EDGE ( 'NONE', *, *, #27938, .T. ) ;
#82637 = EDGE_CURVE ( 'NONE', #3013, #4528, #22018, .T. ) ;
#82638 = CARTESIAN_POINT ( 'NONE',  ( -20.37482282770194075, 4.769447832466558346, -1.500000000000002220 ) ) ;
#82639 = CARTESIAN_POINT ( 'NONE',  ( 1.740910633133015972, 21.82039641801506846, 11.49999999999999645 ) ) ;
#82640 = EDGE_CURVE ( 'NONE', #26990, #36206, #13418, .T. ) ;
#82641 = FACE_OUTER_BOUND ( 'NONE', #74241, .T. ) ;
#82642 = CARTESIAN_POINT ( 'NONE',  ( -20.59131556071872282, -9.131246169528550283, 11.49999999999998934 ) ) ;
#82643 = AXIS2_PLACEMENT_3D ( 'NONE', #6774, #31108, #47348 ) ;
#82644 = EDGE_CURVE ( 'NONE', #65974, #78100, #30210, .T. ) ;
#82645 = CARTESIAN_POINT ( 'NONE',  ( 11.42219733811748306, 17.55150860717643724, 11.49999999999998934 ) ) ;
#82646 = CARTESIAN_POINT ( 'NONE',  ( 5.993553214355093139, -5.876774720514417183, 20.20316077874593930 ) ) ;
#82647 = EDGE_CURVE ( 'NONE', #28343, #79556, #43887, .T. ) ;
#82648 = CARTESIAN_POINT ( 'NONE',  ( -119.5547922413071689, -24.15620529776629510, 10.23563542870659582 ) ) ;
#82649 = DIRECTION ( 'NONE',  ( 0.000000000000000000, 0.9999999999976377785, 2.173523156925979975E-06 ) ) ;
#82650 = EDGE_LOOP ( 'NONE', ( #98, #1735, #39226, #51975 ) ) ;
#82651 = VECTOR ( 'NONE', #19726, 1000.000000000000114 ) ;
#82652 = VERTEX_POINT ( 'NONE', #46758 ) ;
#82653 = VECTOR ( 'NONE', #3755, 1000.000000000000000 ) ;
#82654 = EDGE_LOOP ( 'NONE', ( #46283, #78237, #4933, #21388 ) ) ;
#82655 = CARTESIAN_POINT ( 'NONE',  ( -66.55943415735386282, -23.73766607897669800, -1.055555164236460897 ) ) ;
#82656 = AXIS2_PLACEMENT_3D ( 'NONE', #14647, #90782, #7539 ) ;
#82657 = CARTESIAN_POINT ( 'NONE',  ( 20.36625868517733196, 6.724766957447481097, -1.500000000000002220 ) ) ;
#82658 = DIRECTION ( 'NONE',  ( -0.000000000000000000, 2.173523156925979552E-06, -0.9999999999976378895 ) ) ;
#82659 = ORIENTED_EDGE ( 'NONE', *, *, #28466, .F. ) ;
#82660 = CARTESIAN_POINT ( 'NONE',  ( -15.55823947972799282, -14.28038451723262270, 11.49999999999998934 ) ) ;
#82661 = CARTESIAN_POINT ( 'NONE',  ( 11.16000000000000014, -9.652339641703484574, -1.621096496867199033 ) ) ;
#82662 = CARTESIAN_POINT ( 'NONE',  ( -118.6228709571500701, -24.65952944569305316, 1.056160979905706565 ) ) ;
#82663 = CARTESIAN_POINT ( 'NONE',  ( -100.5228709571500332, -24.63287334234179227, 0.9662140553045398539 ) ) ;
#82664 = DIRECTION ( 'NONE',  ( 0.06975647374412546897, 0.9975640502598241977, 0.000000000000000000 ) ) ;
#82665 = CARTESIAN_POINT ( 'NONE',  ( -1.222978892338334012, -5.876774720514411854, 19.56655654527324373 ) ) ;
#82666 = CARTESIAN_POINT ( 'NONE',  ( -15.83042281971428977, -15.45127431894796466, -1.500000000000002220 ) ) ;
#82667 = CARTESIAN_POINT ( 'NONE',  ( 0.000000000000000000, -2.056774720514426669, 0.000000000000000000 ) ) ;
#82668 = ADVANCED_FACE ( 'NONE', ( #54876 ), #47261, .F. ) ;
#82669 = PLANE ( 'NONE',  #35224 ) ;
#82670 = CARTESIAN_POINT ( 'NONE',  ( -34.52287095715006160, -23.47593901973090169, -1.443836447538997314 ) ) ;
#82671 = FACE_OUTER_BOUND ( 'NONE', #13071, .T. ) ;
#82672 = CARTESIAN_POINT ( 'NONE',  ( -110.9909297185884327, -29.50249817218807635, 6.986241424688308221 ) ) ;
#82673 = EDGE_CURVE ( 'NONE', #25591, #40969, #5814, .T. ) ;
#82674 = CARTESIAN_POINT ( 'NONE',  ( -5.977879402576776968, -18.46583800616800630, 11.49999999999998934 ) ) ;
#82675 = CARTESIAN_POINT ( 'NONE',  ( 8.224165413489119558, 19.69228431130148493, 11.49999999999998934 ) ) ;
#82676 = CARTESIAN_POINT ( 'NONE',  ( 32.25249349869194759, 1.684774720514423674, -12.65342752644895263 ) ) ;
#82677 = CARTESIAN_POINT ( 'NONE',  ( -52.62287095715005592, -23.48783264082478794, -1.443836473390070596 ) ) ;
#82678 = CARTESIAN_POINT ( 'NONE',  ( -113.5228709571500616, -29.50248528299804818, 1.056150453629043584 ) ) ;
#82679 = FACE_OUTER_BOUND ( 'NONE', #18002, .T. ) ;
#82680 = CARTESIAN_POINT ( 'NONE',  ( -2.075279548881721947, -22.52154899835045043, -1.500000000000002220 ) ) ;
#82681 = ORIENTED_EDGE ( 'NONE', *, *, #52411, .F. ) ;
#82682 = CARTESIAN_POINT ( 'NONE',  ( 282.9764569301858046, -3.316774720514426900, 20.79159422840526616 ) ) ;
#82683 = CARTESIAN_POINT ( 'NONE',  ( -79.59201494684876366, -24.15543982623907127, -0.2315651400026654261 ) ) ;
#82684 = CARTESIAN_POINT ( 'NONE',  ( 4.927431051831622000, -19.18327824014073357, 11.49999999999999645 ) ) ;
#82685 = CARTESIAN_POINT ( 'NONE',  ( -0.4362980769230789257, -6.376774720514411854, 19.46153846153846345 ) ) ;
#82686 = DIRECTION ( 'NONE',  ( -3.773278334453079030E-23, 0.9999999999976377785, 2.173523156925979128E-06 ) ) ;
#82687 = ORIENTED_EDGE ( 'NONE', *, *, #82410, .F. ) ;
#82688 = CARTESIAN_POINT ( 'NONE',  ( -68.52287095715006160, -24.66019654487199730, 8.947790411086124607 ) ) ;
#82689 = CARTESIAN_POINT ( 'NONE',  ( -29.22648335530837471, -25.26026456907465345, 2.413925847313246109 ) ) ;
#82690 = DIRECTION ( 'NONE',  ( 0.9903949459893287566, 0.09776975748869010108, -0.09776975748868974025 ) ) ;
#82691 = CARTESIAN_POINT ( 'NONE',  ( 15.46703529437019853, -15.08741104398349187, -1.500000000000002220 ) ) ;
#82692 = CARTESIAN_POINT ( 'NONE',  ( -26.33488822642538452, -24.88201932036028552, 6.524121876823151034 ) ) ;
#82693 = CARTESIAN_POINT ( 'NONE',  ( 15.46825748771582631, 11.69065726450791409, -1.500000000000002220 ) ) ;
#82694 = FACE_OUTER_BOUND ( 'NONE', #15488, .T. ) ;
#82696 = CARTESIAN_POINT ( 'NONE',  ( -129.5228709571501042, -23.95044443724992789, 10.65354141964649237 ) ) ;
#82695 = B_SPLINE_CURVE_WITH_KNOTS ( 'NONE', 3,
 ( #58637, #57158, #65282, #50521, #88096, #74353 ),
 .UNSPECIFIED., .F., .F.,
 ( 4, 2, 4 ),
 ( 6.384118678617110714E-06, 0.001386860460828380623, 0.002767336802978144061 ),
 .UNSPECIFIED. ) ;
#82697 = ADVANCED_FACE ( 'NONE', ( #8194 ), #36772, .F. ) ;
#82698 = CARTESIAN_POINT ( 'NONE',  ( 12.93213199337649044, -14.99640713134888692, 11.49999999999998934 ) ) ;
#82699 = VERTEX_POINT ( 'NONE', #37271 ) ;
#82700 = B_SPLINE_CURVE_WITH_KNOTS ( 'NONE', 3,
 ( #73810, #4311, #7283, #85918 ),
 .UNSPECIFIED., .F., .F.,
 ( 4, 4 ),
 ( 0.000000000000000000, 0.0002088004239042353695 ),
 .UNSPECIFIED. ) ;
#82701 = CARTESIAN_POINT ( 'NONE',  ( -19.34540493331696354, 6.066486871809979142, 11.49999999999999645 ) ) ;
#82702 = CARTESIAN_POINT ( 'NONE',  ( 13.59451591917074431, 3.316774720514426456, -28.23515841827053308 ) ) ;
#82704 = EDGE_CURVE ( 'NONE', #18629, #24103, #62487, .T. ) ;
#82703 = VECTOR ( 'NONE', #42961, 1000.000000000000114 ) ;
#82705 = CARTESIAN_POINT ( 'NONE',  ( -46.58953762381672448, -24.66019654487199020, 8.947790411086131712 ) ) ;
#82706 = EDGE_LOOP ( 'NONE', ( #27629, #12769, #10922, #71908 ) ) ;
#82707 = CARTESIAN_POINT ( 'NONE',  ( -102.5474479301096693, -24.66019654487200086, 8.947790411086115725 ) ) ;
#82708 = CARTESIAN_POINT ( 'NONE',  ( 31.63608488009069575, 3.478648800329905644, 27.34773273846989738 ) ) ;
#82709 = CARTESIAN_POINT ( 'NONE',  ( -44.62287095715004170, -23.73907113216990439, -1.053371485793233697 ) ) ;
#82710 = FACE_OUTER_BOUND ( 'NONE', #80936, .T. ) ;
#82711 = LINE ( 'NONE', #12696, #94876 ) ;
#82712 = CARTESIAN_POINT ( 'NONE',  ( -5.826506878040391690, 19.21762618028343184, 11.49999999999998934 ) ) ;
#82713 = CARTESIAN_POINT ( 'NONE',  ( -79.58953762381673869, -23.47593901973091235, -1.443836447539004642 ) ) ;
#82714 = VERTEX_POINT ( 'NONE', #90058 ) ;
#82715 = AXIS2_PLACEMENT_3D ( 'NONE', #31884, #62856, #24265 ) ;
#82716 = CARTESIAN_POINT ( 'NONE',  ( 0.7049041324096299022, -22.85584899170066109, 11.49999999999999645 ) ) ;
#82717 = CARTESIAN_POINT ( 'NONE',  ( -106.2228709571500644, -23.47593901973090524, -1.443836447538996648 ) ) ;
#82718 = DIRECTION ( 'NONE',  ( 0.000000000000000000, 0.000000000000000000, -1.000000000000000000 ) ) ;
#82719 = DIRECTION ( 'NONE',  ( 0.7071067811865507924, 0.000000000000000000, 0.7071067811865442421 ) ) ;
#82720 = AXIS2_PLACEMENT_3D ( 'NONE', #56672, #96221, #26705 ) ;
#82721 = CARTESIAN_POINT ( 'NONE',  ( -25.92875734969025814, -6.376774720514426953, 26.43402280011862615 ) ) ;
#82722 = AXIS2_PLACEMENT_3D ( 'NONE', #67467, #98393, #75552 ) ;
#82723 = CARTESIAN_POINT ( 'NONE',  ( -90.52287095715009002, -23.48783264082477373, -1.443836473390088582 ) ) ;
#82724 = CARTESIAN_POINT ( 'NONE',  ( -22.40390758644239710, -1.035154934579901820, 11.49999999999999645 ) ) ;
#82725 = CARTESIAN_POINT ( 'NONE',  ( -87.52287095715006160, -29.50250786944525672, 11.44777988621623344 ) ) ;
#82726 = VERTEX_POINT ( 'NONE', #36278 ) ;
#82727 = CARTESIAN_POINT ( 'NONE',  ( 2.178911383790714584, -20.24183328246387958, 11.49999999999998934 ) ) ;
#82728 = ORIENTED_EDGE ( 'NONE', *, *, #67363, .F. ) ;
#82729 = CARTESIAN_POINT ( 'NONE',  ( -3.094460115123966570, -22.75893099265358188, -1.500000000000002220 ) ) ;
#82731 = DIRECTION ( 'NONE',  ( 0.000000000000000000, 0.9999999999976377785, 2.173523156925979128E-06 ) ) ;
#82730 = B_SPLINE_CURVE_WITH_KNOTS ( 'NONE', 3,
 ( #63497, #48765, #72597, #79691, #94418, #42159 ),
 .UNSPECIFIED., .F., .F.,
 ( 4, 2, 4 ),
 ( 3.258661033901071854E-05, 0.002748063894075334409, 0.005463541177811657469 ),
 .UNSPECIFIED. ) ;
#82732 = ORIENTED_EDGE ( 'NONE', *, *, #41328, .F. ) ;
#82733 = CARTESIAN_POINT ( 'NONE',  ( -108.5228709571500616, -23.73934037231757443, 11.05740245334328087 ) ) ;
#82734 = CARTESIAN_POINT ( 'NONE',  ( -94.62287095715005592, -23.48783264082478794, -1.443836473390063491 ) ) ;
#82735 = LINE ( 'NONE', #13217, #52906 ) ;
#82737 = EDGE_LOOP ( 'NONE', ( #80488, #4141, #30340, #6965 ) ) ;
#82736 = CARTESIAN_POINT ( 'NONE',  ( -4.916304867406160461, -20.68799595667769964, 11.49999999999999645 ) ) ;
#82738 = EDGE_LOOP ( 'NONE', ( #82119, #3719, #15124, #67428 ) ) ;
#82739 = CARTESIAN_POINT ( 'NONE',  ( -10.57539506955483333, 19.50334513348995813, -1.500000000000002220 ) ) ;
#82740 = CARTESIAN_POINT ( 'NONE',  ( -18.12278953325389708, -9.833843834435361586, 11.49999999999998934 ) ) ;
#82741 = EDGE_LOOP ( 'NONE', ( #29784, #17256, #5009, #96845 ) ) ;
#82742 = ORIENTED_EDGE ( 'NONE', *, *, #42788, .F. ) ;
#82743 = CARTESIAN_POINT ( 'NONE',  ( 5.949073730962466833, 5.965225279485572685, -27.94053387008862188 ) ) ;
#82744 = CARTESIAN_POINT ( 'NONE',  ( 3.050049012211247579, -5.876774720514426065, 21.53019692557248632 ) ) ;
#82745 = ORIENTED_EDGE ( 'NONE', *, *, #16778, .T. ) ;
#82747 = ORIENTED_EDGE ( 'NONE', *, *, #18183, .T. ) ;
#82746 = ADVANCED_FACE ( 'NONE', ( #12919 ), #80208, .T. ) ;
#82748 = ORIENTED_EDGE ( 'NONE', *, *, #69276, .T. ) ;
#82749 = CARTESIAN_POINT ( 'NONE',  ( -124.6623382465025145, -25.28334050553294432, 4.245309122437063820 ) ) ;
#82750 = CARTESIAN_POINT ( 'NONE',  ( -28.62375899609942564, -24.50739853925337641, 8.947790409070465856 ) ) ;
#82751 = CARTESIAN_POINT ( 'NONE',  ( 15.50761710536979798, -3.593805972274602301, -28.23039328495928046 ) ) ;
#82752 = CARTESIAN_POINT ( 'NONE',  ( 20.29938135082171158, -4.300543036493735372, -1.500000000000002220 ) ) ;
#82753 = CARTESIAN_POINT ( 'NONE',  ( -8.443908442993951269, 20.02826104456839218, 11.49999999999999645 ) ) ;
#82754 = ORIENTED_EDGE ( 'NONE', *, *, #84148, .F. ) ;
#82755 = EDGE_CURVE ( 'NONE', #5079, #68195, #33534, .T. ) ;
#82756 = CARTESIAN_POINT ( 'NONE',  ( -100.4849985857635630, -25.18518816741224953, 3.295769164467318824 ) ) ;
#82757 = CARTESIAN_POINT ( 'NONE',  ( -34.52287095715006160, -23.47596703998600631, 11.44779298504229459 ) ) ;
#82758 = CARTESIAN_POINT ( 'NONE',  ( -115.6263010057922429, -24.52300882791528736, 0.6510814631126266017 ) ) ;
#82759 = CARTESIAN_POINT ( 'NONE',  ( -22.40390758644239710, -1.035154934579901820, 11.49999999999998934 ) ) ;
#82760 = EDGE_CURVE ( 'NONE', #12714, #98742, #17812, .T. ) ;
#82761 = CARTESIAN_POINT ( 'NONE',  ( -51.08807254026520184, -25.26334689473844364, 4.449946248032227381 ) ) ;
#82762 = ORIENTED_EDGE ( 'NONE', *, *, #59411, .F. ) ;
#82763 = LINE ( 'NONE', #74163, #90620 ) ;
#82764 = CARTESIAN_POINT ( 'NONE',  ( 3.300000000000006040, 0.000000000000000000, 0.000000000000000000 ) ) ;
#82765 = EDGE_CURVE ( 'NONE', #71418, #20569, #43194, .T. ) ;
#82766 = VERTEX_POINT ( 'NONE', #56892 ) ;
#82767 = EDGE_CURVE ( 'NONE', #79746, #45709, #56165, .T. ) ;
#82768 = EDGE_LOOP ( 'NONE', ( #4262, #19, #87786, #78820 ) ) ;
#82769 = VECTOR ( 'NONE', #38837, 1000.000000000000000 ) ;
#82770 = CARTESIAN_POINT ( 'NONE',  ( 9.278253834636469577, -6.376774720514426953, 21.48128695274316158 ) ) ;
#82771 = ORIENTED_EDGE ( 'NONE', *, *, #45308, .F. ) ;
#82772 = CARTESIAN_POINT ( 'NONE',  ( 7.794017451908327843, -19.83292067980804774, -1.500000000000002220 ) ) ;
#82773 = ORIENTED_EDGE ( 'NONE', *, *, #98023, .F. ) ;
#82774 = CARTESIAN_POINT ( 'NONE',  ( 6.660000000000001030, -10.15233964170348457, 0.003711184059992174607 ) ) ;
#82775 = CARTESIAN_POINT ( 'NONE',  ( 13.92123049006271707, -16.85212209846622855, 11.49999999999998934 ) ) ;
#82776 = LINE ( 'NONE', #6152, #69199 ) ;
#82777 = CARTESIAN_POINT ( 'NONE',  ( 21.16149768242404861, -8.233860041645145955, -1.500000000000002220 ) ) ;
#82778 = CARTESIAN_POINT ( 'NONE',  ( -41.24137195392557942, -25.28892493134095432, 3.620793846790061554 ) ) ;
#82779 = CARTESIAN_POINT ( 'NONE',  ( 8.667033081675079131, -3.316774720514425567, -27.07192531862967400 ) ) ;
#82780 = CARTESIAN_POINT ( 'NONE',  ( -3.149188516569510377, 21.71089317892358395, -1.500000000000002220 ) ) ;
#82781 = LINE ( 'NONE', #13263, #81954 ) ;
#82782 = ORIENTED_EDGE ( 'NONE', *, *, #54940, .F. ) ;
#82783 = CARTESIAN_POINT ( 'NONE',  ( -40.33347935548481189, -25.29368123691946479, 5.540415114266751040 ) ) ;
#82784 = ADVANCED_FACE ( 'NONE', ( #93920 ), #1104, .F. ) ;
#82785 = VERTEX_POINT ( 'NONE', #10701 ) ;
#82786 = PLANE ( 'NONE',  #14072 ) ;
#82787 = CIRCLE ( 'NONE', #39044, 3.349999999999998757 ) ;
#82788 = LINE ( 'NONE', #7159, #52237 ) ;
#82789 = VECTOR ( 'NONE', #82499, 1000.000000000000227 ) ;
#82790 = CARTESIAN_POINT ( 'NONE',  ( -10.26558916711599778, -22.69538807860070406, 0.04347934593173622547 ) ) ;
#82791 = CARTESIAN_POINT ( 'NONE',  ( -20.53569570583907122, -5.550916044964551155, -1.500000000000002220 ) ) ;
#82792 = CARTESIAN_POINT ( 'NONE',  ( -112.5934586508881523, -23.73766607897671577, -1.055555164236427590 ) ) ;
#82793 = CARTESIAN_POINT ( 'NONE',  ( 4.444543648262985869, 12.92677669529668627, 2.100000000000000089 ) ) ;
#82794 = CARTESIAN_POINT ( 'NONE',  ( -85.51575671001552337, -23.85016227208579664, -0.8807180028928368598 ) ) ;
#82795 = CARTESIAN_POINT ( 'NONE',  ( -93.52287095715006160, -29.50247984919015209, -1.443849546365051806 ) ) ;
#82796 = FACE_OUTER_BOUND ( 'NONE', #80300, .T. ) ;
#82797 = ORIENTED_EDGE ( 'NONE', *, *, #43509, .T. ) ;
#82798 = CARTESIAN_POINT ( 'NONE',  ( -5.392953615240748455, 18.82278424538476713, 11.49999999999999645 ) ) ;
#82799 = CARTESIAN_POINT ( 'NONE',  ( -40.52287095715006870, -29.50250786944525672, 11.44777988621624232 ) ) ;
#82800 = CARTESIAN_POINT ( 'NONE',  ( -91.15361000704997707, -25.26877915520014639, 5.947789088310639904 ) ) ;
#82801 = ORIENTED_EDGE ( 'NONE', *, *, #83686, .T. ) ;
#82802 = LINE ( 'NONE', #90922, #92777 ) ;
#82803 = CARTESIAN_POINT ( 'NONE',  ( -100.8159136911362594, -25.03998861187190172, 7.529830385290721573 ) ) ;
#82804 = CARTESIAN_POINT ( 'NONE',  ( -27.70544111104076990, -24.65058036537550024, 8.251826706788236265 ) ) ;
#82805 = CARTESIAN_POINT ( 'NONE',  ( -50.13103505045899766, -25.12667166846206257, 7.080526547379527358 ) ) ;
#82806 = CARTESIAN_POINT ( 'NONE',  ( -17.00503767097633556, -9.977476526402845991, 11.49999999999998934 ) ) ;
#82807 = B_SPLINE_CURVE_WITH_KNOTS ( 'NONE', 3,
 ( #90634, #67310, #20617, #82519 ),
 .UNSPECIFIED., .F., .F.,
 ( 4, 4 ),
 ( 0.2589468163131236067, 0.2599475633538891883 ),
 .UNSPECIFIED. ) ;
#82808 = EDGE_LOOP ( 'NONE', ( #54039, #91854, #27142, #20722, #29573, #71525, #20984, #59530 ) ) ;
#82809 = CARTESIAN_POINT ( 'NONE',  ( 10.46399479596398052, 3.316774720514422903, -27.03001098546561209 ) ) ;
#82810 = CARTESIAN_POINT ( 'NONE',  ( -104.5228709571500758, -23.47596703998600631, 11.44779298504228215 ) ) ;
#82811 = DATE_AND_TIME ( #34661, #13311 ) ;
#82812 = ADVANCED_FACE ( 'NONE', ( #41663 ), #87825, .F. ) ;
#82813 = ORIENTED_EDGE ( 'NONE', *, *, #32939, .F. ) ;
#82814 = CARTESIAN_POINT ( 'NONE',  ( -54.52287095715009713, -24.33927499327855770, 9.819080762295813614 ) ) ;
#82815 = LINE ( 'NONE', #51888, #75009 ) ;
#82816 = CARTESIAN_POINT ( 'NONE',  ( -55.51141851980899844, -23.85016227208578954, -0.8807180028928371929 ) ) ;
#82817 = FACE_OUTER_BOUND ( 'NONE', #33582, .T. ) ;
#82818 = CARTESIAN_POINT ( 'NONE',  ( -45.52287095715006160, -24.99156044556202616, 7.747789690856173195 ) ) ;
#82819 = FACE_OUTER_BOUND ( 'NONE', #56092, .T. ) ;
#82820 = B_SPLINE_CURVE_WITH_KNOTS ( 'NONE', 3,
 ( #43776, #90439, #51385, #51890 ),
 .UNSPECIFIED., .F., .F.,
 ( 4, 4 ),
 ( 0.3200144389552843638, 0.3290208702273997865 ),
 .UNSPECIFIED. ) ;
#82821 = CARTESIAN_POINT ( 'NONE',  ( -120.5228709571500616, -23.47593901973090524, -1.443836447538996204 ) ) ;
#82822 = CARTESIAN_POINT ( 'NONE',  ( -14.92271332039470444, 13.28099397388983327, 11.49999999999998934 ) ) ;
#82823 = EDGE_CURVE ( 'NONE', #20070, #17632, #19419, .T. ) ;
#82824 = DIRECTION ( 'NONE',  ( -0.000000000000000000, 1.000000000000000000, -0.000000000000000000 ) ) ;
#82825 = CARTESIAN_POINT ( 'NONE',  ( -0.06124857980327405582, -22.25708900282751301, 9.349680052484377057 ) ) ;
#82826 = ORIENTED_EDGE ( 'NONE', *, *, #5788, .T. ) ;
#82827 = DIRECTION ( 'NONE',  ( 0.7071067811865507924, 0.000000000000000000, -0.7071067811865442421 ) ) ;
#82828 = CARTESIAN_POINT ( 'NONE',  ( 10.40220176116686979, -5.447062032237068863, -27.19353416079722763 ) ) ;
#82829 = CARTESIAN_POINT ( 'NONE',  ( -119.6284910101131942, -23.48783264082477018, -1.443836473390087916 ) ) ;
#82830 = LINE ( 'NONE', #83332, #2170 ) ;
#82831 = CARTESIAN_POINT ( 'NONE',  ( 0.3910256410256394144, -6.376774720514411854, 19.63681891025641235 ) ) ;
#82832 = CARTESIAN_POINT ( 'NONE',  ( -81.55862812813013818, -23.73766607897671221, -1.055555164236432919 ) ) ;
#82833 = AXIS2_PLACEMENT_3D ( 'NONE', #85932, #70208, #7295 ) ;
#82834 = CARTESIAN_POINT ( 'NONE',  ( -119.6228709571500559, -23.47593901973091235, -1.443836447538997536 ) ) ;
#82835 = APPROVAL ( #15799, 'UNSPECIFIED' ) ;
#82836 = CARTESIAN_POINT ( 'NONE',  ( -1.359251851468251449, -5.876774720514419847, 20.71116975788854120 ) ) ;
#82837 = ORIENTED_EDGE ( 'NONE', *, *, #6799, .T. ) ;
#82838 = CARTESIAN_POINT ( 'NONE',  ( -68.52287095715006160, -29.50247984919015209, -1.443849546365055359 ) ) ;
#82839 = CARTESIAN_POINT ( 'NONE',  ( -127.5556656467780812, -24.15543982623907837, -0.2315651400026539075 ) ) ;
#82840 = ORIENTED_EDGE ( 'NONE', *, *, #70640, .T. ) ;
#82841 = CARTESIAN_POINT ( 'NONE',  ( -18.13051092187696156, -9.059970205480309957, 11.49999999999998934 ) ) ;
#82842 = DIRECTION ( 'NONE',  ( -0.000000000000000000, 0.000000000000000000, 1.000000000000000000 ) ) ;
#82843 = CARTESIAN_POINT ( 'NONE',  ( -49.62287095715004881, -23.73907113216990794, -1.053371485793234807 ) ) ;
#82844 = CARTESIAN_POINT ( 'NONE',  ( -2.499999999999993339, 18.99999999999977618, 2.100000000000000089 ) ) ;
#82845 = ORIENTED_EDGE ( 'NONE', *, *, #48002, .T. ) ;
#82846 = PLANE ( 'NONE',  #90612 ) ;
#82847 = DIRECTION ( 'NONE',  ( 0.000000000000000000, 0.000000000000000000, 1.000000000000000000 ) ) ;
#82848 = AXIS2_PLACEMENT_3D ( 'NONE', #36014, #90806, #96424 ) ;
#82849 = CARTESIAN_POINT ( 'NONE',  ( 6.297820759360134524, 19.07352124001985771, -1.500000000000002220 ) ) ;
#82850 = CARTESIAN_POINT ( 'NONE',  ( -17.04133944854041616, 12.32129857345222845, 11.49999999999999645 ) ) ;
#82851 =( GEOMETRIC_REPRESENTATION_CONTEXT ( 3 ) GLOBAL_UNCERTAINTY_ASSIGNED_CONTEXT ( ( #20554 ) ) GLOBAL_UNIT_ASSIGNED_CONTEXT ( ( #50131, #26288, #89190 ) ) REPRESENTATION_CONTEXT ( 'NONE', 'WORKASPACE' ) );
#82852 = CARTESIAN_POINT ( 'NONE',  ( -28.87563289579386350, -25.03413959481116535, 6.908192424899269213 ) ) ;
#82853 = CARTESIAN_POINT ( 'NONE',  ( -111.6228709571500275, -24.33927499327855415, 9.819080762295820719 ) ) ;
#82854 = CARTESIAN_POINT ( 'NONE',  ( -21.42919730060085115, -5.301375089729956969, -1.500000000000002220 ) ) ;
#82855 = CARTESIAN_POINT ( 'NONE',  ( 20.32696876622996029, 2.630761579057304900, -1.500000000000002220 ) ) ;
#82856 = CARTESIAN_POINT ( 'NONE',  ( -39.44787993411948435, -25.31589142152604666, 4.218554769620590505 ) ) ;
#82857 = CARTESIAN_POINT ( 'NONE',  ( -59.62287095715004881, -24.64898659630367916, 1.056161002820822592 ) ) ;
#82858 = PLANE ( 'NONE',  #89796 ) ;
#82859 = EDGE_LOOP ( 'NONE', ( #27476, #18237, #3508, #30942 ) ) ;
#82860 = CARTESIAN_POINT ( 'NONE',  ( -29.49875734969025842, 5.965225279485572685, 17.86602280011862476 ) ) ;
#82861 = FACE_OUTER_BOUND ( 'NONE', #79898, .T. ) ;
#82862 = ORIENTED_EDGE ( 'NONE', *, *, #73571, .F. ) ;
#82863 = VERTEX_POINT ( 'NONE', #86815 ) ;
#82864 = CARTESIAN_POINT ( 'NONE',  ( 3.252401863874210264, 5.965225279485592225, -29.35688408629928858 ) ) ;
#82865 = CARTESIAN_POINT ( 'NONE',  ( -1.358974358974355257, -5.876774720514426953, 21.75000000000000711 ) ) ;
#82866 = CARTESIAN_POINT ( 'NONE',  ( -76.50398578030031160, -24.34968618360934300, 0.1864209137778858327 ) ) ;
#82867 = CARTESIAN_POINT ( 'NONE',  ( -15.40095275084150117, -13.70674696055758801, -1.500000000000002220 ) ) ;
#82868 = CARTESIAN_POINT ( 'NONE',  ( -21.57561264457377348, 0.06291308125064201673, 11.49999999999999645 ) ) ;
#82869 = ORIENTED_EDGE ( 'NONE', *, *, #36020, .T. ) ;
#82870 = CARTESIAN_POINT ( 'NONE',  ( -71.62287095715005592, -29.50250243563736774, 8.947779886222143375 ) ) ;
#82871 = CARTESIAN_POINT ( 'NONE',  ( -4.223504350552545361, -6.376774720514411854, 19.52341893546492813 ) ) ;
#82872 = CARTESIAN_POINT ( 'NONE',  ( -5.491053050139323766, 21.65304554001118120, 11.49999999999998934 ) ) ;
#82873 = B_SPLINE_CURVE_WITH_KNOTS ( 'NONE', 3,
 ( #95608, #66186, #89000, #4265 ),
 .UNSPECIFIED., .F., .F.,
 ( 4, 4 ),
 ( 0.000000000000000000, 9.999999999997510880E-05 ),
 .UNSPECIFIED. ) ;
#82874 = CARTESIAN_POINT ( 'NONE',  ( -79.60383831484530504, -25.12205723040236904, 6.693229097001963446 ) ) ;
#82875 = CARTESIAN_POINT ( 'NONE',  ( -61.62287095715004881, -24.64898659630528854, 1.056161002820822592 ) ) ;
#82876 = VERTEX_POINT ( 'NONE', #48267 ) ;
#82877 = DIRECTION ( 'NONE',  ( 0.9872275723272646575, 0.000000000000000000, 0.1593164160933058515 ) ) ;
#82878 = CARTESIAN_POINT ( 'NONE',  ( -96.55620429048339304, -23.48786465467241058, 11.44779295918254114 ) ) ;
#82879 = EDGE_CURVE ( 'NONE', #27297, #99233, #24411, .T. ) ;
#82880 = CARTESIAN_POINT ( 'NONE',  ( -19.94048968823238255, 6.179419890754223488, 11.49999999999998934 ) ) ;
#82881 = EDGE_CURVE ( 'NONE', #41589, #34094, #75127, .T. ) ;
#82882 = EDGE_LOOP ( 'NONE', ( #87621, #9376, #58300 ) ) ;
#82884 = VERTEX_POINT ( 'NONE', #57398 ) ;
#82883 = CARTESIAN_POINT ( 'NONE',  ( -86.54507443799202804, -24.51314013834314665, 0.6176544820404149538 ) ) ;
#82885 = ORIENTED_EDGE ( 'NONE', *, *, #2256, .T. ) ;
#82886 = CIRCLE ( 'NONE', #16460, 1.325999999999943446 ) ;
#82887 = CARTESIAN_POINT ( 'NONE',  ( -100.6015246471107218, -23.48786465467241413, 11.44779295918254469 ) ) ;
#82888 = CARTESIAN_POINT ( 'NONE',  ( 20.91448408463407205, 2.778442817847782020, -1.500000000000002220 ) ) ;
#82889 = VERTEX_POINT ( 'NONE', #94931 ) ;
#82890 = CARTESIAN_POINT ( 'NONE',  ( -122.9228709571500531, -23.47596703998600631, 11.44779298504227860 ) ) ;
#82891 = LINE ( 'NONE', #5277, #44986 ) ;
#82892 = CARTESIAN_POINT ( 'NONE',  ( -48.62287095715005592, -23.73934037231756733, 11.05740245334328975 ) ) ;
#82893 = CARTESIAN_POINT ( 'NONE',  ( -71.62287095715005592, -29.50248528299804818, 1.056150453629036701 ) ) ;
#82894 = CARTESIAN_POINT ( 'NONE',  ( 7.480769230769231726, -6.376774720514420736, 20.77403846153845635 ) ) ;
#82895 = CARTESIAN_POINT ( 'NONE',  ( -7.892909027492730267, -20.28523913882780505, -1.500000000000002220 ) ) ;
#82896 = CARTESIAN_POINT ( 'NONE',  ( -71.70379718938951896, -25.24674313106178403, 6.052014784346466669 ) ) ;
#82898 = VERTEX_POINT ( 'NONE', #32026 ) ;
#82897 = CARTESIAN_POINT ( 'NONE',  ( 21.78807519107708401, 4.755904613692067073, 11.49999999999999645 ) ) ;
#82899 = ADVANCED_FACE ( 'NONE', ( #24910 ), #33036, .F. ) ;
#82900 = DIRECTION ( 'NONE',  ( -3.773278334453079618E-23, 0.9999999999976377785, 2.173523156925979975E-06 ) ) ;
#82901 = CYLINDRICAL_SURFACE ( 'NONE', #45979, 2.249999999999998668 ) ;
#82902 = CYLINDRICAL_SURFACE ( 'NONE', #79706, 2.040000000000000036 ) ;
#82903 = ORIENTED_EDGE ( 'NONE', *, *, #24573, .T. ) ;
#82904 = ORIENTED_EDGE ( 'NONE', *, *, #77606, .T. ) ;
#82905 = VERTEX_POINT ( 'NONE', #79701 ) ;
#82906 = CARTESIAN_POINT ( 'NONE',  ( -75.52287095715006160, -24.92579138211020151, 1.929029949965663793 ) ) ;
#82907 = VECTOR ( 'NONE', #21535, 1000.000000000000114 ) ;
#82908 = DIRECTION ( 'NONE',  ( -1.000000000000000000, 0.000000000000000000, -0.000000000000000000 ) ) ;
#82909 = CARTESIAN_POINT ( 'NONE',  ( 29.71119274252842501, -4.341971045292455145, 27.93347042254709223 ) ) ;
#82910 = CARTESIAN_POINT ( 'NONE',  ( -49.12170187741904925, -25.28917234601119901, 4.199658634648916866 ) ) ;
#82911 = CARTESIAN_POINT ( 'NONE',  ( -7.246369895950522277, -17.95243785538732340, 11.49999999999998934 ) ) ;
#82912 = B_SPLINE_CURVE_WITH_KNOTS ( 'NONE', 3,
 ( #17811, #26427, #10196, #48773 ),
 .UNSPECIFIED., .F., .F.,
 ( 4, 4 ),
 ( 7.357964204579942986E-06, 0.001221264703421874901 ),
 .UNSPECIFIED. ) ;
#82913 = LINE ( 'NONE', #50485, #92738 ) ;
#82914 = ORIENTED_EDGE ( 'NONE', *, *, #78779, .F. ) ;
#82915 = CARTESIAN_POINT ( 'NONE',  ( 7.305494252837257285, 17.95555029072639286, 11.49999999999999645 ) ) ;
#82916 = CARTESIAN_POINT ( 'NONE',  ( 30.09341516180546350, 1.684774720514424562, -11.39311774897855756 ) ) ;
#82917 = ORIENTED_EDGE ( 'NONE', *, *, #22491, .T. ) ;
#82918 = FACE_OUTER_BOUND ( 'NONE', #14777, .T. ) ;
#82919 = CARTESIAN_POINT ( 'NONE',  ( 9.464509667910858681, 5.356774720513593380, -27.03659963401723942 ) ) ;
#82920 = PLANE ( 'NONE',  #72513 ) ;
#82921 = CARTESIAN_POINT ( 'NONE',  ( -87.62287095715004170, -23.47596703998600631, 11.44779298504227860 ) ) ;
#82922 = EDGE_CURVE ( 'NONE', #62936, #64433, #25419, .T. ) ;
#82923 = AXIS2_PLACEMENT_3D ( 'NONE', #12186, #20793, #91316 ) ;
#82924 = CARTESIAN_POINT ( 'NONE',  ( 9.307004028210867475, 17.29072351678862418, -1.500000000000002220 ) ) ;
#82925 = CARTESIAN_POINT ( 'NONE',  ( -116.5562042904833930, -24.65952944569305316, 1.056160979905706121 ) ) ;
#82927 = VERTEX_POINT ( 'NONE', #17302 ) ;
#82926 = LOCAL_TIME ( 0, 54, 15.00000000000000000, #35411 ) ;
#82928 = CARTESIAN_POINT ( 'NONE',  ( 20.98156868870745484, 4.911575462371418510, -1.500000000000002220 ) ) ;
#82929 = CARTESIAN_POINT ( 'NONE',  ( -33.50410096519379977, -23.96169478059712432, 10.65365249895719124 ) ) ;
#82930 = CARTESIAN_POINT ( 'NONE',  ( -116.2228709571501213, -23.47593901973090880, -1.443836447538996870 ) ) ;
#82931 = CARTESIAN_POINT ( 'NONE',  ( -50.52287095715009002, -24.82558206586149652, 1.605769216559628454 ) ) ;
#82932 = PLANE ( 'NONE',  #42329 ) ;
#82933 = CARTESIAN_POINT ( 'NONE',  ( -21.12268324108725892, 9.058254180033936009, -1.500000000000002220 ) ) ;
#82934 = ADVANCED_FACE ( 'NONE', ( #40654, #9186 ), #72110, .F. ) ;
#82935 = APPLICATION_PROTOCOL_DEFINITION ( 'international standard', 'config_control_design', 1994, #40771 ) ;
#82936 = LINE ( 'NONE', #82444, #12612 ) ;
#82937 = CARTESIAN_POINT ( 'NONE',  ( -49.49642667126946094, -25.30285855287542773, 4.744951912546983230 ) ) ;
#82938 = CARTESIAN_POINT ( 'NONE',  ( 18.82035724208558491, -7.196742317222773799, 11.49999999999999645 ) ) ;
#82939 = CARTESIAN_POINT ( 'NONE',  ( -108.9545715455115129, -25.28814359653987154, 4.170144815448148634 ) ) ;
#82940 = CARTESIAN_POINT ( 'NONE',  ( -37.62287095715005592, -29.50250243563736774, 8.947779886222148704 ) ) ;
#82941 = CARTESIAN_POINT ( 'NONE',  ( -104.5228709571500758, -24.65952944569305316, 1.056160979905702346 ) ) ;
#82942 = PLANE ( 'NONE',  #19678 ) ;
#82943 = CARTESIAN_POINT ( 'NONE',  ( -110.3698707892751401, -25.29779155563274173, 3.294862198595579716 ) ) ;
#82944 = CARTESIAN_POINT ( 'NONE',  ( 7.713363164125232707, -18.29545692620113684, 11.49999999999998934 ) ) ;
#82945 = CARTESIAN_POINT ( 'NONE',  ( -113.6268379778973951, -24.15543982623907837, -0.2315651400026574602 ) ) ;
#82946 = CARTESIAN_POINT ( 'NONE',  ( 10.99584971316270732, 16.45119811332560289, -1.500000000000002220 ) ) ;
#82947 = DIRECTION ( 'NONE',  ( -0.000000000000000000, -1.000000000000000000, -0.000000000000000000 ) ) ;
#82948 = DIRECTION ( 'NONE',  ( -0.1311553622875919756, -0.000000000000000000, -0.9913618264504692190 ) ) ;
#82949 = CARTESIAN_POINT ( 'NONE',  ( -67.62287095715005592, -29.50247984919015209, -1.443849546365055359 ) ) ;
#82950 = CARTESIAN_POINT ( 'NONE',  ( -13.01863806243235899, 16.06808769575019014, 11.49999999999999645 ) ) ;
#82951 = CARTESIAN_POINT ( 'NONE',  ( 0.3910256410256441884, -6.376774720514427841, 21.75000000000000000 ) ) ;
#82952 = ADVANCED_FACE ( 'NONE', ( #71605 ), #2102, .T. ) ;
#82953 = CARTESIAN_POINT ( 'NONE',  ( -97.55620429048337883, -24.64965694238574656, 8.947790433994192938 ) ) ;
#82954 = APPROVAL ( #65262, 'UNSPECIFIED' ) ;
#82955 = PLANE ( 'NONE',  #45756 ) ;
#82956 = CARTESIAN_POINT ( 'NONE',  ( 6.262736145392394427, -21.83385498489561272, 11.49999999999999645 ) ) ;
#82957 = CIRCLE ( 'NONE', #79773, 2.350000000000000089 ) ;
#82958 = VERTEX_POINT ( 'NONE', #67487 ) ;
#82959 = B_SPLINE_SURFACE_WITH_KNOTS ( 'NONE', 3, 3, ( 
 ( #70197, #8800, #45866, #53985 ),
 ( #93517, #22002, #46862, #47364 ),
 ( #8294, #78293, #6789, #68706 ),
 ( #7792, #93019, #84912, #23496 ),
 ( #54475, #38735, #183, #38237 ),
 ( #52985, #84419, #39239, #24012 ),
 ( #39739, #70696, #45379, #1192 ) ),
 .UNSPECIFIED., .F., .F., .F.,
 ( 4, 3, 4 ),
 ( 4, 4 ),
 ( 0.3389043335492655795, 0.5146336264641651059, 0.6903629193790645768 ),
 ( 0.8868704786767156456, 0.9154791878198447197 ),
 .UNSPECIFIED. ) ;
#82960 = CARTESIAN_POINT ( 'NONE',  ( -0.02075734969026423599, 6.376774720514426953, 22.60902280011862686 ) ) ;
#82961 = CARTESIAN_POINT ( 'NONE',  ( 29.70220533433690946, 3.316774720514426456, 28.20564067601640801 ) ) ;
#82962 = CARTESIAN_POINT ( 'NONE',  ( 8.097539468418187170, -0.7382521156407183538, -3.736985260579223311 ) ) ;
#82963 = CARTESIAN_POINT ( 'NONE',  ( -95.62287095715005592, -23.47593901973091235, -1.443836447539001089 ) ) ;
#82964 = EDGE_CURVE ( 'NONE', #94513, #2264, #69020, .T. ) ;
#82965 = ORIENTED_EDGE ( 'NONE', *, *, #21798, .T. ) ;
#82966 = ORIENTED_EDGE ( 'NONE', *, *, #86314, .F. ) ;
#82967 = CARTESIAN_POINT ( 'NONE',  ( -29.49875734969025842, -5.965225279485572685, 25.61802280011862720 ) ) ;
#82968 = CARTESIAN_POINT ( 'NONE',  ( -15.36296916364455711, -16.94538937337987150, -1.500000000000002220 ) ) ;
#82969 = CARTESIAN_POINT ( 'NONE',  ( -29.66016279085162566, -23.66217729016224780, -1.055554856561816246 ) ) ;
#82970 = CARTESIAN_POINT ( 'NONE',  ( -15.49073194614445015, 15.02706685249526686, -1.500000000000002220 ) ) ;
#82971 = CARTESIAN_POINT ( 'NONE',  ( -123.5886726267617917, -24.65952944569305316, 1.056160979905707897 ) ) ;
#82972 = CARTESIAN_POINT ( 'NONE',  ( -50.62287095715005592, -29.50248789122583659, 2.256150453626215580 ) ) ;
#82973 = AXIS2_PLACEMENT_3D ( 'NONE', #98401, #37518, #30398 ) ;
#82974 = CARTESIAN_POINT ( 'NONE',  ( -18.95691745938505335, -12.16397891629814865, 11.49999999999999645 ) ) ;
#82975 = EDGE_LOOP ( 'NONE', ( #91596, #92511, #42832, #67887 ) ) ;
#82976 = CARTESIAN_POINT ( 'NONE',  ( -87.52287095715006160, -23.47593901973090524, -1.443836447538996648 ) ) ;
#82977 = AXIS2_PLACEMENT_3D ( 'NONE', #69732, #16421, #77810 ) ;
#82978 = CARTESIAN_POINT ( 'NONE',  ( -13.73438224071023761, 17.16576579689093762, 11.49999999999998934 ) ) ;
#82979 = CARTESIAN_POINT ( 'NONE',  ( -105.5906753045558588, -24.40133493613049964, 9.663955038902797057 ) ) ;
#82980 = CARTESIAN_POINT ( 'NONE',  ( -40.81364289383298427, -25.10925777354066923, 2.874306191861136117 ) ) ;
#82981 = ORIENTED_EDGE ( 'NONE', *, *, #10316, .F. ) ;
#82982 = CARTESIAN_POINT ( 'NONE',  ( 31.84105487026622683, -3.622774720514426949, -11.95870468328481984 ) ) ;
#82983 = CARTESIAN_POINT ( 'NONE',  ( -90.49854335619302503, -25.00182538069146787, 7.747789668545043362 ) ) ;
#82984 = VERTEX_POINT ( 'NONE', #5575 ) ;
#82985 = CARTESIAN_POINT ( 'NONE',  ( -29.52287095715007581, -23.87575411459822305, -0.6494985517685606391 ) ) ;
#82986 = ORIENTED_EDGE ( 'NONE', *, *, #85630, .T. ) ;
#82987 = ORIENTED_EDGE ( 'NONE', *, *, #28946, .F. ) ;
#82988 = EDGE_CURVE ( 'NONE', #87707, #51886, #64200, .T. ) ;
#82989 = CARTESIAN_POINT ( 'NONE',  ( 31.82032313667048484, 6.376774720514426953, 9.148483289431936782 ) ) ;
#82990 = CARTESIAN_POINT ( 'NONE',  ( 0.3910256410256441884, -5.876774720514426953, 21.75000000000000000 ) ) ;
#82991 = CARTESIAN_POINT ( 'NONE',  ( -57.56701934434523338, -23.48783264082477018, -1.443836473390095243 ) ) ;
#82992 = CARTESIAN_POINT ( 'NONE',  ( 10.07161678670223637, 17.78519941539584792, -1.500000000000002220 ) ) ;
#82993 = VERTEX_POINT ( 'NONE', #42170 ) ;
#82994 = CARTESIAN_POINT ( 'NONE',  ( 13.91401389203221406, 5.965225279485572685, 158.0376437107427137 ) ) ;
#82995 = CARTESIAN_POINT ( 'NONE',  ( -30.62200344337179914, -24.13759587396041439, -0.5132947483565731828 ) ) ;
#82997 = CARTESIAN_POINT ( 'NONE',  ( -79.62632635320383656, -25.20074414427590170, 3.409327697718777195 ) ) ;
#82996 = AXIS2_PLACEMENT_3D ( 'NONE', #33509, #64493, #95409 ) ;
#82998 = CARTESIAN_POINT ( 'NONE',  ( -47.58953762381672448, -23.48786465467240703, 11.44779295918255180 ) ) ;
#82999 = ORIENTED_EDGE ( 'NONE', *, *, #15219, .F. ) ;
#83000 = CARTESIAN_POINT ( 'NONE',  ( -49.52287095715006160, -24.65952944569304606, 1.056160979905693686 ) ) ;
#83001 = DIRECTION ( 'NONE',  ( 0.000000000000000000, 0.9999999999976377785, 2.173523156925979128E-06 ) ) ;
#83002 = APPROVAL_PERSON_ORGANIZATION ( #69726, #14687, #85431 ) ;
#83003 = CARTESIAN_POINT ( 'NONE',  ( 0.4431998670617953717, 20.78131286043265646, 11.49999999999998934 ) ) ;
#83004 = EDGE_CURVE ( 'NONE', #25851, #99951, #22987, .T. ) ;
#83005 = ORIENTED_EDGE ( 'NONE', *, *, #98271, .T. ) ;
#83007 = ORIENTED_EDGE ( 'NONE', *, *, #81458, .F. ) ;
#83006 = CARTESIAN_POINT ( 'NONE',  ( -40.41683116089613748, -25.30532407203700984, 5.082404393492757855 ) ) ;
#83008 = B_SPLINE_CURVE_WITH_KNOTS ( 'NONE', 3,
 ( #49080, #87118, #79508, #57200, #34842, #2397 ),
 .UNSPECIFIED., .F., .F.,
 ( 4, 2, 4 ),
 ( 6.391158118952235087E-06, 0.001387004593080775738, 0.002767618028042598960 ),
 .UNSPECIFIED. ) ;
#83009 = CARTESIAN_POINT ( 'NONE',  ( -91.23534077628073646, -25.23397913219354649, 6.409327625488847602 ) ) ;
#83010 = ORIENTED_EDGE ( 'NONE', *, *, #24268, .F. ) ;
#83011 = ORIENTED_EDGE ( 'NONE', *, *, #15429, .F. ) ;
#83012 = FACE_OUTER_BOUND ( 'NONE', #23069, .T. ) ;
#83013 = CARTESIAN_POINT ( 'NONE',  ( 14.15579980161844986, -3.316774720514426456, -28.31186755866361437 ) ) ;
#83014 = CIRCLE ( 'NONE', #87955, 18.35000000000000142 ) ;
#83015 = CARTESIAN_POINT ( 'NONE',  ( -113.6228709571500559, -23.47593901973091235, -1.443836447538999312 ) ) ;
#83016 = CARTESIAN_POINT ( 'NONE',  ( 8.160000000000000142, 1.990213166801898970, 6.144159427248533589 ) ) ;
#83018 = ORIENTED_EDGE ( 'NONE', *, *, #27357, .T. ) ;
#83017 = CARTESIAN_POINT ( 'NONE',  ( 19.88262469969689050, -9.776007750257504014, 11.49999999999999645 ) ) ;
#83019 = EDGE_CURVE ( 'NONE', #49971, #99116, #50766, .T. ) ;
#83020 = DIRECTION ( 'NONE',  ( -1.000000000000000000, 0.000000000000000000, 0.000000000000000000 ) ) ;
#83021 = CARTESIAN_POINT ( 'NONE',  ( 22.61563695565308407, -1.323143620866313208, -1.500000000000002220 ) ) ;
#83022 = EDGE_CURVE ( 'NONE', #54320, #76406, #74585, .T. ) ;
#83024 = ORIENTED_EDGE ( 'NONE', *, *, #22163, .T. ) ;
#83023 = CARTESIAN_POINT ( 'NONE',  ( -99.33845364856260574, -25.30505776661208728, 5.120429160701139182 ) ) ;
#83025 = EDGE_LOOP ( 'NONE', ( #45143, #57311, #5289, #32721 ) ) ;
#83026 = CARTESIAN_POINT ( 'NONE',  ( -10.26098930579144763, -5.972795536074636757, 28.98685178976001353 ) ) ;
#83027 = B_SPLINE_CURVE_WITH_KNOTS ( 'NONE', 3,
 ( #15262, #52837, #46219, #98993 ),
 .UNSPECIFIED., .F., .F.,
 ( 4, 4 ),
 ( 2.236995757993482539E-11, 0.0004668241723168402280 ),
 .UNSPECIFIED. ) ;
#83028 = AXIS2_PLACEMENT_3D ( 'NONE', #85547, #38375, #38873 ) ;
#83029 = CARTESIAN_POINT ( 'NONE',  ( -4.233023369943174075, 19.68221892606961987, 11.49999999999998934 ) ) ;
#83030 = DIRECTION ( 'NONE',  ( 0.000000000000000000, 0.000000000000000000, 1.000000000000000000 ) ) ;
#83031 = ORIENTED_EDGE ( 'NONE', *, *, #74433, .T. ) ;
#83032 = CARTESIAN_POINT ( 'NONE',  ( -89.52287095715004739, -23.96177878511309345, 10.65340807706329684 ) ) ;
#83033 = CARTESIAN_POINT ( 'NONE',  ( -8.840690135214121170, 20.45858245768130956, -1.500000000000002220 ) ) ;
#83034 = ORIENTED_EDGE ( 'NONE', *, *, #19298, .T. ) ;
#83035 = CARTESIAN_POINT ( 'NONE',  ( -4.968349358974361252, -6.376774720514411854, 19.46153846153847056 ) ) ;
#83036 = CARTESIAN_POINT ( 'NONE',  ( -89.62287095715007013, -23.95044443724992433, 10.65354141964649948 ) ) ;
#83037 = DIRECTION ( 'NONE',  ( -1.000000000000000000, -3.773278334444166432E-23, -8.201307841325785021E-29 ) ) ;
#83038 = CARTESIAN_POINT ( 'NONE',  ( -84.58953762381672448, -24.65952944569305316, 1.056160979905704567 ) ) ;
#83039 = CARTESIAN_POINT ( 'NONE',  ( -24.90875734969025501, 3.316774720514426456, 26.43402280011862615 ) ) ;
#83040 = CARTESIAN_POINT ( 'NONE',  ( -18.49313839071750820, -6.238557295281221826, -1.500000000000002220 ) ) ;
#83041 = AXIS2_PLACEMENT_3D ( 'NONE', #91173, #91667, #69339 ) ;
#83042 = CARTESIAN_POINT ( 'NONE',  ( 5.910897418159350103, -20.63055655796343757, 11.49999999999998934 ) ) ;
#83043 = CARTESIAN_POINT ( 'NONE',  ( -2.702089344534958304, -5.876774720514411854, 19.72789237585158162 ) ) ;
#83044 = DIRECTION ( 'NONE',  ( 1.000000000000000000, 3.773278334444166432E-23, 8.201307841325785021E-29 ) ) ;
#83045 = DIRECTION ( 'NONE',  ( 0.8788171126619707119, -0.4771587602595986910, 0.000000000000000000 ) ) ;
#83046 = CARTESIAN_POINT ( 'NONE',  ( 13.81544771398824345, -18.15223324129861382, -1.500000000000002220 ) ) ;
#83047 = ADVANCED_FACE ( 'NONE', ( #82694 ), #73599, .F. ) ;
#83048 = CARTESIAN_POINT ( 'NONE',  ( -20.27875734969026311, -4.543225279485573864, 24.00402280011862288 ) ) ;
#83049 = CARTESIAN_POINT ( 'NONE',  ( 7.160000000000000142, 0.1579206558577707364, 6.788828319098143105 ) ) ;
#83050 = CARTESIAN_POINT ( 'NONE',  ( 18.80405327530603543, -6.659971710459020144, 11.49999999999999645 ) ) ;
#83051 = DIRECTION ( 'NONE',  ( -3.773278334453079030E-23, 0.9999999999976377785, 2.173523156925979128E-06 ) ) ;
#83052 = CARTESIAN_POINT ( 'NONE',  ( -74.49654804551374809, -24.66019654487200441, 8.947790411086105067 ) ) ;
#83053 = PLANE ( 'NONE',  #86103 ) ;
#83054 = ORIENTED_EDGE ( 'NONE', *, *, #13583, .T. ) ;
#83055 = PLANE ( 'NONE',  #29912 ) ;
#83056 = CARTESIAN_POINT ( 'NONE',  ( -124.5228709571502037, -23.96127896941633750, -0.6493128931037959184 ) ) ;
#83057 = CARTESIAN_POINT ( 'NONE',  ( 20.88924836996103451, 6.054424527964996194, -1.500000000000002220 ) ) ;
#83058 = CARTESIAN_POINT ( 'NONE',  ( -37.58953762381672448, -23.47593901973091235, -1.443836447539011525 ) ) ;
#83059 = CARTESIAN_POINT ( 'NONE',  ( 17.63768857353127828, -8.544740250177758512, -1.500000000000002220 ) ) ;
#83060 = CARTESIAN_POINT ( 'NONE',  ( -99.33777189820985143, -25.23274841714367511, 6.421454660997744313 ) ) ;
#83061 = B_SPLINE_CURVE_WITH_KNOTS ( 'NONE', 3,
 ( #17953, #56029, #93060, #63645 ),
 .UNSPECIFIED., .F., .F.,
 ( 4, 4 ),
 ( 2.775557561562891351E-17, 0.0001000000000000167286 ),
 .UNSPECIFIED. ) ;
#83062 = AXIS2_PLACEMENT_3D ( 'NONE', #10807, #74208, #5186 ) ;
#83063 = VERTEX_POINT ( 'NONE', #21286 ) ;
#83064 = SECURITY_CLASSIFICATION ( '', '', #43535 ) ;
#83065 = CARTESIAN_POINT ( 'NONE',  ( -60.62287095715003460, -23.85229601348995843, 10.88205029486208986 ) ) ;
#83066 = CARTESIAN_POINT ( 'NONE',  ( -123.6228709571500559, -23.47596703998600631, 11.44779298504227860 ) ) ;
#83067 = CARTESIAN_POINT ( 'NONE',  ( 18.14102482237423075, -9.550406459077080967, 11.49999999999999645 ) ) ;
#83068 = DIRECTION ( 'NONE',  ( -1.000000000000000000, -3.773278334444167608E-23, -8.201307833595939069E-29 ) ) ;
#83069 = CARTESIAN_POINT ( 'NONE',  ( -42.52287095715005449, -24.66019654487199020, 8.947790411086133489 ) ) ;
#83070 = EDGE_CURVE ( 'NONE', #94577, #53188, #20787, .T. ) ;
#83071 = VECTOR ( 'NONE', #70713, 1000.000000000000114 ) ;
#83072 = ORIENTED_EDGE ( 'NONE', *, *, #59050, .F. ) ;
#83073 = CARTESIAN_POINT ( 'NONE',  ( -62.52287095715006160, -24.64965694238406613, 8.947790433994201820 ) ) ;
#83074 = CARTESIAN_POINT ( 'NONE',  ( -40.42371425561744047, -25.28892422309021981, 3.294940063421055498 ) ) ;
#83075 = EDGE_CURVE ( 'NONE', #54184, #44858, #58386, .T. ) ;
#83076 = DIRECTION ( 'NONE',  ( 0.000000000000000000, -0.9999999999976377785, -2.173523156925979975E-06 ) ) ;
#83077 = VECTOR ( 'NONE', #28480, 1000.000000000000000 ) ;
#83078 = DIRECTION ( 'NONE',  ( -3.773278334453079030E-23, 0.9999999999976377785, 2.173523156925979128E-06 ) ) ;
#83079 = EDGE_LOOP ( 'NONE', ( #53061, #44970, #15727, #4995 ) ) ;
#83080 = DIRECTION ( 'NONE',  ( 0.000000000000000000, 0.000000000000000000, 1.000000000000000000 ) ) ;
#83081 = ADVANCED_FACE ( 'NONE', ( #83187 ), #91844, .T. ) ;
#83082 = EDGE_CURVE ( 'NONE', #90098, #63613, #90315, .T. ) ;
#83083 = CARTESIAN_POINT ( 'NONE',  ( -2.116611060711651504, 22.89395876494169002, 11.49999999999999645 ) ) ;
#83084 = CARTESIAN_POINT ( 'NONE',  ( -22.70586268970451371, -1.818501321912391999, 11.49999999999998934 ) ) ;
#83085 = CARTESIAN_POINT ( 'NONE',  ( -110.5546867764639671, -24.15602025860899360, 10.28564288303533480 ) ) ;
#83086 = B_SPLINE_SURFACE_WITH_KNOTS ( 'NONE', 3, 3, ( 
 ( #17386, #56970, #25500, #40726 ),
 ( #24989, #71684, #18388, #49357 ),
 ( #71182, #26509, #2181, #3183 ),
 ( #3675, #33113, #87397, #10781 ),
 ( #64091, #34123, #57970, #48854 ),
 ( #65095, #57473, #18881, #88406 ),
 ( #88909, #19380, #78765, #9265 ) ),
 .UNSPECIFIED., .F., .F., .F.,
 ( 4, 3, 4 ),
 ( 4, 4 ),
 ( 0.7945040050992251413, 0.8970133687736507877, 0.9995227324480765452 ),
 ( 0.7796921278179643755, 0.7810648099988581894 ),
 .UNSPECIFIED. ) ;
#83087 = CARTESIAN_POINT ( 'NONE',  ( -29.49875734969026198, -5.965225279485572685, 2.362022800118626531 ) ) ;
#83088 = DIRECTION ( 'NONE',  ( 0.000000000000000000, 1.084202172485504434E-16, -1.000000000000000000 ) ) ;
#83089 = EDGE_CURVE ( 'NONE', #97718, #30829, #33989, .T. ) ;
#83090 = PLANE ( 'NONE',  #78675 ) ;
#83091 = CARTESIAN_POINT ( 'NONE',  ( -64.62287095715005592, -23.48783264082478084, -1.443836473390069042 ) ) ;
#83092 = CARTESIAN_POINT ( 'NONE',  ( 21.76694381678408519, 2.417257996116004115, -1.500000000000002220 ) ) ;
#83093 = CARTESIAN_POINT ( 'NONE',  ( 7.403636664866980688, -5.876774720514423400, 21.18544102487025782 ) ) ;
#83094 = CARTESIAN_POINT ( 'NONE',  ( -50.62287095715006302, -24.92579138211019085, 1.929029949965668456 ) ) ;
#83095 = CARTESIAN_POINT ( 'NONE',  ( -41.46445985487523700, -25.29262591909929725, 4.252576102391492086 ) ) ;
#83096 = DIRECTION ( 'NONE',  ( 0.000000000000000000, -1.000000000000000000, 0.000000000000000000 ) ) ;
#83097 = CARTESIAN_POINT ( 'NONE',  ( -106.6228709571500559, -29.50248528299804818, 1.056150453629043584 ) ) ;
#83098 = CARTESIAN_POINT ( 'NONE',  ( -41.32836283488544638, 4.772774720514425972, 39.26872235229541985 ) ) ;
#83099 = ORIENTED_EDGE ( 'NONE', *, *, #13018, .F. ) ;
#83100 = B_SPLINE_CURVE_WITH_KNOTS ( 'NONE', 3,
 ( #92305, #13674, #38022, #91805, #30409, #100396 ),
 .UNSPECIFIED., .F., .F.,
 ( 4, 2, 4 ),
 ( 6.391158118963032216E-06, 0.001387004593080781809, 0.002767618028042600695 ),
 .UNSPECIFIED. ) ;
#83101 = CARTESIAN_POINT ( 'NONE',  ( 20.25987197511681259, 2.754759976156288204, -1.500000000000002220 ) ) ;
#83102 = B_SPLINE_CURVE_WITH_KNOTS ( 'NONE', 3,
 ( #50446, #80394, #82383, #10884, #3783, #88510, #11875, #35225, #28108, #34719, #97116, #73776, #66696, #65200 ),
 .UNSPECIFIED., .F., .F.,
 ( 4, 2, 2, 2, 2, 2, 4 ),
 ( 3.469446951953614189E-18, 0.0003991292329371358004, 0.0007982584658742681314, 0.001197387698811397914, 0.001596516931748527806, 0.002394775397622781951, 0.003193033863497036530 ),
 .UNSPECIFIED. ) ;
#83103 = EDGE_LOOP ( 'NONE', ( #37483, #63510, #9108, #74594 ) ) ;
#83104 = ORIENTED_EDGE ( 'NONE', *, *, #97527, .F. ) ;
#83105 = ORIENTED_EDGE ( 'NONE', *, *, #84463, .F. ) ;
#83106 = ORIENTED_EDGE ( 'NONE', *, *, #46709, .F. ) ;
#83107 = ADVANCED_FACE ( 'NONE', ( #19793 ), #58877, .F. ) ;
#83108 = CARTESIAN_POINT ( 'NONE',  ( 17.08057647167376913, 15.47633299359885761, -1.500000000000002220 ) ) ;
#83109 = LINE ( 'NONE', #98332, #48707 ) ;
#83110 = CARTESIAN_POINT ( 'NONE',  ( 17.32893120472914816, 10.46255702124672027, -1.500000000000002220 ) ) ;
#83111 = AXIS2_PLACEMENT_3D ( 'NONE', #33219, #40338, #48958 ) ;
#83112 = VERTEX_POINT ( 'NONE', #90815 ) ;
#83113 = CARTESIAN_POINT ( 'NONE',  ( 29.70220533433691301, 3.316774720514426456, 28.20564067601639735 ) ) ;
#83114 = DIRECTION ( 'NONE',  ( 0.000000000000000000, 0.9999999999976377785, 2.173523156925979975E-06 ) ) ;
#83115 = LINE ( 'NONE', #90244, #41581 ) ;
#83116 = CARTESIAN_POINT ( 'NONE',  ( -70.49056310608266074, -24.83618233451450052, 1.606449574219541487 ) ) ;
#83118 = ORIENTED_EDGE ( 'NONE', *, *, #86593, .T. ) ;
#83117 = CARTESIAN_POINT ( 'NONE',  ( -21.42254595866439004, -0.3319015934494286557, 11.49999999999999645 ) ) ;
#83119 = LINE ( 'NONE', #51693, #12741 ) ;
#83120 = CARTESIAN_POINT ( 'NONE',  ( -41.54630002450753068, -24.15543982623907127, -0.2315651400026566831 ) ) ;
#83121 = ORIENTED_EDGE ( 'NONE', *, *, #23937, .T. ) ;
#83122 = CARTESIAN_POINT ( 'NONE',  ( 20.27745880512110688, -4.159726151199424571, 11.49999999999998934 ) ) ;
#83123 = EDGE_CURVE ( 'NONE', #14722, #54721, #71559, .T. ) ;
#83124 = ORIENTED_EDGE ( 'NONE', *, *, #14394, .T. ) ;
#83125 = EDGE_CURVE ( 'NONE', #41225, #58220, #89706, .T. ) ;
#83126 = CARTESIAN_POINT ( 'NONE',  ( -91.52287095715013265, -23.96177878511310055, 10.65340807706329507 ) ) ;
#83127 = ORIENTED_EDGE ( 'NONE', *, *, #7207, .T. ) ;
#83128 = CARTESIAN_POINT ( 'NONE',  ( 4.931982383686722926, -6.376774720514411854, 19.38944687450761961 ) ) ;
#83129 = VERTEX_POINT ( 'NONE', #61378 ) ;
#83130 = CARTESIAN_POINT ( 'NONE',  ( 6.892386425805808514, -19.84609432511738447, -1.500000000000002220 ) ) ;
#83131 = CARTESIAN_POINT ( 'NONE',  ( -1.351711525931510449, 21.94731587555429186, 11.49999999999999645 ) ) ;
#83132 = EDGE_CURVE ( 'NONE', #90808, #70257, #29737, .T. ) ;
#83133 = CARTESIAN_POINT ( 'NONE',  ( -37.62898825168296923, -24.51419770103156637, 9.386484678747175181 ) ) ;
#83134 = CARTESIAN_POINT ( 'NONE',  ( -21.23328875057882570, -7.520457577684837247, 11.49999999999998934 ) ) ;
#83135 = CARTESIAN_POINT ( 'NONE',  ( -18.84683179826791743, -9.195131953753229226, -1.500000000000002220 ) ) ;
#83136 = EDGE_CURVE ( 'NONE', #49712, #69249, #92801, .T. ) ;
#83137 = CARTESIAN_POINT ( 'NONE',  ( -2.768609665556980293, -0.3587747205144057872, -29.41086200512614823 ) ) ;
#83138 = CARTESIAN_POINT ( 'NONE',  ( -91.55620429048337883, -23.48783264082478084, -1.443836473390063713 ) ) ;
#83139 = AXIS2_PLACEMENT_3D ( 'NONE', #28288, #37409, #59248 ) ;
#83140 = DIRECTION ( 'NONE',  ( 0.000000000000000000, 0.000000000000000000, 1.000000000000000000 ) ) ;
#83141 = ORIENTED_EDGE ( 'NONE', *, *, #86906, .T. ) ;
#83142 = B_SPLINE_CURVE_WITH_KNOTS ( 'NONE', 3,
 ( #12461, #4857, #28194, #22057 ),
 .UNSPECIFIED., .F., .F.,
 ( 4, 4 ),
 ( 0.000000000000000000, 1.000000000000000000 ),
 .UNSPECIFIED. ) ;
#83143 = EDGE_CURVE ( 'NONE', #60457, #11737, #83100, .T. ) ;
#83144 = APPROVAL_PERSON_ORGANIZATION ( #71367, #15255, #9455 ) ;
#83145 = EDGE_LOOP ( 'NONE', ( #42364, #99134, #32308, #64445 ) ) ;
#83146 = ORIENTED_EDGE ( 'NONE', *, *, #8179, .F. ) ;
#83147 = B_SPLINE_CURVE_WITH_KNOTS ( 'NONE', 3,
 ( #55011, #85438, #7820, #15426, #39763, #94054 ),
 .UNSPECIFIED., .F., .F.,
 ( 4, 2, 4 ),
 ( 0.000000000000000000, 0.001380764517854764966, 0.002761529035709529931 ),
 .UNSPECIFIED. ) ;
#83148 = CARTESIAN_POINT ( 'NONE',  ( -66.55386350891794223, -23.96119346886880308, -0.6495511937832151306 ) ) ;
#83149 = CARTESIAN_POINT ( 'NONE',  ( -19.33005188562793819, 9.364626179424670127, -1.500000000000002220 ) ) ;
#83150 = AXIS2_PLACEMENT_3D ( 'NONE', #20520, #70080, #45384 ) ;
#83151 = CARTESIAN_POINT ( 'NONE',  ( -81.48149462243459595, -25.23679622552714363, 6.293943003980942308 ) ) ;
#83152 = EDGE_LOOP ( 'NONE', ( #9622, #53756, #65665, #25759 ) ) ;
#83153 = CARTESIAN_POINT ( 'NONE',  ( -2.902382693073098707, -20.91247731031871382, 11.49999999999998934 ) ) ;
#83154 = CARTESIAN_POINT ( 'NONE',  ( -99.58390386930925331, -25.25019242640517447, 3.741874911158628247 ) ) ;
#83155 = CARTESIAN_POINT ( 'NONE',  ( -81.48149462243461016, -25.24685308744633261, 6.293942982122115559 ) ) ;
#83156 = CARTESIAN_POINT ( 'NONE',  ( -100.5228709571500332, -24.83602698348161297, 1.605859176311263292 ) ) ;
#83157 = CARTESIAN_POINT ( 'NONE',  ( 7.805843057017202824, 3.316774720514425567, -27.15467198446602026 ) ) ;
#83158 = CARTESIAN_POINT ( 'NONE',  ( -65.52287095715006160, -29.50249982740957577, 7.747779886224967605 ) ) ;
#83159 = CARTESIAN_POINT ( 'NONE',  ( -14.81638660137672225, 16.44347145309322045, -1.500000000000002220 ) ) ;
#83160 = VECTOR ( 'NONE', #36351, 1000.000000000000114 ) ;
#83161 = PLANE ( 'NONE',  #6303 ) ;
#83162 = CARTESIAN_POINT ( 'NONE',  ( -56.52287095715006870, -24.64965694238407323, 8.947790433994201820 ) ) ;
#83163 = CARTESIAN_POINT ( 'NONE',  ( 12.09245314707524876, 4.658029312750951334, -27.52981586573924488 ) ) ;
#83164 = CARTESIAN_POINT ( 'NONE',  ( -41.86878170341644534, -25.31624462002888265, 4.256748773907617078 ) ) ;
#83165 = CARTESIAN_POINT ( 'NONE',  ( -100.6291402768932386, -24.52300882791526959, 0.6510814631126226049 ) ) ;
#83166 = CARTESIAN_POINT ( 'NONE',  ( 10.09180897563621926, 16.61094848277074476, 11.49999999999998934 ) ) ;
#83167 = CARTESIAN_POINT ( 'NONE',  ( -15.71168838272081558, 14.50144224353281786, -1.500000000000002220 ) ) ;
#83168 = FACE_OUTER_BOUND ( 'NONE', #98967, .T. ) ;
#83169 = DIRECTION ( 'NONE',  ( 0.000000000000000000, -0.000000000000000000, -1.000000000000000000 ) ) ;
#83170 = FACE_OUTER_BOUND ( 'NONE', #74546, .T. ) ;
#83171 = LINE ( 'NONE', #21269, #84892 ) ;
#83172 = CARTESIAN_POINT ( 'NONE',  ( 22.64978874513612439, 0.4204215919581203442, -1.500000000000002220 ) ) ;
#83173 = B_SPLINE_SURFACE_WITH_KNOTS ( 'NONE', 3, 3, ( 
 ( #74775, #60079, #4286, #66207 ),
 ( #5272, #19998, #43846, #36230 ),
 ( #52454, #21476, #12380, #83386 ),
 ( #28119, #67193, #35236, #27626 ),
 ( #82394, #90016, #98108, #28614 ),
 ( #13873, #20985, #44844, #74290 ),
 ( #90508, #75768, #6268, #58572 ),
 ( #50966, #81903, #4781, #35736 ),
 ( #66707, #97618, #51459, #12872 ),
 ( #51958, #82887, #13372, #44350 ) ),
 .UNSPECIFIED., .F., .F., .F.,
 ( 4, 3, 3, 4 ),
 ( 4, 4 ),
 ( 0.7022005934544808259, 0.7765311282028796169, 0.8508616629512784080, 0.9995227324480758790 ),
 ( 0.2995301457407982260, 0.3007213865952733656 ),
 .UNSPECIFIED. ) ;
#83174 = EDGE_LOOP ( 'NONE', ( #80882, #98581, #83921, #97000 ) ) ;
#83175 = CARTESIAN_POINT ( 'NONE',  ( 14.43441819135929727, 5.965225279485572685, -28.36222020317710246 ) ) ;
#83176 = CARTESIAN_POINT ( 'NONE',  ( -102.6228709571500559, -24.64965695001469115, 8.947790433994178727 ) ) ;
#83177 = CARTESIAN_POINT ( 'NONE',  ( -19.78623529325263775, -1.157695164950638844, 11.49999999999999645 ) ) ;
#83178 = CARTESIAN_POINT ( 'NONE',  ( -59.62287095715005592, -24.51283580621365132, 0.6167428607019761477 ) ) ;
#83179 = CARTESIAN_POINT ( 'NONE',  ( -2.704906987277324593, 5.965225279485572685, -28.92935364444904067 ) ) ;
#83180 = ORIENTED_EDGE ( 'NONE', *, *, #50736, .T. ) ;
#83181 = CARTESIAN_POINT ( 'NONE',  ( -53.62287095715005592, -24.50321055353806798, 9.387540953477540029 ) ) ;
#83182 = CIRCLE ( 'NONE', #75069, 0.3000000000000016542 ) ;
#83183 = CARTESIAN_POINT ( 'NONE',  ( -75.52287095715010423, -24.92604778743017846, 8.074972756849359001 ) ) ;
#83184 = CARTESIAN_POINT ( 'NONE',  ( 21.64940796807912449, -0.2623997510114038922, 11.49999999999998934 ) ) ;
#83185 = CARTESIAN_POINT ( 'NONE',  ( -49.73634623139758304, -25.27517911410419416, 2.988891300836324039 ) ) ;
#83186 = CARTESIAN_POINT ( 'NONE',  ( 17.17441491540288823, 9.109037055621362455, -1.500000000000002220 ) ) ;
#83187 = FACE_OUTER_BOUND ( 'NONE', #96111, .T. ) ;
#83188 = PLANE ( 'NONE',  #10224 ) ;
#83189 = CARTESIAN_POINT ( 'NONE',  ( 17.16143643543069075, 9.858047367376444825, 11.49999999999998934 ) ) ;
#83190 = EDGE_LOOP ( 'NONE', ( #51215, #34837, #71217, #71894 ) ) ;
#83191 = B_SPLINE_CURVE_WITH_KNOTS ( 'NONE', 3,
 ( #40196, #17354, #56939, #16346, #47312, #71151 ),
 .UNSPECIFIED., .F., .F.,
 ( 4, 2, 4 ),
 ( 1.570887131794952276E-05, 0.001396322306279766060, 0.002776935741241582344 ),
 .UNSPECIFIED. ) ;
#83192 = VECTOR ( 'NONE', #68616, 1000.000000000000114 ) ;
#83193 = CARTESIAN_POINT ( 'NONE',  ( -14.66855384320708033, -14.05595220846724835, 11.49999999999999645 ) ) ;
#83194 = DIRECTION ( 'NONE',  ( -3.773278334453080206E-23, 0.9999999999976377785, 2.173523156925979975E-06 ) ) ;
#83195 = CARTESIAN_POINT ( 'NONE',  ( -98.52287095715006160, -23.48786465467241769, 11.44779295918254114 ) ) ;
#83196 = ADVANCED_FACE ( 'NONE', ( #84692 ), #22775, .T. ) ;
#83197 = B_SPLINE_CURVE_WITH_KNOTS ( 'NONE', 3,
 ( #2755, #95090, #33187, #33696, #95589, #49939, #64674, #55542 ),
 .UNSPECIFIED., .F., .F.,
 ( 4, 2, 2, 4 ),
 ( 0.000000000000000000, 0.002001098010032797275, 0.003001647015049197648, 0.004002196020065598020 ),
 .UNSPECIFIED. ) ;
#83198 = ORIENTED_EDGE ( 'NONE', *, *, #59759, .F. ) ;
#83199 = CARTESIAN_POINT ( 'NONE',  ( -30.59367615247571592, -24.87212640336024805, 1.420893871182737467 ) ) ;
#83200 = CARTESIAN_POINT ( 'NONE',  ( 13.02968616431713578, -5.152774720514426754, -26.31186222701416000 ) ) ;
#83201 = CARTESIAN_POINT ( 'NONE',  ( -87.52287095715006160, -29.50248528299804818, 1.056150453629040253 ) ) ;
#83202 = EDGE_CURVE ( 'NONE', #38457, #70502, #54557, .T. ) ;
#83203 = CARTESIAN_POINT ( 'NONE',  ( -95.62287095715009855, -24.15431212366392799, -0.2830839119429097717 ) ) ;
#83204 = DIRECTION ( 'NONE',  ( -3.773278334453079030E-23, 0.9999999999976377785, 2.173523156925979128E-06 ) ) ;
#83205 = CARTESIAN_POINT ( 'NONE',  ( -7.287290609967129740, 18.71191762695291771, -1.500000000000002220 ) ) ;
#83206 = AXIS2_PLACEMENT_3D ( 'NONE', #12481, #57186, #11982 ) ;
#83207 = ADVANCED_FACE ( 'NONE', ( #15684 ), #37527, .T. ) ;
#83208 = CARTESIAN_POINT ( 'NONE',  ( -28.55620429048340725, -23.32632435101244894, -1.443835797391826548 ) ) ;
#83209 = ORIENTED_EDGE ( 'NONE', *, *, #38909, .T. ) ;
#83210 = CARTESIAN_POINT ( 'NONE',  ( -117.6228709571500559, -23.47596703998600631, 11.44779298504227683 ) ) ;
#83211 = EDGE_CURVE ( 'NONE', #38181, #99597, #34594, .T. ) ;
#83212 = EDGE_CURVE ( 'NONE', #32836, #66793, #45643, .T. ) ;
#83213 = VECTOR ( 'NONE', #45044, 1000.000000000000000 ) ;
#83214 = CARTESIAN_POINT ( 'NONE',  ( 20.41593879258296695, -10.28030303932802880, 11.49999999999999645 ) ) ;
#83215 = CARTESIAN_POINT ( 'NONE',  ( -30.47287095715008576, -25.25807433263999258, 3.875005595686505711 ) ) ;
#83216 = DIRECTION ( 'NONE',  ( 0.000000000000000000, -2.173523156925980399E-06, 0.9999999999976378895 ) ) ;
#83217 = CARTESIAN_POINT ( 'NONE',  ( -7.641025641025641413, -6.376774720514418959, 20.36458333333334636 ) ) ;
#83218 = ADVANCED_FACE ( 'NONE', ( #84189 ), #14680, .T. ) ;
#83219 = CARTESIAN_POINT ( 'NONE',  ( -43.52287095715006160, -24.64965694238406613, 8.947790433994205372 ) ) ;
#83220 = B_SPLINE_CURVE_WITH_KNOTS ( 'NONE', 3,
 ( #52945, #99091, #21463, #69153, #44337, #28601 ),
 .UNSPECIFIED., .F., .F.,
 ( 4, 2, 4 ),
 ( 0.000000000000000000, 0.001380764517854765182, 0.002761529035709530365 ),
 .UNSPECIFIED. ) ;
#83221 = CARTESIAN_POINT ( 'NONE',  ( -53.01255352321339842, 2.682774720514426559, 35.59556822165056644 ) ) ;
#83222 = AXIS2_PLACEMENT_3D ( 'NONE', #4950, #19661, #4462 ) ;
#83223 = FACE_OUTER_BOUND ( 'NONE', #13684, .T. ) ;
#83224 = ORIENTED_EDGE ( 'NONE', *, *, #61618, .T. ) ;
#83225 = CARTESIAN_POINT ( 'NONE',  ( 14.56535739210195857, -14.21638276092092745, 11.49999999999998934 ) ) ;
#83226 = VECTOR ( 'NONE', #31883, 1000.000000000000114 ) ;
#83227 = EDGE_LOOP ( 'NONE', ( #74287, #89213, #8503, #13982 ) ) ;
#83228 = B_SPLINE_CURVE_WITH_KNOTS ( 'NONE', 3,
 ( #3969, #65392, #41529, #2977, #18184, #72484 ),
 .UNSPECIFIED., .F., .F.,
 ( 4, 2, 4 ),
 ( 6.384118678608570081E-06, 0.001386860460828373684, 0.002767336802978138856 ),
 .UNSPECIFIED. ) ;
#83229 = EDGE_CURVE ( 'NONE', #49573, #76836, #4419, .T. ) ;
#83230 = CARTESIAN_POINT ( 'NONE',  ( 22.85142058292489153, -2.183311388647848350, 11.49999999999998934 ) ) ;
#83231 = CARTESIAN_POINT ( 'NONE',  ( -115.6228709571500559, -23.48786465467242479, 11.44779295918253759 ) ) ;
#83232 = ORIENTED_EDGE ( 'NONE', *, *, #79905, .T. ) ;
#83233 = CARTESIAN_POINT ( 'NONE',  ( -38.62287095715005592, -23.47593901973091235, -1.443836447539011525 ) ) ;
#83234 = CARTESIAN_POINT ( 'NONE',  ( -67.52287095715004739, -24.33927499327855415, 9.819080762295804732 ) ) ;
#83235 = ADVANCED_FACE ( 'NONE', ( #85279 ), #7661, .F. ) ;
#83236 = CARTESIAN_POINT ( 'NONE',  ( -74.62287095715005592, -23.47593901973091235, -1.443836447539006196 ) ) ;
#83238 = ORIENTED_EDGE ( 'NONE', *, *, #11498, .F. ) ;
#83237 = CARTESIAN_POINT ( 'NONE',  ( -7.948041996521916452, 19.69052605537007850, 11.49999999999999645 ) ) ;
#83239 = ORIENTED_EDGE ( 'NONE', *, *, #25437, .F. ) ;
#83240 = CARTESIAN_POINT ( 'NONE',  ( -10.56713949322891999, -19.48831581008217384, -1.500000000000002220 ) ) ;
#83241 = CARTESIAN_POINT ( 'NONE',  ( -13.12974562303265813, -15.89414520977026513, 11.49999999999998934 ) ) ;
#83242 = EDGE_CURVE ( 'NONE', #31325, #23352, #14090, .T. ) ;
#83243 = B_SPLINE_CURVE_WITH_KNOTS ( 'NONE', 3,
 ( #82129, #96357, #18233, #26346 ),
 .UNSPECIFIED., .F., .F.,
 ( 4, 4 ),
 ( 0.1899215428025058938, 0.1989279740746213720 ),
 .UNSPECIFIED. ) ;
#83244 = ORIENTED_EDGE ( 'NONE', *, *, #29669, .T. ) ;
#83245 = ORIENTED_EDGE ( 'NONE', *, *, #7979, .T. ) ;
#83246 = DIRECTION ( 'NONE',  ( 3.773278334444167608E-23, -1.000000000000000000, 0.000000000000000000 ) ) ;
#83247 = CARTESIAN_POINT ( 'NONE',  ( -36.55620429048339304, -24.64898659630528854, 1.056161002820822592 ) ) ;
#83248 = ORIENTED_EDGE ( 'NONE', *, *, #69722, .F. ) ;
#83249 = ORIENTED_EDGE ( 'NONE', *, *, #55210, .F. ) ;
#83250 = LINE ( 'NONE', #75627, #32447 ) ;
#83251 = CARTESIAN_POINT ( 'NONE',  ( -41.63440463616400677, -24.35071581493542325, 9.817618358456032368 ) ) ;
#83252 = DIRECTION ( 'NONE',  ( 0.000000000000000000, -2.173523156925979552E-06, 0.9999999999976378895 ) ) ;
#83253 = CARTESIAN_POINT ( 'NONE',  ( 19.40724743217988291, -7.346346906864608783, -1.500000000000002220 ) ) ;
#83254 = CARTESIAN_POINT ( 'NONE',  ( 9.495391690522565042, 19.61495305411445500, 11.49999999999999645 ) ) ;
#83255 = AXIS2_PLACEMENT_3D ( 'NONE', #63417, #2005, #17722 ) ;
#83256 = FACE_OUTER_BOUND ( 'NONE', #60193, .T. ) ;
#83257 = CARTESIAN_POINT ( 'NONE',  ( -113.6228709571501128, -23.96177878511308634, 10.65340807706329507 ) ) ;
#83258 = CARTESIAN_POINT ( 'NONE',  ( -115.6235241281218009, -25.00158670708910691, 2.256160236439219258 ) ) ;
#83259 = CARTESIAN_POINT ( 'NONE',  ( -16.61153998044026991, -15.06042057022924929, 11.49999999999998934 ) ) ;
#83260 = EDGE_CURVE ( 'NONE', #94215, #20042, #85791, .T. ) ;
#83261 = CARTESIAN_POINT ( 'NONE',  ( -51.29687923781917647, -25.31296603634400100, 3.993462069187891039 ) ) ;
#83262 = ORIENTED_EDGE ( 'NONE', *, *, #38133, .T. ) ;
#83263 = B_SPLINE_CURVE_WITH_KNOTS ( 'NONE', 3,
 ( #215, #77325, #24546, #93550, #8831, #86453, #32162, #70232, #69737, #8327, #7826, #85954, #93053, #31160, #23029, #45904, #62130, #712, #54511 ),
 .UNSPECIFIED., .F., .F.,
 ( 4, 1, 1, 1, 1, 1, 1, 1, 1, 1, 1, 1, 1, 1, 1, 1, 4 ),
 ( 0.000000000000000000, 0.06867706841303485021, 0.1368709585090958636, 0.2061143571452989376, 0.2775381819697280150, 0.3497719775548984722, 0.4212508361555684644, 0.4929107569233693309, 0.5670265889927383895, 0.6066141532413351634, 0.6497039535189884640, 0.6973031504846843864, 0.7490856597091365421, 0.8048806474593092064, 0.8654850057023351084, 0.9302371271531362229, 1.000000000000000000 ),
 .UNSPECIFIED. ) ;
#83264 = DIRECTION ( 'NONE',  ( -3.773278334453079618E-23, 0.9999999999976377785, 2.173523156925979975E-06 ) ) ;
#83265 = CARTESIAN_POINT ( 'NONE',  ( -57.58953762381671027, -24.65952944569304250, 1.056160979905691910 ) ) ;
#83266 = CIRCLE ( 'NONE', #55705, 12.65241003308275758 ) ;
#83267 = EDGE_LOOP ( 'NONE', ( #17459, #35829, #69467, #21507 ) ) ;
#83268 = VERTEX_POINT ( 'NONE', #84780 ) ;
#83269 = EDGE_CURVE ( 'NONE', #10237, #99590, #24385, .T. ) ;
#83270 = CARTESIAN_POINT ( 'NONE',  ( -99.91009256315520304, -25.31150033986424575, 5.318604188631694818 ) ) ;
#83271 = ORIENTED_EDGE ( 'NONE', *, *, #91344, .T. ) ;
#83272 = CARTESIAN_POINT ( 'NONE',  ( -20.53569570583907122, -5.550916044964551155, -1.500000000000002220 ) ) ;
#83273 = ORIENTED_EDGE ( 'NONE', *, *, #48332, .F. ) ;
#83274 = CARTESIAN_POINT ( 'NONE',  ( 32.98733314340959311, 5.965225279485572685, 2.074222136288530027 ) ) ;
#83275 = CARTESIAN_POINT ( 'NONE',  ( 15.37114825158464271, 14.37155165002682544, -1.500000000000002220 ) ) ;
#83276 = CARTESIAN_POINT ( 'NONE',  ( -82.52287095715006160, -24.64898659630367916, 1.056161002820826145 ) ) ;
#83277 = CARTESIAN_POINT ( 'NONE',  ( -113.5228709571500758, -24.33927499327855770, 9.819080762295806508 ) ) ;
#83278 = CARTESIAN_POINT ( 'NONE',  ( -65.52287095715010423, -24.14406661686763300, 10.28769366194077151 ) ) ;
#83279 = CARTESIAN_POINT ( 'NONE',  ( -19.17877449816284496, 10.63638241594707345, -1.500000000000002220 ) ) ;
#83280 = CARTESIAN_POINT ( 'NONE',  ( -87.58323434392801232, -24.65952944569305316, 1.056160979905705455 ) ) ;
#83281 = ORIENTED_EDGE ( 'NONE', *, *, #48063, .T. ) ;
#83282 = CARTESIAN_POINT ( 'NONE',  ( -80.44905418446258238, -25.30553335704075124, 4.507974687363522470 ) ) ;
#83283 = EDGE_CURVE ( 'NONE', #18260, #50853, #15768, .T. ) ;
#83284 = CARTESIAN_POINT ( 'NONE',  ( -116.6228709571500559, -23.47593901973091235, -1.443836447538997536 ) ) ;
#83285 = DIRECTION ( 'NONE',  ( 0.000000000000000000, -1.000000000000000000, 0.000000000000000000 ) ) ;
#83286 = CARTESIAN_POINT ( 'NONE',  ( -10.19904455147402089, -23.73149922466213368, 6.147794833475636267 ) ) ;
#83287 = CARTESIAN_POINT ( 'NONE',  ( 21.27783752795556538, -0.9766432368044721812, -1.500000000000002220 ) ) ;
#83288 = CARTESIAN_POINT ( 'NONE',  ( 6.184520403203631389, 5.356774720514425603, -25.32021290018218451 ) ) ;
#83289 = CARTESIAN_POINT ( 'NONE',  ( -107.5199639939815484, -23.73791477778912551, 11.05961554403170055 ) ) ;
#83290 = CARTESIAN_POINT ( 'NONE',  ( 28.20688450243646272, -14.82721238576461609, -7.073367244510395224 ) ) ;
#83291 = DIRECTION ( 'NONE',  ( 0.7071067811865474617, 0.000000000000000000, 0.7071067811865474617 ) ) ;
#83293 = CARTESIAN_POINT ( 'NONE',  ( -79.62287095715009855, -24.50321055353803956, 9.387540953477525818 ) ) ;
#83292 = B_SPLINE_CURVE_WITH_KNOTS ( 'NONE', 3,
 ( #89090, #96692, #19566, #33292 ),
 .UNSPECIFIED., .F., .F.,
 ( 4, 4 ),
 ( 0.02877499693705111092, 0.02977574397781653295 ),
 .UNSPECIFIED. ) ;
#83294 = ORIENTED_EDGE ( 'NONE', *, *, #51037, .F. ) ;
#83295 = CARTESIAN_POINT ( 'NONE',  ( -98.90284052011273275, -25.24560384201612706, 6.309255790471715919 ) ) ;
#83296 = CARTESIAN_POINT ( 'NONE',  ( -17.52035102510334141, -8.822347199899118309, 11.49999999999999645 ) ) ;
#83297 = CARTESIAN_POINT ( 'NONE',  ( -125.6228709571500843, -25.00158670708909625, 2.256160236439166855 ) ) ;
#83298 = B_SPLINE_CURVE_WITH_KNOTS ( 'NONE', 3,
 ( #35978, #53215, #75525, #84143 ),
 .UNSPECIFIED., .F., .F.,
 ( 4, 4 ),
 ( 0.000000000000000000, 1.000000000000000000 ),
 .UNSPECIFIED. ) ;
#83299 = CARTESIAN_POINT ( 'NONE',  ( -16.22218391600152643, 6.376774720514426953, -54.85883559227303863 ) ) ;
#83300 = VERTEX_POINT ( 'NONE', #93388 ) ;
#83301 = CARTESIAN_POINT ( 'NONE',  ( -88.58842802440713626, -24.35071581493543746, 9.817618358456025263 ) ) ;
#83302 = CARTESIAN_POINT ( 'NONE',  ( -101.8581997900095502, -25.20156876886343866, 6.591836956137893111 ) ) ;
#83303 = CARTESIAN_POINT ( 'NONE',  ( -25.53098197642538736, -24.92569209777881056, 4.942811685741776984 ) ) ;
#83304 = CARTESIAN_POINT ( 'NONE',  ( -45.62287095715004881, -24.14321612903114556, -0.2833117244521596301 ) ) ;
#83305 = CARTESIAN_POINT ( 'NONE',  ( -13.01991350253972080, 14.82018230214031895, -1.500000000000002220 ) ) ;
#83306 = ORIENTED_EDGE ( 'NONE', *, *, #57130, .T. ) ;
#83307 = DIRECTION ( 'NONE',  ( -1.333806637208504346E-15, 6.669033186042521139E-15, -1.000000000000000000 ) ) ;
#83308 = DIRECTION ( 'NONE',  ( -0.7071067811865476838, 0.000000000000000000, 0.7071067811865474617 ) ) ;
#83309 = VECTOR ( 'NONE', #67012, 1000.000000000000000 ) ;
#83310 = SHAPE_DEFINITION_REPRESENTATION ( #56309, #50921 ) ;
#83311 = ADVANCED_FACE ( 'NONE', ( #50 ), #24882, .F. ) ;
#83312 = ORIENTED_EDGE ( 'NONE', *, *, #28012, .T. ) ;
#83313 = CARTESIAN_POINT ( 'NONE',  ( -96.55620429048340725, -24.64898659630528499, 1.056161002820828143 ) ) ;
#83314 = CARTESIAN_POINT ( 'NONE',  ( -45.62287095715004881, -25.00182538069145011, 7.747789668545099317 ) ) ;
#83315 = CARTESIAN_POINT ( 'NONE',  ( -55.54039504408765993, -24.52300882791530157, 0.6510814631126364826 ) ) ;
#83316 = CARTESIAN_POINT ( 'NONE',  ( -20.27875734969026311, 6.143225279485574397, 24.00402280011862288 ) ) ;
#83317 = DIRECTION ( 'NONE',  ( 0.000000000000000000, -0.9999999999976377785, -2.173523156925979128E-06 ) ) ;
#83318 = EDGE_CURVE ( 'NONE', #54301, #1762, #72160, .T. ) ;
#83319 = DIRECTION ( 'NONE',  ( -0.000000000000000000, 2.173523156925979552E-06, -0.9999999999976378895 ) ) ;
#83320 = EDGE_CURVE ( 'NONE', #55337, #76238, #78238, .T. ) ;
#83321 = LINE ( 'NONE', #37154, #68876 ) ;
#83322 = CARTESIAN_POINT ( 'NONE',  ( 15.90762396150235958, 12.10710967819287198, 11.49999999999998934 ) ) ;
#83323 = CIRCLE ( 'NONE', #67211, 1.399999999999998579 ) ;
#83324 = EDGE_CURVE ( 'NONE', #23469, #71932, #86287, .T. ) ;
#83325 = DIRECTION ( 'NONE',  ( 0.000000000000000000, 0.000000000000000000, 1.000000000000000000 ) ) ;
#83326 = CARTESIAN_POINT ( 'NONE',  ( -45.57860638382562257, -24.83644354573578283, 8.397322867130103674 ) ) ;
#83327 = ORIENTED_EDGE ( 'NONE', *, *, #40617, .F. ) ;
#83328 = CARTESIAN_POINT ( 'NONE',  ( -74.62287095715005592, -24.64898659630367561, 1.056161002820824368 ) ) ;
#83329 = CARTESIAN_POINT ( 'NONE',  ( 22.81105451610979173, 8.475225279485572472, -18.46691820600746681 ) ) ;
#83330 = EDGE_CURVE ( 'NONE', #46643, #18086, #4370, .T. ) ;
#83331 = CARTESIAN_POINT ( 'NONE',  ( -4.993225604111835914, 5.965225279485592225, -29.11654937215278593 ) ) ;
#83332 = CARTESIAN_POINT ( 'NONE',  ( -36.52287095715006870, -29.50247984919015209, -1.443849546365060466 ) ) ;
#83333 = DIRECTION ( 'NONE',  ( -0.000000000000000000, 1.000000000000000000, -0.000000000000000000 ) ) ;
#83334 = CARTESIAN_POINT ( 'NONE',  ( -39.60068863268012507, -23.96119346886879597, -0.6495511937832143534 ) ) ;
#83335 = B_SPLINE_CURVE_WITH_KNOTS ( 'NONE', 3,
 ( #43366, #83904, #14382, #61084, #59590, #20998 ),
 .UNSPECIFIED., .F., .F.,
 ( 4, 2, 4 ),
 ( 6.384118694779733475E-06, 0.001386860460836455327, 0.002767336802978130617 ),
 .UNSPECIFIED. ) ;
#83336 = LINE ( 'NONE', #60024, #90201 ) ;
#83337 = CARTESIAN_POINT ( 'NONE',  ( -51.69567503897438598, -25.31574286181298561, 4.127965101553169092 ) ) ;
#83338 = DIRECTION ( 'NONE',  ( -3.773278334453079030E-23, 0.9999999999976377785, 2.173523156925979128E-06 ) ) ;
#83339 = FACE_OUTER_BOUND ( 'NONE', #75010, .T. ) ;
#83340 = ORIENTED_EDGE ( 'NONE', *, *, #93453, .T. ) ;
#83341 = CARTESIAN_POINT ( 'NONE',  ( -18.13051092187696156, -9.059970205480309957, -1.500000000000002220 ) ) ;
#83342 = CARTESIAN_POINT ( 'NONE',  ( -122.5207654451141224, -23.96119346886880663, -0.6495511937832028071 ) ) ;
#83343 = DIRECTION ( 'NONE',  ( 1.000000000000000000, 0.000000000000000000, -2.168404344971008868E-16 ) ) ;
#83344 = CARTESIAN_POINT ( 'NONE',  ( -109.6228709571501128, -23.94994826722516379, -0.6494450866351683116 ) ) ;
#83345 = ORIENTED_EDGE ( 'NONE', *, *, #64608, .T. ) ;
#83346 = DIRECTION ( 'NONE',  ( -3.773278334453079618E-23, 0.9999999999976377785, 2.173523156925978705E-06 ) ) ;
#83347 = CARTESIAN_POINT ( 'NONE',  ( -46.52287095715005449, -24.33927499327854349, 9.819080762295813614 ) ) ;
#83348 = CARTESIAN_POINT ( 'NONE',  ( -15.22981678846565856, -13.14137338692033907, -1.500000000000002220 ) ) ;
#83349 = CARTESIAN_POINT ( 'NONE',  ( -3.607955376466517095, 20.77440192976073519, 11.49999999999999645 ) ) ;
#83350 = VECTOR ( 'NONE', #46371, 1000.000000000000000 ) ;
#83351 = CARTESIAN_POINT ( 'NONE',  ( -3.749999999999999112, 25.69999999999999574, 2.100000000000000089 ) ) ;
#83352 = CARTESIAN_POINT ( 'NONE',  ( -70.63480130512397182, -24.52399227489126687, 9.353111116836529959 ) ) ;
#83353 = CARTESIAN_POINT ( 'NONE',  ( 10.35204687333978057, 19.51823071965408829, 11.49999999999998934 ) ) ;
#83354 = CARTESIAN_POINT ( 'NONE',  ( -20.18818894172909140, 3.697778396234267184, 11.49999999999998934 ) ) ;
#83355 = LINE ( 'NONE', #20954, #30065 ) ;
#83356 = CARTESIAN_POINT ( 'NONE',  ( 31.10870921191468597, 5.152774720514429418, -4.748485609378566785 ) ) ;
#83357 = DIRECTION ( 'NONE',  ( -0.000000000000000000, 1.000000000000000000, -0.000000000000000000 ) ) ;
#83358 = ORIENTED_EDGE ( 'NONE', *, *, #56732, .T. ) ;
#83359 = CARTESIAN_POINT ( 'NONE',  ( -99.12380231474227799, -25.27434709648489886, 4.001575133896465353 ) ) ;
#83360 = B_SPLINE_SURFACE_WITH_KNOTS ( 'NONE', 3, 1, ( 
 ( #60266, #6461 ),
 ( #99300, #21176 ),
 ( #12572, #21662 ),
 ( #60760, #91189 ),
 ( #59256, #82089 ),
 ( #43536, #59763 ),
 ( #52637, #74473 ) ),
 .UNSPECIFIED., .F., .F., .F.,
 ( 4, 1, 1, 1, 4 ),
 ( 2, 2 ),
 ( 0.3452202732246780759, 0.4949101844912719983, 0.6446000957578658097, 0.7942900070244596211, 0.9439799182910535436 ),
 ( 0.000000000000000000, 1.000000000000000000 ),
 .UNSPECIFIED. ) ;
#83361 = CARTESIAN_POINT ( 'NONE',  ( -72.62287095715005592, -24.64965695001468404, 8.947790433994184056 ) ) ;
#83362 = ORIENTED_EDGE ( 'NONE', *, *, #97147, .T. ) ;
#83363 = ORIENTED_EDGE ( 'NONE', *, *, #11638, .F. ) ;
#83364 = DIRECTION ( 'NONE',  ( 0.1478094111296165691, -0.9890158633619158257, 6.377659838150018832E-17 ) ) ;
#83365 = DIRECTION ( 'NONE',  ( -2.352173255807796549E-16, 3.728519047445511252E-18, 1.000000000000000000 ) ) ;
#83366 = FACE_OUTER_BOUND ( 'NONE', #84109, .T. ) ;
#83367 = CARTESIAN_POINT ( 'NONE',  ( 19.85042311639309531, 5.490197614093233369, -1.500000000000002220 ) ) ;
#83368 = CARTESIAN_POINT ( 'NONE',  ( -4.019545577234938882, 21.20919285897865336, 11.49999999999999645 ) ) ;
#83369 = VERTEX_POINT ( 'NONE', #40119 ) ;
#83370 = DIRECTION ( 'NONE',  ( -3.773278334453079030E-23, 0.9999999999976377785, 2.173523156925979128E-06 ) ) ;
#83371 = FACE_OUTER_BOUND ( 'NONE', #12117, .T. ) ;
#83372 = CARTESIAN_POINT ( 'NONE',  ( 19.81157572017019319, -10.35993776028809421, -1.500000000000002220 ) ) ;
#83373 = CARTESIAN_POINT ( 'NONE',  ( -48.62287095715004881, -23.48786465467241058, 11.44779295918254824 ) ) ;
#83374 = DIRECTION ( 'NONE',  ( -0.000000000000000000, 1.000000000000000000, -0.000000000000000000 ) ) ;
#83375 = ORIENTED_EDGE ( 'NONE', *, *, #41255, .F. ) ;
#83376 = DIRECTION ( 'NONE',  ( 0.000000000000000000, -1.000000000000000000, 0.000000000000000000 ) ) ;
#83377 = CARTESIAN_POINT ( 'NONE',  ( -49.63342129923848489, -24.35071581493542325, 9.817618358456035921 ) ) ;
#83378 = B_SPLINE_CURVE_WITH_KNOTS ( 'NONE', 3,
 ( #32177, #64164, #95085, #25570 ),
 .UNSPECIFIED., .F., .F.,
 ( 4, 4 ),
 ( 0.000000000000000000, 0.0001000000000000028644 ),
 .UNSPECIFIED. ) ;
#83379 = CARTESIAN_POINT ( 'NONE',  ( 18.69404101259207707, 9.334567778723176446, 11.49999999999998934 ) ) ;
#83380 = VERTEX_POINT ( 'NONE', #92390 ) ;
#83381 = EDGE_CURVE ( 'NONE', #17782, #73380, #1566, .T. ) ;
#83382 = CIRCLE ( 'NONE', #49440, 1.149999999999998135 ) ;
#83384 = VERTEX_POINT ( 'NONE', #63478 ) ;
#83383 = CARTESIAN_POINT ( 'NONE',  ( -86.59502635198218456, -23.96119346886881019, -0.6495511937831902616 ) ) ;
#83385 = VERTEX_POINT ( 'NONE', #30995 ) ;
#83386 = CARTESIAN_POINT ( 'NONE',  ( -100.5064008495685357, -24.83644354573578994, 8.397322867130101898 ) ) ;
#83387 = CARTESIAN_POINT ( 'NONE',  ( 13.68530018921192060, -16.06810839794082924, -1.500000000000002220 ) ) ;
#83388 = EDGE_CURVE ( 'NONE', #88394, #69866, #61159, .T. ) ;
#83389 = ORIENTED_EDGE ( 'NONE', *, *, #62590, .F. ) ;
#83390 = DIRECTION ( 'NONE',  ( 0.000000000000000000, 0.000000000000000000, -1.000000000000000000 ) ) ;
#83391 = FACE_OUTER_BOUND ( 'NONE', #29438, .T. ) ;
#83392 = CARTESIAN_POINT ( 'NONE',  ( 21.36706796925463792, 4.321743776461201669, -1.500000000000002220 ) ) ;
#83393 = CARTESIAN_POINT ( 'NONE',  ( -110.9909297185884327, -25.14264188228929697, 6.986250900936915365 ) ) ;
#83394 = CARTESIAN_POINT ( 'NONE',  ( -36.62287095715004170, -23.94994826722565406, -0.6494450866342751372 ) ) ;
#83395 = CARTESIAN_POINT ( 'NONE',  ( -84.58953762381672448, -24.64965694238407679, 8.947790433994653014 ) ) ;
#83396 = CARTESIAN_POINT ( 'NONE',  ( 20.88924836996103451, 6.054424527964996194, -1.500000000000002220 ) ) ;
#83397 = CARTESIAN_POINT ( 'NONE',  ( -71.53293015653792963, -25.31639593012666012, 5.453599084002859421 ) ) ;
#83399 = EDGE_LOOP ( 'NONE', ( #97835, #43352, #87160, #87871 ) ) ;
#83398 = CARTESIAN_POINT ( 'NONE',  ( -2.124831620219566730, 22.23837930986240607, 11.49999999999999645 ) ) ;
#83400 = CARTESIAN_POINT ( 'NONE',  ( -45.62287095715007013, -24.63287334234178871, 0.9662140553045390767 ) ) ;
#83401 = CARTESIAN_POINT ( 'NONE',  ( -69.62287095715005592, -23.47596703998600631, 11.44779298504227683 ) ) ;
#83402 = FACE_OUTER_BOUND ( 'NONE', #86885, .T. ) ;
#83403 = VERTEX_POINT ( 'NONE', #76653 ) ;
#83404 = VECTOR ( 'NONE', #81389, 1000.000000000000114 ) ;
#83405 = VERTEX_POINT ( 'NONE', #30494 ) ;
#83406 = ORIENTED_EDGE ( 'NONE', *, *, #54621, .T. ) ;
#83407 = CARTESIAN_POINT ( 'NONE',  ( -75.52287095715013265, -23.85196035786901447, -0.8779234886475122401 ) ) ;
#83408 = CARTESIAN_POINT ( 'NONE',  ( 32.42932432802503939, -6.376774720514426953, -0.2107846672978405389 ) ) ;
#83409 = CARTESIAN_POINT ( 'NONE',  ( -52.52287095715006870, -23.48786465467241058, 11.44779295918255002 ) ) ;
#83410 = CARTESIAN_POINT ( 'NONE',  ( -49.10457154551149728, -25.27419814425984512, 3.999772249604824914 ) ) ;
#83411 = CARTESIAN_POINT ( 'NONE',  ( 6.274899854645557440, -5.876774720514428729, 21.83451738260096775 ) ) ;
#83412 = CARTESIAN_POINT ( 'NONE',  ( -37.62287095715003460, -23.73934037231756378, 11.05740245334329863 ) ) ;
#83413 = CARTESIAN_POINT ( 'NONE',  ( -45.62287095715004881, -23.47596703998600276, 11.44779298504227505 ) ) ;
#83414 = ORIENTED_EDGE ( 'NONE', *, *, #77465, .F. ) ;
#83415 = CARTESIAN_POINT ( 'NONE',  ( -18.22486019313910077, 6.713856318530649681, 11.49999999999999645 ) ) ;
#83416 = CARTESIAN_POINT ( 'NONE',  ( -87.92287095715006728, -23.47596703998600631, 11.44779298504227860 ) ) ;
#83417 = VERTEX_POINT ( 'NONE', #7155 ) ;
#83418 = CARTESIAN_POINT ( 'NONE',  ( 3.450324536843889067, -5.876774720514404748, 18.60429515659643229 ) ) ;
#83419 = CARTESIAN_POINT ( 'NONE',  ( 3.398951772795901771, -5.876774720514403860, 18.23562605320997676 ) ) ;
#83420 = CARTESIAN_POINT ( 'NONE',  ( -116.5228709571501042, -23.47593901973090524, -1.443836447538996426 ) ) ;
#83421 = CARTESIAN_POINT ( 'NONE',  ( -65.62287095715005592, -29.50250786944525672, 11.44777988621623699 ) ) ;
#83422 = EDGE_CURVE ( 'NONE', #20204, #39807, #58864, .T. ) ;
#83423 = CARTESIAN_POINT ( 'NONE',  ( -19.07250549579359244, -4.594354733287289605, -1.500000000000002220 ) ) ;
#83424 = CARTESIAN_POINT ( 'NONE',  ( 8.160000000000000142, -9.652339641703484574, 0.003711184059992174607 ) ) ;
#83425 = ORIENTED_EDGE ( 'NONE', *, *, #10972, .F. ) ;
#83426 = VECTOR ( 'NONE', #71860, 1000.000000000000000 ) ;
#83427 = CARTESIAN_POINT ( 'NONE',  ( 0.7969447072908428797, -21.54811710690876225, 11.49999999999998934 ) ) ;
#83428 = CARTESIAN_POINT ( 'NONE',  ( 30.93860345374796594, -0.6647747205144264315, 19.84760796525321780 ) ) ;
#83429 = CARTESIAN_POINT ( 'NONE',  ( -70.61198345729647485, -25.12219137084317211, 7.066382252255097640 ) ) ;
#83431 = B_SPLINE_CURVE_WITH_KNOTS ( 'NONE', 3,
 ( #98179, #83960, #6830, #14440, #45412, #76335 ),
 .UNSPECIFIED., .F., .F.,
 ( 4, 2, 4 ),
 ( 0.000000000000000000, 0.001380764517854763665, 0.002761529035709527329 ),
 .UNSPECIFIED. ) ;
#83430 = CARTESIAN_POINT ( 'NONE',  ( -50.52287095715008292, -24.62226745350441703, 0.9660975649729551806 ) ) ;
#83432 = CARTESIAN_POINT ( 'NONE',  ( -99.72418814851606328, -25.18439392545337796, 3.555267871858176942 ) ) ;
#83433 = CARTESIAN_POINT ( 'NONE',  ( 3.314627170985911420, 22.80399709308638023, -1.500000000000002220 ) ) ;
#83434 = PERSON_AND_ORGANIZATION ( #70597, #27821 ) ;
#83435 = CARTESIAN_POINT ( 'NONE',  ( 32.53135143123563466, 5.965225279485572685, 6.926385399448451885 ) ) ;
#83436 = DIRECTION ( 'NONE',  ( -3.773278334453079030E-23, 0.9999999999976377785, 2.173523156925979128E-06 ) ) ;
#83437 = CARTESIAN_POINT ( 'NONE',  ( 14.76687977769557847, -13.71354340032049457, 11.49999999999999645 ) ) ;
#83438 = CARTESIAN_POINT ( 'NONE',  ( -84.62287095715008434, -23.47596703998600631, 11.44779298504227860 ) ) ;
#83439 = CARTESIAN_POINT ( 'NONE',  ( -52.52287095715006870, -29.50248528299804818, 1.056150453629033370 ) ) ;
#83440 = ADVANCED_FACE ( 'NONE', ( #38106 ), #26396, .T. ) ;
#83441 = CARTESIAN_POINT ( 'NONE',  ( 14.52511747680497933, -6.475225279485573360, -27.86035006098926559 ) ) ;
#83442 = CARTESIAN_POINT ( 'NONE',  ( -29.62287095715004881, -23.40875089534885589, 11.44779299594469713 ) ) ;
#83443 = CARTESIAN_POINT ( 'NONE',  ( -122.5228709571500048, -23.73934037231757443, 11.05740245334328087 ) ) ;
#83444 = CARTESIAN_POINT ( 'NONE',  ( -6.239078800006583769, 18.87631364486404806, -1.500000000000002220 ) ) ;
#83445 = ADVANCED_FACE ( 'NONE', ( #33011 ), #25892, .F. ) ;
#83446 = CARTESIAN_POINT ( 'NONE',  ( -113.5541410105945488, -24.15543982623907482, -0.2315651400026574047 ) ) ;
#83447 = CARTESIAN_POINT ( 'NONE',  ( 11.81298147481671279, -15.83112273922526470, -1.500000000000002220 ) ) ;
#83448 = LINE ( 'NONE', #44912, #76681 ) ;
#83449 = EDGE_CURVE ( 'NONE', #5568, #64035, #87796, .T. ) ;
#83450 = ADVANCED_FACE ( 'NONE', ( #96403 ), #33503, .F. ) ;
#83451 = CARTESIAN_POINT ( 'NONE',  ( -78.62287095715004170, -23.48786465467241413, 11.44779295918254469 ) ) ;
#83452 = CARTESIAN_POINT ( 'NONE',  ( -74.62287095715005592, -23.47596703998600631, 11.44779298504227860 ) ) ;
#83453 = CARTESIAN_POINT ( 'NONE',  ( -3.285303218690974525, -20.39892020120133154, 11.49999999999999645 ) ) ;
#83454 = CARTESIAN_POINT ( 'NONE',  ( -70.62287095715005592, -23.47593901973091235, -1.443836447539006196 ) ) ;
#83455 = ADVANCED_FACE ( 'NONE', ( #88803 ), #25389, .T. ) ;
#83456 = CARTESIAN_POINT ( 'NONE',  ( 31.13513474936813807, 4.540774720514427543, 3.331262582247328741 ) ) ;
#83457 = CARTESIAN_POINT ( 'NONE',  ( -106.5596206104284533, -23.48783264082477373, -1.443836473390085695 ) ) ;
#83458 = CARTESIAN_POINT ( 'NONE',  ( -13.93578158028743985, 17.96481793202167054, 11.49999999999999645 ) ) ;
#83459 = ORIENTED_EDGE ( 'NONE', *, *, #13599, .F. ) ;
#83460 = LINE ( 'NONE', #6838, #39752 ) ;
#83461 = CARTESIAN_POINT ( 'NONE',  ( -62.55620429048339304, -23.47593901973091235, -1.443836447539007972 ) ) ;
#83462 = CARTESIAN_POINT ( 'NONE',  ( 8.007726535620864894, 18.53121347637897287, 11.49999999999998934 ) ) ;
#83463 = EDGE_CURVE ( 'NONE', #15126, #98224, #18281, .T. ) ;
#83464 = CARTESIAN_POINT ( 'NONE',  ( -63.53936857308043074, -24.51314013834316796, 0.6176544820404160641 ) ) ;
#83465 = CIRCLE ( 'NONE', #75420, 1.699999999999999289 ) ;
#83466 = DIRECTION ( 'NONE',  ( 0.000000000000000000, 0.000000000000000000, 1.000000000000000000 ) ) ;
#83467 = ORIENTED_EDGE ( 'NONE', *, *, #3097, .F. ) ;
#83468 = AXIS2_PLACEMENT_3D ( 'NONE', #75739, #74750, #68650 ) ;
#83469 = ORIENTED_EDGE ( 'NONE', *, *, #58494, .F. ) ;
#83470 = CARTESIAN_POINT ( 'NONE',  ( 0.3545156366401029935, -5.876774720514413630, 20.17598923696321478 ) ) ;
#83471 = CARTESIAN_POINT ( 'NONE',  ( 21.34038654641452482, 8.310931564070170197, -1.500000000000002220 ) ) ;
#83472 = CARTESIAN_POINT ( 'NONE',  ( -29.48132452782988366, -24.42614700373432512, 0.6176547996449994749 ) ) ;
#83473 = CARTESIAN_POINT ( 'NONE',  ( -21.33164055427280914, -3.227942221655450972, -1.500000000000002220 ) ) ;
#83474 = DIRECTION ( 'NONE',  ( -3.773278334453079030E-23, 0.9999999999976377785, 2.173523156925979128E-06 ) ) ;
#83475 = DIRECTION ( 'NONE',  ( -1.526034937513432889E-15, 7.121496375062686157E-15, -1.000000000000000000 ) ) ;
#83476 = CARTESIAN_POINT ( 'NONE',  ( 5.579783289733251550, -20.15082174716252794, 11.49999999999999645 ) ) ;
#83477 = VERTEX_POINT ( 'NONE', #96903 ) ;
#83478 = CARTESIAN_POINT ( 'NONE',  ( -50.52287095715006160, -23.47596703998600631, 11.44779298504229104 ) ) ;
#83479 = CARTESIAN_POINT ( 'NONE',  ( 12.33731239738771102, -18.22686410513083288, 11.49999999999998934 ) ) ;
#83480 = CARTESIAN_POINT ( 'NONE',  ( -105.6242952428360127, -24.92592662359561473, 8.075495903017998245 ) ) ;
#83481 = CARTESIAN_POINT ( 'NONE',  ( -27.89469851781394283, -25.21724992210043581, 7.595245531572402342 ) ) ;
#83482 = ORIENTED_EDGE ( 'NONE', *, *, #15907, .F. ) ;
#83483 = CARTESIAN_POINT ( 'NONE',  ( 5.202077965628057576, 2.038091937962834166, 2.869745073849996442E-16 ) ) ;
#83484 = CARTESIAN_POINT ( 'NONE',  ( -90.54594762189722701, -24.63419186844611275, 9.035850630976923981 ) ) ;
#83485 = B_SPLINE_CURVE_WITH_KNOTS ( 'NONE', 3,
 ( #81584, #17679, #11068, #50629 ),
 .UNSPECIFIED., .F., .F.,
 ( 4, 4 ),
 ( 0.000000000000000000, 0.0005192307692307995826 ),
 .UNSPECIFIED. ) ;
#83486 = ORIENTED_EDGE ( 'NONE', *, *, #83931, .F. ) ;
#83487 = CARTESIAN_POINT ( 'NONE',  ( -72.64441443556766842, -23.73791477778911840, 11.05961554403170943 ) ) ;
#83488 = ORIENTED_EDGE ( 'NONE', *, *, #61215, .T. ) ;
#83489 = B_SPLINE_CURVE_WITH_KNOTS ( 'NONE', 3,
 ( #58104, #89533, #89039, #96154 ),
 .UNSPECIFIED., .F., .F.,
 ( 4, 4 ),
 ( 0.9411720679360631170, 0.9501784992081787617 ),
 .UNSPECIFIED. ) ;
#83490 = ORIENTED_EDGE ( 'NONE', *, *, #30978, .F. ) ;
#83491 = CARTESIAN_POINT ( 'NONE',  ( -40.49165087243459737, -25.29352311369862605, 5.543942880681965946 ) ) ;
#83492 = CARTESIAN_POINT ( 'NONE',  ( -92.52287095715006160, -29.50248528299804818, 1.056150453629040253 ) ) ;
#83493 = CARTESIAN_POINT ( 'NONE',  ( -36.56104621580127656, -23.73766607897670156, -1.055555164236459120 ) ) ;
#83494 = CARTESIAN_POINT ( 'NONE',  ( 2.554409723529738052, 20.22502395925995700, -1.500000000000002220 ) ) ;
#83495 = EDGE_CURVE ( 'NONE', #73557, #33030, #64489, .T. ) ;
#83496 = ORIENTED_EDGE ( 'NONE', *, *, #96739, .T. ) ;
#83497 = CARTESIAN_POINT ( 'NONE',  ( -3.085512303079157359, -6.376774720514415407, 19.95084900476495093 ) ) ;
#83498 = CARTESIAN_POINT ( 'NONE',  ( -30.62155233649869146, -24.14929313691197876, 10.49653219292474482 ) ) ;
#83499 = EDGE_CURVE ( 'NONE', #3731, #49859, #41993, .T. ) ;
#83500 = DIRECTION ( 'NONE',  ( 1.000000000000000000, 0.000000000000000000, 0.000000000000000000 ) ) ;
#83501 = CARTESIAN_POINT ( 'NONE',  ( -25.56006801123770700, -24.90049575466193232, 5.680075578843891471 ) ) ;
#83502 = EDGE_LOOP ( 'NONE', ( #1698, #46839, #68512, #42004 ) ) ;
#83503 = DIRECTION ( 'NONE',  ( -0.000000000000000000, 2.173523156925979552E-06, -0.9999999999976378895 ) ) ;
#83504 = CARTESIAN_POINT ( 'NONE',  ( -29.31102972132424966, -25.26247878080915399, 7.337442809714779024 ) ) ;
#83505 = VECTOR ( 'NONE', #19312, 1000.000000000000000 ) ;
#83506 = CARTESIAN_POINT ( 'NONE',  ( 6.705275102110877405, 19.67741782454948662, 11.49999999999998934 ) ) ;
#83508 = ADVANCED_FACE ( 'NONE', ( #41129 ), #10671, .F. ) ;
#83507 = ORIENTED_EDGE ( 'NONE', *, *, #42824, .F. ) ;
#83510 = ORIENTED_EDGE ( 'NONE', *, *, #42921, .T. ) ;
#83509 = CARTESIAN_POINT ( 'NONE',  ( 4.653846153846159517, -6.376774720514415407, 19.99999999999999289 ) ) ;
#83511 = CARTESIAN_POINT ( 'NONE',  ( 29.94037442937952065, -5.350967020813893527, 19.84760796525321425 ) ) ;
#83513 = EDGE_LOOP ( 'NONE', ( #71930, #48499, #7897, #52431 ) ) ;
#83512 = ADVANCED_FACE ( 'NONE', ( #89293 ), #11166, .T. ) ;
#83514 = ORIENTED_EDGE ( 'NONE', *, *, #63667, .T. ) ;
#83515 = LINE ( 'NONE', #21608, #57567 ) ;
#83516 = CARTESIAN_POINT ( 'NONE',  ( -50.55649023882089921, -25.27412228879126133, 2.837765180535595011 ) ) ;
#83517 = FACE_OUTER_BOUND ( 'NONE', #72644, .T. ) ;
#83518 = CARTESIAN_POINT ( 'NONE',  ( -86.52287095715007581, -24.50216790748203977, 0.6166512839542572788 ) ) ;
#83519 = LINE ( 'NONE', #52582, #80500 ) ;
#83521 = ORIENTED_EDGE ( 'NONE', *, *, #26868, .F. ) ;
#83520 = CARTESIAN_POINT ( 'NONE',  ( -22.05048665130746954, -1.834114841651104832, 11.49999999999999645 ) ) ;
#83522 = CARTESIAN_POINT ( 'NONE',  ( -108.5181468800120399, -23.96119346886881729, -0.6495511937831862648 ) ) ;
#83523 = CARTESIAN_POINT ( 'NONE',  ( 20.10346781357453949, 10.43426432342431553, 11.49999999999998934 ) ) ;
#83525 = ORIENTED_EDGE ( 'NONE', *, *, #43030, .F. ) ;
#83524 = CARTESIAN_POINT ( 'NONE',  ( -0.02075734969026423599, -5.965225279485572685, -0.08597719988137648983 ) ) ;
#83526 = B_SPLINE_CURVE_WITH_KNOTS ( 'NONE', 3,
 ( #15663, #8560, #45625, #14155 ),
 .UNSPECIFIED., .F., .F.,
 ( 4, 4 ),
 ( 0.000000000000000000, 9.999999999998897304E-05 ),
 .UNSPECIFIED. ) ;
#83527 = ORIENTED_EDGE ( 'NONE', *, *, #86871, .F. ) ;
#83528 = CARTESIAN_POINT ( 'NONE',  ( -29.52287095715006515, -23.38906523657919578, -1.443836447538998424 ) ) ;
#83529 = B_SPLINE_CURVE_WITH_KNOTS ( 'NONE', 3,
 ( #25414, #70591, #88321, #48771, #79697, #1591 ),
 .UNSPECIFIED., .F., .F.,
 ( 4, 2, 4 ),
 ( 6.391158118959990520E-06, 0.001387004593080781809, 0.002767618028042603730 ),
 .UNSPECIFIED. ) ;
#83530 = VECTOR ( 'NONE', #19051, 1000.000000000000114 ) ;
#83531 = APPROVAL ( #68107, 'UNSPECIFIED' ) ;
#83532 = CIRCLE ( 'NONE', #98155, 11.85241003308275864 ) ;
#83533 = CARTESIAN_POINT ( 'NONE',  ( -17.82723130383223165, -9.322377578706960932, 11.49999999999998934 ) ) ;
#83534 = LINE ( 'NONE', #45496, #13277 ) ;
#83535 = ORIENTED_EDGE ( 'NONE', *, *, #83242, .T. ) ;
#83536 = CARTESIAN_POINT ( 'NONE',  ( -89.52287095715006160, -23.48786465467241769, 11.44779295918254292 ) ) ;
#83537 = CARTESIAN_POINT ( 'NONE',  ( -16.35649155429130985, -15.18990082740072367, -1.500000000000002220 ) ) ;
#83538 = AXIS2_PLACEMENT_3D ( 'NONE', #52736, #14663, #38507 ) ;
#83539 = AXIS2_PLACEMENT_3D ( 'NONE', #20264, #53238, #13152 ) ;
#83540 = ORIENTED_EDGE ( 'NONE', *, *, #16038, .F. ) ;
#83541 = VERTEX_POINT ( 'NONE', #73573 ) ;
#83542 = CARTESIAN_POINT ( 'NONE',  ( -110.6228709571500701, -23.48786465467241769, 11.44779295918254114 ) ) ;
#83543 = DIRECTION ( 'NONE',  ( -0.000000000000000000, 1.000000000000000000, -0.000000000000000000 ) ) ;
#83544 = FACE_OUTER_BOUND ( 'NONE', #1289, .T. ) ;
#83545 = LINE ( 'NONE', #64991, #28757 ) ;
#83546 = CIRCLE ( 'NONE', #2597, 2.249999999999998668 ) ;
#83547 = CARTESIAN_POINT ( 'NONE',  ( 13.55016566187448923, -5.965225279485570908, -28.22449608469281657 ) ) ;
#83548 = CARTESIAN_POINT ( 'NONE',  ( -5.499840656826012975, 18.73951620154120334, 11.49999999999998934 ) ) ;
#83549 = CARTESIAN_POINT ( 'NONE',  ( 32.45853543194704116, 0.3587747205144265483, 9.169203677920338080 ) ) ;
#83550 = CARTESIAN_POINT ( 'NONE',  ( -10.41973078503355588, 18.78793304046337198, -1.500000000000002220 ) ) ;
#83551 = DIRECTION ( 'NONE',  ( -0.9161084732596779245, 5.365801633547208359E-16, 0.4009304992412300872 ) ) ;
#83552 = LINE ( 'NONE', #13534, #84308 ) ;
#83553 = DIRECTION ( 'NONE',  ( 1.000000000000000000, 0.000000000000000000, 0.000000000000000000 ) ) ;
#83554 = CARTESIAN_POINT ( 'NONE',  ( -6.082769120682566921, -21.99330073093985405, -1.500000000000002220 ) ) ;
#83555 = CARTESIAN_POINT ( 'NONE',  ( -96.63021412912847552, -24.15620529776628445, 10.23563542870660115 ) ) ;
#83556 = CARTESIAN_POINT ( 'NONE',  ( -127.6228709571500559, -23.47593901973091235, -1.443836447538995760 ) ) ;
#83557 = CARTESIAN_POINT ( 'NONE',  ( 15.90762396150235958, 12.10710967819287198, 11.49999999999999645 ) ) ;
#83558 = CARTESIAN_POINT ( 'NONE',  ( -64.58953762381673869, -24.64898659630528499, 1.056161002820823036 ) ) ;
#83559 = CARTESIAN_POINT ( 'NONE',  ( -74.60134804213069515, -23.73791477778911840, 11.05961554403170588 ) ) ;
#83560 = LINE ( 'NONE', #61252, #78048 ) ;
#83561 = EDGE_CURVE ( 'NONE', #84112, #44563, #71578, .T. ) ;
#83562 = EDGE_LOOP ( 'NONE', ( #968, #61149, #26645, #51930 ) ) ;
#83563 = DIRECTION ( 'NONE',  ( 0.000000000000000000, -2.173523156925980399E-06, 0.9999999999976378895 ) ) ;
#83564 = CARTESIAN_POINT ( 'NONE',  ( 10.46399479596578175, -3.400839389856524342, -27.03001098546515735 ) ) ;
#83565 = CARTESIAN_POINT ( 'NONE',  ( 18.95625057990686813, 10.65820999021175730, 11.49999999999998934 ) ) ;
#83566 = CARTESIAN_POINT ( 'NONE',  ( -0.02075734969026423599, -6.376774720514426953, -0.08597719988137648983 ) ) ;
#83567 = CARTESIAN_POINT ( 'NONE',  ( -11.98250242409135780, 15.54504917500377559, -1.500000000000002220 ) ) ;
#83568 = CARTESIAN_POINT ( 'NONE',  ( -99.36303409631229044, -25.22482018454191888, 6.487150432439984904 ) ) ;
#83569 = ORIENTED_EDGE ( 'NONE', *, *, #46466, .F. ) ;
#83570 = CALENDAR_DATE ( 2026, 9, 10 ) ;
#83571 = VECTOR ( 'NONE', #40679, 1000.000000000000000 ) ;
#83572 = ADVANCED_FACE ( 'NONE', ( #50239 ), #3071, .T. ) ;
#83573 = DIRECTION ( 'NONE',  ( -3.773278334444167608E-23, 1.000000000000000000, 0.000000000000000000 ) ) ;
#83574 = CARTESIAN_POINT ( 'NONE',  ( 3.398286024651508530, -6.376774720514429617, 21.76255057507181334 ) ) ;
#83575 = CARTESIAN_POINT ( 'NONE',  ( -7.951223608505463503, 18.87544906973805325, 11.49999999999999645 ) ) ;
#83576 = CARTESIAN_POINT ( 'NONE',  ( -28.49194798280534968, 6.376774720514426953, 28.38521343323375490 ) ) ;
#83577 = EDGE_CURVE ( 'NONE', #62364, #80236, #81179, .T. ) ;
#83578 = CARTESIAN_POINT ( 'NONE',  ( -88.52287095715006160, -23.47596703998600631, 11.44779298504228393 ) ) ;
#83579 = ORIENTED_EDGE ( 'NONE', *, *, #59491, .F. ) ;
#83580 = CARTESIAN_POINT ( 'NONE',  ( 31.48454476783385658, -4.132774720514426292, -1.134026763942596494 ) ) ;
#83581 = CARTESIAN_POINT ( 'NONE',  ( -39.74201634257447324, -25.28892478847090430, 3.555061831638682168 ) ) ;
#83582 = LINE ( 'NONE', #14574, #3076 ) ;
#83583 = EDGE_CURVE ( 'NONE', #53349, #27745, #2072, .T. ) ;
#83584 = CARTESIAN_POINT ( 'NONE',  ( -85.52287095715006160, -23.48783264082476663, -1.443836473390089470 ) ) ;
#83585 = ORIENTED_EDGE ( 'NONE', *, *, #84161, .T. ) ;
#83586 = CARTESIAN_POINT ( 'NONE',  ( 32.74409430443929381, 4.661791533294069367, -3.688467650547408994 ) ) ;
#83587 = CARTESIAN_POINT ( 'NONE',  ( -13.34915495237762251, 18.83725853537101358, 11.49999999999999645 ) ) ;
#83588 = CARTESIAN_POINT ( 'NONE',  ( -13.73562189146022661, -18.16285900770654393, -1.500000000000002220 ) ) ;
#83589 = CARTESIAN_POINT ( 'NONE',  ( 3.165726958143470160, -6.376774720514422512, 21.14296526391294506 ) ) ;
#83590 = CARTESIAN_POINT ( 'NONE',  ( -105.6228709571500843, -24.14321612903118464, -0.2833117244520867439 ) ) ;
#83591 = DIRECTION ( 'NONE',  ( 0.000000000000000000, -2.173523156925980399E-06, 0.9999999999976378895 ) ) ;
#83592 = CARTESIAN_POINT ( 'NONE',  ( -74.52287095715004739, -24.51387760970726148, 9.387446482453416507 ) ) ;
#83593 = CARTESIAN_POINT ( 'NONE',  ( -99.50663065733192525, -25.30157701748021637, 4.996268205051663358 ) ) ;
#83594 = CARTESIAN_POINT ( 'NONE',  ( -0.1377007522546883911, -21.91379463844567965, -1.500000000000002220 ) ) ;
#83595 = DIRECTION ( 'NONE',  ( 0.1489078231574191002, 6.845827386180410961E-16, -0.9888510809027407644 ) ) ;
#83596 = VECTOR ( 'NONE', #5479, 1000.000000000000114 ) ;
#83597 = B_SPLINE_CURVE_WITH_KNOTS ( 'NONE', 3,
 ( #96029, #18404, #71701, #25005 ),
 .UNSPECIFIED., .F., .F.,
 ( 4, 4 ),
 ( 0.000000000000000000, 1.000000000000000000 ),
 .UNSPECIFIED. ) ;
#83598 = FACE_OUTER_BOUND ( 'NONE', #56943, .T. ) ;
#83599 = CARTESIAN_POINT ( 'NONE',  ( -77.62287095715005592, -23.96127896941631619, -0.6493128931037820406 ) ) ;
#83600 = CARTESIAN_POINT ( 'NONE',  ( 1.949999999999999956, 0.1924999999999999489, 0.1925000000000000044 ) ) ;
#83601 = DIRECTION ( 'NONE',  ( -0.000000000000000000, -1.000000000000000000, -0.000000000000000000 ) ) ;
#83602 = CARTESIAN_POINT ( 'NONE',  ( -107.6228709571500985, -23.95044443724993144, 10.65354141964649592 ) ) ;
#83603 = EDGE_LOOP ( 'NONE', ( #31252, #73538, #96019, #49871 ) ) ;
#83604 = VECTOR ( 'NONE', #49362, 1000.000000000000000 ) ;
#83605 = CARTESIAN_POINT ( 'NONE',  ( -3.558151220431595707, 20.12126150705307381, 11.49999999999998934 ) ) ;
#83606 = EDGE_LOOP ( 'NONE', ( #69393, #13455, #17604, #44223, #7356 ) ) ;
#83607 = AXIS2_PLACEMENT_3D ( 'NONE', #37642, #6191, #99519 ) ;
#83608 = ORIENTED_EDGE ( 'NONE', *, *, #37342, .F. ) ;
#83609 = VERTEX_POINT ( 'NONE', #17785 ) ;
#83610 = ORIENTED_EDGE ( 'NONE', *, *, #19817, .F. ) ;
#83611 = EDGE_CURVE ( 'NONE', #95824, #33670, #66063, .T. ) ;
#83612 = CARTESIAN_POINT ( 'NONE',  ( -22.90524134523018773, 2.401388714834002069, 11.49999999999998934 ) ) ;
#83613 = CARTESIAN_POINT ( 'NONE',  ( -35.52287095715008292, -24.92579138211052481, 1.929029949967122182 ) ) ;
#83614 = B_SPLINE_CURVE_WITH_KNOTS ( 'NONE', 3,
 ( #5082, #19798, #28411, #50773, #81714, #36526 ),
 .UNSPECIFIED., .F., .F.,
 ( 4, 2, 4 ),
 ( 6.391158118972359742E-06, 0.001387004593080795036, 0.002767618028042617608 ),
 .UNSPECIFIED. ) ;
#83615 = CARTESIAN_POINT ( 'NONE',  ( -5.512817753899047268, 19.46650688538001361, -1.500000000000002220 ) ) ;
#83616 = VECTOR ( 'NONE', #99014, 1000.000000000000114 ) ;
#83617 = ORIENTED_EDGE ( 'NONE', *, *, #40993, .F. ) ;
#83618 = LINE ( 'NONE', #38449, #13645 ) ;
#83619 = FACE_OUTER_BOUND ( 'NONE', #66706, .T. ) ;
#83620 = VECTOR ( 'NONE', #24561, 1000.000000000000114 ) ;
#83621 = EDGE_CURVE ( 'NONE', #71750, #10167, #21276, .T. ) ;
#83622 = CARTESIAN_POINT ( 'NONE',  ( -128.2228709571500644, -23.47596703998600631, 11.44779298504227860 ) ) ;
#83623 = CARTESIAN_POINT ( 'NONE',  ( -99.59346001018235484, -23.96169478059713498, 10.65365249895717703 ) ) ;
#83625 = ORIENTED_EDGE ( 'NONE', *, *, #54736, .F. ) ;
#83624 = CARTESIAN_POINT ( 'NONE',  ( -8.434714792116727367, -19.68496499552307455, 11.49999999999999645 ) ) ;
#83626 = DIRECTION ( 'NONE',  ( -3.773278334444167608E-23, 1.000000000000000000, 0.000000000000000000 ) ) ;
#83627 = CARTESIAN_POINT ( 'NONE',  ( -94.52287095715009002, -23.73934037231757443, 11.05740245334328087 ) ) ;
#83628 = VERTEX_POINT ( 'NONE', #51230 ) ;
#83629 = CARTESIAN_POINT ( 'NONE',  ( -20.69558417703438025, 1.077208295497980250, 11.49999999999998934 ) ) ;
#83630 = EDGE_CURVE ( 'NONE', #35425, #22324, #37499, .T. ) ;
#83632 = EDGE_LOOP ( 'NONE', ( #89174, #84342, #6121, #13790, #25253, #16370, #18904, #53863, #71442 ) ) ;
#83631 = LINE ( 'NONE', #68416, #57269 ) ;
#83633 = ADVANCED_FACE ( 'NONE', ( #99389, #6047 ), #82669, .T. ) ;
#83634 = CARTESIAN_POINT ( 'NONE',  ( -28.62974205479175893, -24.36036647229939334, 0.6176551810875500204 ) ) ;
#83635 = VERTEX_POINT ( 'NONE', #83665 ) ;
#83636 = CARTESIAN_POINT ( 'NONE',  ( 3.879812756903532556, -6.376774720514401196, 18.16163344421570969 ) ) ;
#83637 = ORIENTED_EDGE ( 'NONE', *, *, #69069, .T. ) ;
#83638 = CARTESIAN_POINT ( 'NONE',  ( -1.027814097295878693, -20.98676634966329146, -1.500000000000002220 ) ) ;
#83639 = CARTESIAN_POINT ( 'NONE',  ( 21.83198049998918577, 2.282343850347359648, 11.49999999999999645 ) ) ;
#83640 = CARTESIAN_POINT ( 'NONE',  ( -37.64193247772556816, -24.15620529776627379, 10.23563542870660825 ) ) ;
#83641 = CARTESIAN_POINT ( 'NONE',  ( 13.09772080625096891, 18.35129493929886380, 11.49999999999998934 ) ) ;
#83642 = AXIS2_PLACEMENT_3D ( 'NONE', #93526, #14903, #91537 ) ;
#83643 = CARTESIAN_POINT ( 'NONE',  ( -9.893913718187896222, 18.50344063021147889, -1.500000000000002220 ) ) ;
#83644 = PLANE ( 'NONE',  #49667 ) ;
#83645 = LINE ( 'NONE', #52708, #48633 ) ;
#83646 = CARTESIAN_POINT ( 'NONE',  ( 17.51792015816173986, 5.965225279485572685, 29.01255224319336889 ) ) ;
#83647 = ORIENTED_EDGE ( 'NONE', *, *, #52855, .F. ) ;
#83648 = ORIENTED_EDGE ( 'NONE', *, *, #94324, .F. ) ;
#83649 = ORIENTED_EDGE ( 'NONE', *, *, #43655, .T. ) ;
#83650 = CARTESIAN_POINT ( 'NONE',  ( -68.52287095715007581, -23.47593901973090524, -1.443836447538997092 ) ) ;
#83651 = EDGE_CURVE ( 'NONE', #3492, #21600, #12657, .T. ) ;
#83652 = CARTESIAN_POINT ( 'NONE',  ( 4.075586527997184128, 21.15050231453075824, -1.500000000000002220 ) ) ;
#83653 = FACE_OUTER_BOUND ( 'NONE', #39643, .T. ) ;
#83654 = ORIENTED_EDGE ( 'NONE', *, *, #54633, .F. ) ;
#83655 = CARTESIAN_POINT ( 'NONE',  ( 6.686094007546604878, -20.02240253118446844, 11.49999999999998934 ) ) ;
#83656 = LINE ( 'NONE', #76530, #1197 ) ;
#83657 = CARTESIAN_POINT ( 'NONE',  ( -64.60983413518364671, -23.48783264082477018, -1.443836473390096353 ) ) ;
#83658 = EDGE_CURVE ( 'NONE', #4528, #39813, #45566, .T. ) ;
#83659 = CARTESIAN_POINT ( 'NONE',  ( -83.54730440395789515, -24.35071581493543036, 9.817618358456028815 ) ) ;
#83660 = DIRECTION ( 'NONE',  ( -3.773278334453079618E-23, 0.9999999999976377785, 2.173523156925979975E-06 ) ) ;
#83661 = CARTESIAN_POINT ( 'NONE',  ( -70.74026866089610621, -25.31511106678998502, 4.894904372220056921 ) ) ;
#83662 = CARTESIAN_POINT ( 'NONE',  ( 22.15222936869060177, 0.07132910108538677296, -1.500000000000002220 ) ) ;
#83663 = DIRECTION ( 'NONE',  ( 0.000000000000000000, 0.000000000000000000, -1.000000000000000000 ) ) ;
#83664 = EDGE_LOOP ( 'NONE', ( #59821, #7974, #43546, #46723, #22955, #40258 ) ) ;
#83665 = CARTESIAN_POINT ( 'NONE',  ( 30.09341516180546350, -2.682774720514426559, -13.89311774897855933 ) ) ;
#83666 = CARTESIAN_POINT ( 'NONE',  ( -59.52287095715006160, -23.47596703998600631, 11.44779298504228926 ) ) ;
#83667 = FACE_OUTER_BOUND ( 'NONE', #5169, .T. ) ;
#83668 = EDGE_CURVE ( 'NONE', #93720, #22199, #36494, .T. ) ;
#83669 = ADVANCED_FACE ( 'NONE', ( #52728 ), #32139, .T. ) ;
#83670 = VECTOR ( 'NONE', #24357, 1000.000000000000000 ) ;
#83671 = FACE_OUTER_BOUND ( 'NONE', #14961, .T. ) ;
#83672 = CARTESIAN_POINT ( 'NONE',  ( 19.43689267596983683, 0.5339526363925560792, 11.49999999999998934 ) ) ;
#83673 = CARTESIAN_POINT ( 'NONE',  ( 3.659817510876246960, 21.07357064420920878, -1.500000000000002220 ) ) ;
#83674 = CARTESIAN_POINT ( 'NONE',  ( -62.49492364790526722, -24.51314013834316441, 0.6176544820404141767 ) ) ;
#83675 = DIRECTION ( 'NONE',  ( -4.335561085774420994E-16, -0.000000000000000000, 1.000000000000000000 ) ) ;
#83676 = CARTESIAN_POINT ( 'NONE',  ( -117.6228709571500701, -24.66019654487199730, 8.947790411086121054 ) ) ;
#83677 = CARTESIAN_POINT ( 'NONE',  ( -36.62287095715007013, -23.73934037231756378, 11.05740245334329863 ) ) ;
#83678 = CARTESIAN_POINT ( 'NONE',  ( 2.978076788109338402, -22.46882643481310282, -1.500000000000002220 ) ) ;
#83679 = VECTOR ( 'NONE', #44791, 1000.000000000000000 ) ;
#83680 = VERTEX_POINT ( 'NONE', #1448 ) ;
#83681 = CARTESIAN_POINT ( 'NONE',  ( -128.6228709571500417, -24.65952944569305316, 1.056160979905707897 ) ) ;
#83682 = CARTESIAN_POINT ( 'NONE',  ( -122.6228709571500701, -23.48783264082479505, -1.443836473390058828 ) ) ;
#83683 = CARTESIAN_POINT ( 'NONE',  ( 19.60560811685724403, 2.727087469661350738, 11.49999999999999645 ) ) ;
#83684 = VECTOR ( 'NONE', #61331, 1000.000000000000000 ) ;
#83685 = DIRECTION ( 'NONE',  ( 0.9762960071199348056, 0.2164396139380966033, -0.000000000000000000 ) ) ;
#83686 = EDGE_CURVE ( 'NONE', #29751, #80660, #86169, .T. ) ;
#83687 = ORIENTED_EDGE ( 'NONE', *, *, #37014, .T. ) ;
#83688 = CARTESIAN_POINT ( 'NONE',  ( -53.62287095715005592, -23.47596703998600276, 11.44779298504227683 ) ) ;
#83689 = LINE ( 'NONE', #454, #91964 ) ;
#83690 = CARTESIAN_POINT ( 'NONE',  ( 3.837509532605410278, -21.31939230324424628, -1.500000000000002220 ) ) ;
#83691 = DIRECTION ( 'NONE',  ( -3.773278334453079618E-23, 0.9999999999976377785, 2.173523156925979975E-06 ) ) ;
#83693 = VECTOR ( 'NONE', #8463, 1000.000000000000114 ) ;
#83692 = CARTESIAN_POINT ( 'NONE',  ( 14.41255161864883583, -12.98630880007775268, -1.500000000000002220 ) ) ;
#83694 = CARTESIAN_POINT ( 'NONE',  ( -61.62287095715004881, -23.48783264082478439, -1.443836473390069042 ) ) ;
#83695 = CARTESIAN_POINT ( 'NONE',  ( -35.62287095715004881, -24.52232992886363050, 0.6492154411906073674 ) ) ;
#83696 = CARTESIAN_POINT ( 'NONE',  ( 19.75791096855702733, 1.210928449428283038, -1.500000000000002220 ) ) ;
#83697 = ORIENTED_EDGE ( 'NONE', *, *, #63376, .T. ) ;
#83698 = CARTESIAN_POINT ( 'NONE',  ( -18.23349369547262810, -8.965252873808195133, 11.49999999999999645 ) ) ;
#83699 = CARTESIAN_POINT ( 'NONE',  ( -80.57997298781928919, -25.00158670708910691, 2.256160236439221034 ) ) ;
#83700 = ADVANCED_FACE ( 'NONE', ( #70958, #7047 ), #31385, .T. ) ;
#83701 = CARTESIAN_POINT ( 'NONE',  ( 6.482958569640026703, 0.6681657214399144840, 19.30000000000000071 ) ) ;
#83702 = ADVANCED_FACE ( 'NONE', ( #38500 ), #53997, .T. ) ;
#83703 = EDGE_LOOP ( 'NONE', ( #55980, #8415, #43225, #47438 ) ) ;
#83704 = CARTESIAN_POINT ( 'NONE',  ( -0.1426030150137700958, -21.20389190742571373, -1.497999999999532816 ) ) ;
#83705 = DIRECTION ( 'NONE',  ( -3.773278334453080206E-23, 0.9999999999976377785, 2.173523156925979552E-06 ) ) ;
#83706 = CARTESIAN_POINT ( 'NONE',  ( 0.5964549592197740946, 8.529703308962702124, -1.700000000000008837 ) ) ;
#83707 = CARTESIAN_POINT ( 'NONE',  ( -95.62287095715009855, -24.83602698348160587, 1.605859176311266179 ) ) ;
#83708 = DIRECTION ( 'NONE',  ( -3.773278334453080206E-23, 0.9999999999976377785, 2.173523156925979975E-06 ) ) ;
#83709 = CARTESIAN_POINT ( 'NONE',  ( -13.75281105048956576, 14.62798779934380811, -1.500000000000002220 ) ) ;
#83710 = EDGE_CURVE ( 'NONE', #8399, #64351, #57611, .T. ) ;
#83711 = CARTESIAN_POINT ( 'NONE',  ( -85.52287095715004739, -24.99132157543166954, 2.256160258750667502 ) ) ;
#83712 = ORIENTED_EDGE ( 'NONE', *, *, #95965, .F. ) ;
#83713 = DIRECTION ( 'NONE',  ( 0.000000000000000000, 0.000000000000000000, 1.000000000000000000 ) ) ;
#83714 = AXIS2_PLACEMENT_3D ( 'NONE', #89247, #81635, #19715 ) ;
#83715 = EDGE_CURVE ( 'NONE', #90098, #93719, #53041, .T. ) ;
#83716 = EDGE_CURVE ( 'NONE', #881, #50095, #51372, .T. ) ;
#83717 = CARTESIAN_POINT ( 'NONE',  ( -22.76716317511769461, -1.676022972194794791, 11.49999999999999645 ) ) ;
#83718 = DIRECTION ( 'NONE',  ( 0.000000000000000000, 0.9999999999976377785, 2.173523156925979552E-06 ) ) ;
#83719 = CARTESIAN_POINT ( 'NONE',  ( -1.751198251822016161, 22.56127314141087581, 2.100000000000000089 ) ) ;
#83720 = CARTESIAN_POINT ( 'NONE',  ( -114.5228709571500616, -24.65952944569305316, 1.056160979905704123 ) ) ;
#83721 = VECTOR ( 'NONE', #48492, 1000.000000000000000 ) ;
#83722 = CARTESIAN_POINT ( 'NONE',  ( 5.642884982650352654, -5.876774720514425177, 20.85668005806743608 ) ) ;
#83723 = CARTESIAN_POINT ( 'NONE',  ( -95.62287095715005592, -29.50250786944525672, 11.44777988621623166 ) ) ;
#83724 = CARTESIAN_POINT ( 'NONE',  ( -108.6228709571500417, -24.65952944569305316, 1.056160979905705011 ) ) ;
#83725 = ORIENTED_EDGE ( 'NONE', *, *, #54638, .F. ) ;
#83726 = CARTESIAN_POINT ( 'NONE',  ( 20.12614038868121824, 2.982395457389826809, 11.49999999999998934 ) ) ;
#83727 = ORIENTED_EDGE ( 'NONE', *, *, #56281, .F. ) ;
#83728 = CARTESIAN_POINT ( 'NONE',  ( 22.85142058292489153, -2.183311388647848350, -1.500000000000002220 ) ) ;
#83729 = CARTESIAN_POINT ( 'NONE',  ( -28.98875734969026041, 5.965225279485572685, 17.86602280011862476 ) ) ;
#83730 = EDGE_LOOP ( 'NONE', ( #68754, #58759, #68488, #91842 ) ) ;
#83731 = CARTESIAN_POINT ( 'NONE',  ( -38.62287095715005592, -23.72747288104442021, -1.053458166803663554 ) ) ;
#83732 = AXIS2_PLACEMENT_3D ( 'NONE', #47765, #11197, #1085 ) ;
#83733 = CARTESIAN_POINT ( 'NONE',  ( -77.59611031647311563, -23.96169478059713498, 10.65365249895717703 ) ) ;
#83734 = CARTESIAN_POINT ( 'NONE',  ( -51.56024044797280226, -23.73791477778911840, 11.05961554403170766 ) ) ;
#83736 = ORIENTED_EDGE ( 'NONE', *, *, #93681, .T. ) ;
#83735 = CARTESIAN_POINT ( 'NONE',  ( -13.59518820711925358, -16.35513075224449864, 11.49999999999999645 ) ) ;
#83737 = VERTEX_POINT ( 'NONE', #16651 ) ;
#83738 = CARTESIAN_POINT ( 'NONE',  ( 19.92104321119709098, 9.795001720801039369, -1.500000000000002220 ) ) ;
#83739 = CARTESIAN_POINT ( 'NONE',  ( -7.658335995763069448, 19.15843701367676388, 11.49999999999998934 ) ) ;
#83740 = AXIS2_PLACEMENT_3D ( 'NONE', #10101, #96833, #73014 ) ;
#83741 = ORIENTED_EDGE ( 'NONE', *, *, #27450, .F. ) ;
#83742 = ORIENTED_EDGE ( 'NONE', *, *, #76787, .F. ) ;
#83743 = LINE ( 'NONE', #44201, #77093 ) ;
#83744 = CARTESIAN_POINT ( 'NONE',  ( 2.627412086454235851, -5.876774720514419847, 20.59155478446653831 ) ) ;
#83745 = ORIENTED_EDGE ( 'NONE', *, *, #87842, .F. ) ;
#83746 = AXIS2_PLACEMENT_3D ( 'NONE', #94634, #31739, #64215 ) ;
#83747 = AXIS2_PLACEMENT_3D ( 'NONE', #64720, #18505, #96142 ) ;
#83748 = ORIENTED_EDGE ( 'NONE', *, *, #38257, .T. ) ;
#83749 = CARTESIAN_POINT ( 'NONE',  ( -126.3656746162385645, -25.21753786267799313, 3.540021004441403996 ) ) ;
#83750 = LINE ( 'NONE', #22833, #5011 ) ;
#83751 = CARTESIAN_POINT ( 'NONE',  ( -19.76906661924035191, -6.534152953431121347, -1.500000000000002220 ) ) ;
#83752 = CARTESIAN_POINT ( 'NONE',  ( 21.79142754302170815, -0.6654467836950721527, 11.49999999999999645 ) ) ;
#83753 = CARTESIAN_POINT ( 'NONE',  ( -51.07287736509689324, -25.05542596678760603, 7.456204470533294604 ) ) ;
#83754 = CARTESIAN_POINT ( 'NONE',  ( -78.59598984800533117, -23.96169478059713498, 10.65365249895717881 ) ) ;
#83755 = CARTESIAN_POINT ( 'NONE',  ( 15.63351008929417318, -16.12541905121107177, -1.500000000000002220 ) ) ;
#83756 = VECTOR ( 'NONE', #66611, 1000.000000000000114 ) ;
#83757 = B_SPLINE_CURVE_WITH_KNOTS ( 'NONE', 3,
 ( #91771, #98384, #59852, #82670 ),
 .UNSPECIFIED., .F., .F.,
 ( 4, 4 ),
 ( 0.02980720907600921399, 0.03881364034812469915 ),
 .UNSPECIFIED. ) ;
#83758 = CARTESIAN_POINT ( 'NONE',  ( 32.95803010956177559, -3.605854314291305762, -13.01399263622904812 ) ) ;
#83759 = ORIENTED_EDGE ( 'NONE', *, *, #51229, .F. ) ;
#83760 = CARTESIAN_POINT ( 'NONE',  ( -10.54059822343757880, -5.876774720514426953, 22.82308057603841078 ) ) ;
#83761 = FACE_OUTER_BOUND ( 'NONE', #93589, .T. ) ;
#83762 = ORIENTED_EDGE ( 'NONE', *, *, #2489, .F. ) ;
#83763 = ORIENTED_EDGE ( 'NONE', *, *, #40388, .T. ) ;
#83764 = FACE_OUTER_BOUND ( 'NONE', #42882, .T. ) ;
#83765 = EDGE_LOOP ( 'NONE', ( #43864, #57655, #22575, #82627 ) ) ;
#83766 = ADVANCED_FACE ( 'NONE', ( #84163 ), #38595, .F. ) ;
#83767 = CARTESIAN_POINT ( 'NONE',  ( -16.81368161134402683, 13.12552177539105358, -1.500000000000002220 ) ) ;
#83768 = ORIENTED_EDGE ( 'NONE', *, *, #26761, .T. ) ;
#83769 = DIRECTION ( 'NONE',  ( -1.000000000000000000, -0.000000000000000000, -0.000000000000000000 ) ) ;
#83770 = CARTESIAN_POINT ( 'NONE',  ( -11.20027426441765961, 17.80179601997297212, 11.49999999999998934 ) ) ;
#83771 = CARTESIAN_POINT ( 'NONE',  ( -30.61204402015759740, -24.38902418599227673, 0.3015907515355735202 ) ) ;
#83772 = CARTESIAN_POINT ( 'NONE',  ( -113.5228709571500616, -24.64965694238408034, 8.947790433994192938 ) ) ;
#83773 = DIRECTION ( 'NONE',  ( -3.773278334453080206E-23, 0.9999999999976377785, 2.173523156925979975E-06 ) ) ;
#83774 = CARTESIAN_POINT ( 'NONE',  ( 11.09338859787202480, -18.89396691112096605, -1.500000000000002220 ) ) ;
#83775 = DIRECTION ( 'NONE',  ( 0.000000000000000000, -1.000000000000000000, 0.000000000000000000 ) ) ;
#83776 = EDGE_LOOP ( 'NONE', ( #74653, #50675, #43968, #28762 ) ) ;
#83777 = CARTESIAN_POINT ( 'NONE',  ( -122.5190326059218933, -24.51419770103158413, 9.386484678747169852 ) ) ;
#83778 = EDGE_CURVE ( 'NONE', #69852, #80312, #11051, .T. ) ;
#83779 = AXIS2_PLACEMENT_3D ( 'NONE', #55591, #70808, #63716 ) ;
#83780 = EDGE_CURVE ( 'NONE', #24356, #54444, #23804, .T. ) ;
#83781 = EDGE_CURVE ( 'NONE', #50554, #34695, #50119, .T. ) ;
#83782 = CARTESIAN_POINT ( 'NONE',  ( -120.5228709571500900, -24.14321612903119885, -0.2833117244520856892 ) ) ;
#83783 = CARTESIAN_POINT ( 'NONE',  ( -130.5728709571500588, -23.78087380709146004, 10.97511746239721298 ) ) ;
#83784 = EDGE_CURVE ( 'NONE', #57062, #884, #65366, .T. ) ;
#83785 = AXIS2_PLACEMENT_3D ( 'NONE', #96907, #11175, #57375 ) ;
#83786 = CARTESIAN_POINT ( 'NONE',  ( -10.25202023458897393, -22.90670518572982672, 9.440663514584137772 ) ) ;
#83787 = CARTESIAN_POINT ( 'NONE',  ( 12.11089201280794470, -17.53110042540249225, 11.49999999999998934 ) ) ;
#83788 = CARTESIAN_POINT ( 'NONE',  ( -112.5587146430100489, -23.48783264082478794, -1.443836473390061270 ) ) ;
#83789 = CARTESIAN_POINT ( 'NONE',  ( -27.68651082257923335, -24.97064402014857620, 2.274902934185277559 ) ) ;
#83790 = CARTESIAN_POINT ( 'NONE',  ( 15.31892417638225012, -3.658177093025726023, -28.50911884272268182 ) ) ;
#83791 = CARTESIAN_POINT ( 'NONE',  ( -100.6814946224345846, -25.31401921878175898, 5.197788989978544549 ) ) ;
#83792 = CARTESIAN_POINT ( 'NONE',  ( 8.471766090126642723, -20.80389698432254519, -1.500000000000002220 ) ) ;
#83793 = B_SPLINE_SURFACE_WITH_KNOTS ( 'NONE', 3, 3, ( 
 ( #30184, #9219, #30690, #44938 ),
 ( #92087, #61661, #53548, #32560 ),
 ( #84478, #14958, #92579, #40182 ),
 ( #45932, #63538, #69255, #17338 ),
 ( #94463, #71134, #75860, #6363 ),
 ( #24944, #55921, #86842, #37320 ),
 ( #79231, #52539, #9730, #33071 ) ),
 .UNSPECIFIED., .F., .F., .F.,
 ( 4, 3, 4 ),
 ( 4, 4 ),
 ( 0.0004766839783834332330, 0.1029713700210900112, 0.2054660560637965871 ),
 ( 0.9597381382339776890, 0.9611936842035376793 ),
 .UNSPECIFIED. ) ;
#83794 = CARTESIAN_POINT ( 'NONE',  ( -108.8764474181941040, -25.31476271379807841, 5.144092056987718209 ) ) ;
#83795 = EDGE_LOOP ( 'NONE', ( #70711, #61229, #85153, #12396 ) ) ;
#83797 = DIRECTION ( 'NONE',  ( 1.000000000000000000, 3.773278334444167608E-23, 8.201307833595939069E-29 ) ) ;
#83796 = B_SPLINE_CURVE_WITH_KNOTS ( 'NONE', 3,
 ( #9305, #64640, #39758, #70718 ),
 .UNSPECIFIED., .F., .F.,
 ( 4, 4 ),
 ( 0.6102216688345595275, 0.6192281001066749502 ),
 .UNSPECIFIED. ) ;
#83798 = CARTESIAN_POINT ( 'NONE',  ( 5.347671334029483248, -18.86178030415664963, 11.49999999999999645 ) ) ;
#83799 = CARTESIAN_POINT ( 'NONE',  ( -68.62287095715004170, -24.50216790748098816, 0.6166512839513629274 ) ) ;
#83800 = DIRECTION ( 'NONE',  ( -0.000000000000000000, 1.000000000000000000, -0.000000000000000000 ) ) ;
#83801 = EDGE_CURVE ( 'NONE', #82984, #57281, #70863, .T. ) ;
#83802 = ORIENTED_EDGE ( 'NONE', *, *, #82579, .T. ) ;
#83803 = B_SPLINE_CURVE_WITH_KNOTS ( 'NONE', 3,
 ( #28526, #43767, #43273, #36642, #81823, #74214, #98028, #82809 ),
 .UNSPECIFIED., .F., .F.,
 ( 4, 2, 2, 4 ),
 ( 0.000000000000000000, 0.0004967474533590028650, 0.0007451211800385037012, 0.0009934949067180044290 ),
 .UNSPECIFIED. ) ;
#83804 = CARTESIAN_POINT ( 'NONE',  ( -70.18625720459044715, -25.30468007125771379, 4.853999493951613786 ) ) ;
#83805 = CARTESIAN_POINT ( 'NONE',  ( -36.52287095715008292, -23.72773821059535848, 11.05748984161097326 ) ) ;
#83806 = CARTESIAN_POINT ( 'NONE',  ( -100.6373084487711225, -25.25095777383906892, 5.200261160962469376 ) ) ;
#83807 = VECTOR ( 'NONE', #66488, 1000.000000000000000 ) ;
#83808 = CARTESIAN_POINT ( 'NONE',  ( -122.5562042904834072, -23.47593901973091235, -1.443836447538997536 ) ) ;
#83810 = ADVANCED_FACE ( 'NONE', ( #25267 ), #72959, .F. ) ;
#83809 = CARTESIAN_POINT ( 'NONE',  ( -9.502044936771568473, -17.27029980899984452, -1.500000000000002220 ) ) ;
#83811 = ORIENTED_EDGE ( 'NONE', *, *, #52101, .F. ) ;
#83812 = CARTESIAN_POINT ( 'NONE',  ( 33.40725018382580913, -3.504198967030887069, -12.51830322776342008 ) ) ;
#83813 = CARTESIAN_POINT ( 'NONE',  ( -118.5228709571500758, -24.65952944569305316, 1.056160979905705899 ) ) ;
#83814 = B_SPLINE_CURVE_WITH_KNOTS ( 'NONE', 3,
 ( #94512, #165, #54962, #63081 ),
 .UNSPECIFIED., .F., .F.,
 ( 4, 4 ),
 ( 0.3600430223869087176, 0.3690494536590239738 ),
 .UNSPECIFIED. ) ;
#83815 = EDGE_CURVE ( 'NONE', #90352, #26998, #52745, .T. ) ;
#83816 = AXIS2_PLACEMENT_3D ( 'NONE', #32962, #94849, #17734 ) ;
#83817 = APPROVAL_DATE_TIME ( #92423, #59956 ) ;
#83818 = ORIENTED_EDGE ( 'NONE', *, *, #39671, .F. ) ;
#83819 = LINE ( 'NONE', #93422, #95332 ) ;
#83820 = CARTESIAN_POINT ( 'NONE',  ( -67.62287095715012697, -24.34917612406838572, 0.1852690917426630390 ) ) ;
#83821 = CARTESIAN_POINT ( 'NONE',  ( -98.89994392110364174, -25.03144904247453795, 6.299691620028943895 ) ) ;
#83822 = CARTESIAN_POINT ( 'NONE',  ( -49.55620429048337883, -24.64965694238574301, 8.947790433994201820 ) ) ;
#83823 = AXIS2_PLACEMENT_3D ( 'NONE', #14645, #93264, #7537 ) ;
#83824 = CARTESIAN_POINT ( 'NONE',  ( -69.88050735872322150, -25.24515064012728160, 5.413835170906579286 ) ) ;
#83825 = CARTESIAN_POINT ( 'NONE',  ( -91.52287095715006160, -23.47596703998600631, 11.44779298504228393 ) ) ;
#83826 = CARTESIAN_POINT ( 'NONE',  ( -8.876215969300202957, 17.89991547088461488, 11.49999999999998934 ) ) ;
#83827 = ADVANCED_FACE ( 'NONE', ( #2952 ), #64870, .F. ) ;
#83828 = DIRECTION ( 'NONE',  ( 0.000000000000000000, 0.000000000000000000, 1.000000000000000000 ) ) ;
#83829 = CARTESIAN_POINT ( 'NONE',  ( -45.65167645653958317, -24.15602025860896163, 10.28564288303535434 ) ) ;
#83830 = ORIENTED_EDGE ( 'NONE', *, *, #64364, .T. ) ;
#83831 = DIRECTION ( 'NONE',  ( 0.000000000000000000, 0.000000000000000000, 1.000000000000000000 ) ) ;
#83832 = EDGE_CURVE ( 'NONE', #38212, #46658, #94277, .T. ) ;
#83833 = CARTESIAN_POINT ( 'NONE',  ( -66.52287095715006160, -23.48783264082476663, -1.443836473390092134 ) ) ;
#83834 = CARTESIAN_POINT ( 'NONE',  ( -80.49976769349017047, -24.63419186844610920, 9.035850630976922204 ) ) ;
#83835 = CARTESIAN_POINT ( 'NONE',  ( 31.59111626279633711, -0.3587747205144265483, 16.27760796525321751 ) ) ;
#83836 = CARTESIAN_POINT ( 'NONE',  ( -81.54105079080106577, -24.65952944569304961, 1.056160979905703901 ) ) ;
#83837 = DIRECTION ( 'NONE',  ( -1.000000000000000000, -3.491481338843133355E-15, -2.352173255807796056E-16 ) ) ;
#83838 = CARTESIAN_POINT ( 'NONE',  ( -51.33061876479827390, -25.31574422701022087, 4.756068479901139234 ) ) ;
#83839 = DIRECTION ( 'NONE',  ( -1.000000000000000000, -3.773278334444166432E-23, -8.201307841325785021E-29 ) ) ;
#83840 = CARTESIAN_POINT ( 'NONE',  ( 5.326923076923078426, -6.376774720514420736, 20.76772836538461320 ) ) ;
#83841 = ORIENTED_EDGE ( 'NONE', *, *, #11851, .F. ) ;
#83842 = CARTESIAN_POINT ( 'NONE',  ( -5.286950244708777724, -19.55949958832428948, 11.49999999999998934 ) ) ;
#83843 = CARTESIAN_POINT ( 'NONE',  ( 27.53860345374808105, 5.356774720496559894, 19.84760796525321780 ) ) ;
#83844 = FACE_OUTER_BOUND ( 'NONE', #32219, .T. ) ;
#83845 = AXIS2_PLACEMENT_3D ( 'NONE', #62331, #54723, #38485 ) ;
#83846 = CARTESIAN_POINT ( 'NONE',  ( -99.62287095715005592, -23.72747288104441665, -1.053458166803661111 ) ) ;
#83847 = ORIENTED_EDGE ( 'NONE', *, *, #94951, .F. ) ;
#83848 = DIRECTION ( 'NONE',  ( 0.000000000000000000, 0.000000000000000000, 1.000000000000000000 ) ) ;
#83849 = B_SPLINE_CURVE_WITH_KNOTS ( 'NONE', 3,
 ( #95276, #96276, #73445, #58227 ),
 .UNSPECIFIED., .F., .F.,
 ( 4, 4 ),
 ( 0.000000000000000000, 0.0001000000000000028644 ),
 .UNSPECIFIED. ) ;
#83850 = CARTESIAN_POINT ( 'NONE',  ( -63.62287095715002749, -24.33832256526968862, 0.1851278514119841789 ) ) ;
#83851 = CARTESIAN_POINT ( 'NONE',  ( 5.780499401231428358, -19.25771307485560158, -1.500000000000002220 ) ) ;
#83852 = CARTESIAN_POINT ( 'NONE',  ( -12.45680796028966597, 17.00782699154285638, 11.49999999999999645 ) ) ;
#83853 = AXIS2_PLACEMENT_3D ( 'NONE', #65509, #19292, #50263 ) ;
#83854 = CARTESIAN_POINT ( 'NONE',  ( -100.4426124108961176, -29.50249842297920466, 7.101626040072651413 ) ) ;
#83855 = CARTESIAN_POINT ( 'NONE',  ( -22.12685673520133989, -0.1325007643398395663, -1.500000000000002220 ) ) ;
#83856 = CARTESIAN_POINT ( 'NONE',  ( 20.53815866822273861, -0.6333348845813139283, -1.500000000000002220 ) ) ;
#83857 = CARTESIAN_POINT ( 'NONE',  ( -35.58953762381672448, -24.99132157543083821, 2.256160258750496084 ) ) ;
#83858 = CARTESIAN_POINT ( 'NONE',  ( -20.77875734969026311, -5.356774720514425603, 0.7300228001186309656 ) ) ;
#83859 = EDGE_LOOP ( 'NONE', ( #26146, #31730, #79628, #34816, #31837, #31727, #34381, #13947, #68889 ) ) ;
#83860 = LINE ( 'NONE', #76726, #28231 ) ;
#83861 = EDGE_LOOP ( 'NONE', ( #70529, #99221, #11528, #9384 ) ) ;
#83862 = DIRECTION ( 'NONE',  ( -0.000000000000000000, 1.000000000000000000, -0.000000000000000000 ) ) ;
#83863 = DIRECTION ( 'NONE',  ( -0.9951627101165078093, 1.776356839400250267E-15, 0.09824042138329590335 ) ) ;
#83864 = ORIENTED_EDGE ( 'NONE', *, *, #97897, .T. ) ;
#83865 = ORIENTED_EDGE ( 'NONE', *, *, #97893, .T. ) ;
#83866 = CARTESIAN_POINT ( 'NONE',  ( -65.52287095715006160, -23.48783264082476308, -1.443836473390092578 ) ) ;
#83867 = LINE ( 'NONE', #6245, #6516 ) ;
#83868 = CARTESIAN_POINT ( 'NONE',  ( -19.77875734969026311, 3.316774720514426456, 27.45402280011862572 ) ) ;
#83869 = CARTESIAN_POINT ( 'NONE',  ( 18.09409571311175569, -9.955296453752364272, -1.500000000000002220 ) ) ;
#83870 = CARTESIAN_POINT ( 'NONE',  ( -19.98381242416700587, 8.274006965216138099, 11.49999999999999645 ) ) ;
#83871 = ORIENTED_EDGE ( 'NONE', *, *, #83896, .F. ) ;
#83872 = DIRECTION ( 'NONE',  ( -3.773278334453079030E-23, 0.9999999999976377785, 2.173523156925979128E-06 ) ) ;
#83873 = DIRECTION ( 'NONE',  ( -0.000000000000000000, 1.000000000000000000, -0.000000000000000000 ) ) ;
#83874 = CARTESIAN_POINT ( 'NONE',  ( 21.65046080595755740, -5.567969076317650590, -1.500000000000002220 ) ) ;
#83875 = VECTOR ( 'NONE', #22266, 1000.000000000000000 ) ;
#83876 = CARTESIAN_POINT ( 'NONE',  ( -62.52287095715004739, -24.34917612406836795, 0.1852690917426548511 ) ) ;
#83877 = LINE ( 'NONE', #75266, #85335 ) ;
#83878 = ORIENTED_EDGE ( 'NONE', *, *, #24626, .F. ) ;
#83879 = CARTESIAN_POINT ( 'NONE',  ( -0.02075734969026423599, 6.376774720514426953, -0.08597719988137648983 ) ) ;
#83880 = CARTESIAN_POINT ( 'NONE',  ( 6.424528460793287543, -6.376774720514413630, 19.73230822599986212 ) ) ;
#83881 = CARTESIAN_POINT ( 'NONE',  ( 8.468106961216914641, 19.09613275528424836, 11.49999999999998934 ) ) ;
#83882 = ORIENTED_EDGE ( 'NONE', *, *, #22255, .F. ) ;
#83884 = EDGE_LOOP ( 'NONE', ( #25985, #99210, #94762, #18418 ) ) ;
#83883 = CARTESIAN_POINT ( 'NONE',  ( -98.62287095715005592, -23.94994826722515668, -0.6494450866351687557 ) ) ;
#83886 = VERTEX_POINT ( 'NONE', #9545 ) ;
#83885 = PERSON ( 'NAUO-PER9', 'UNSPECIFIED', 'UNSPECIFIED', ('UNSPECIFIED'), ('UNSPECIFIED'), ('UNSPECIFIED') ) ;
#83887 = CARTESIAN_POINT ( 'NONE',  ( -109.5537012376542236, -24.15620529776628445, 10.23563542870660115 ) ) ;
#83888 = CARTESIAN_POINT ( 'NONE',  ( -12.37649675270136918, 17.12833386298736471, -1.500000000000002220 ) ) ;
#83889 = VERTEX_POINT ( 'NONE', #88181 ) ;
#83890 = CARTESIAN_POINT ( 'NONE',  ( -117.5912916562027419, -23.96119346886881019, -0.6495511937831995875 ) ) ;
#83892 = EDGE_CURVE ( 'NONE', #27379, #11225, #35857, .T. ) ;
#83891 = CARTESIAN_POINT ( 'NONE',  ( -100.4426124108961176, -25.26221318251349146, 7.101635256430813392 ) ) ;
#83893 = CARTESIAN_POINT ( 'NONE',  ( -8.334044162642690878, 20.12857247364870616, -1.500000000000002220 ) ) ;
#83894 = LINE ( 'NONE', #43851, #62704 ) ;
#83895 = VECTOR ( 'NONE', #79566, 1000.000000000000000 ) ;
#83896 = EDGE_CURVE ( 'NONE', #54031, #86922, #85436, .T. ) ;
#83897 = CARTESIAN_POINT ( 'NONE',  ( -36.62287095715006302, -23.72747288104469732, -1.053458166803227902 ) ) ;
#83898 = B_SPLINE_CURVE_WITH_KNOTS ( 'NONE', 3,
 ( #60399, #15193, #84201, #93310 ),
 .UNSPECIFIED., .F., .F.,
 ( 4, 4 ),
 ( 0.000000000000000000, 0.0001000000000000028644 ),
 .UNSPECIFIED. ) ;
#83899 = CARTESIAN_POINT ( 'NONE',  ( -27.61845239340658154, 5.965225279485594001, -10.37513603161905351 ) ) ;
#83900 = CARTESIAN_POINT ( 'NONE',  ( -18.42844947050907578, 11.51566461966115540, -1.500000000000002220 ) ) ;
#83901 = CARTESIAN_POINT ( 'NONE',  ( 0.000000000000000000, -6.943225279485572443, 0.000000000000000000 ) ) ;
#83903 = ORIENTED_EDGE ( 'NONE', *, *, #43321, .F. ) ;
#83902 = CARTESIAN_POINT ( 'NONE',  ( 13.91197278145025074, 17.48688927191260234, 11.49999999999999645 ) ) ;
#83904 = CARTESIAN_POINT ( 'NONE',  ( -33.52287095715004739, -23.73907113217656573, -1.053371485781500860 ) ) ;
#83905 = CARTESIAN_POINT ( 'NONE',  ( -85.49558110888244755, -25.00182538069147142, 7.747789668545045139 ) ) ;
#83906 = CARTESIAN_POINT ( 'NONE',  ( -68.62287095715005592, -24.65952944569304606, 1.056160979905698794 ) ) ;
#83907 = VERTEX_POINT ( 'NONE', #75422 ) ;
#83908 = EDGE_CURVE ( 'NONE', #7838, #67776, #62451, .T. ) ;
#83909 = EDGE_CURVE ( 'NONE', #95461, #23469, #74442, .T. ) ;
#83910 = ORIENTED_EDGE ( 'NONE', *, *, #18486, .F. ) ;
#83911 = EDGE_LOOP ( 'NONE', ( #781, #67430, #40431, #75007 ) ) ;
#83912 = CARTESIAN_POINT ( 'NONE',  ( 6.573941812937369455, 1.185825954564562440E-17, -0.2639660507643281639 ) ) ;
#83913 = CARTESIAN_POINT ( 'NONE',  ( 20.79131504077403747, 4.132458064796619368, 11.49999999999998934 ) ) ;
#83914 = CARTESIAN_POINT ( 'NONE',  ( -127.6228709571500559, -23.47593901973091235, -1.443836447538995760 ) ) ;
#83915 = CARTESIAN_POINT ( 'NONE',  ( -79.70355613134685768, -25.03138256630352387, 7.365681602826161800 ) ) ;
#83916 = CARTESIAN_POINT ( 'NONE',  ( -41.52287095715006870, -23.47593901973090169, -1.443836447538997092 ) ) ;
#83918 = CARTESIAN_POINT ( 'NONE',  ( 32.52533654608641456, 5.023480152701085721, -11.79063777444543781 ) ) ;
#83917 = B_SPLINE_CURVE_WITH_KNOTS ( 'NONE', 3,
 ( #88264, #18737, #42602, #89760, #74037, #26859 ),
 .UNSPECIFIED., .F., .F.,
 ( 4, 2, 4 ),
 ( 0.000000000000000000, 0.001380764517854764532, 0.002761529035709529064 ),
 .UNSPECIFIED. ) ;
#83919 = CARTESIAN_POINT ( 'NONE',  ( -84.62287095715005592, -29.50250243563736774, 8.947779886222141599 ) ) ;
#83920 = CARTESIAN_POINT ( 'NONE',  ( -45.62316515138000028, -23.48783264082476663, -1.443836473390103237 ) ) ;
#83921 = ORIENTED_EDGE ( 'NONE', *, *, #29037, .T. ) ;
#83922 = CARTESIAN_POINT ( 'NONE',  ( -7.499459838998954631, -17.95702976299720532, 11.49999999999999645 ) ) ;
#83923 = CARTESIAN_POINT ( 'NONE',  ( -69.52287095715006160, -24.64898659630367916, 1.056161002820824368 ) ) ;
#83924 = EDGE_LOOP ( 'NONE', ( #64220, #58008, #22982, #80521 ) ) ;
#83925 = DIRECTION ( 'NONE',  ( 0.7512896232465891000, 0.000000000000000000, 0.6599726524652351767 ) ) ;
#83926 = CARTESIAN_POINT ( 'NONE',  ( 3.052815417670126319, -6.376774720514406525, 18.46676085997033923 ) ) ;
#83927 = VECTOR ( 'NONE', #50108, 1000.000000000000000 ) ;
#83928 = DIRECTION ( 'NONE',  ( 0.000000000000000000, 1.000000000000000000, -0.000000000000000000 ) ) ;
#83929 = DIRECTION ( 'NONE',  ( -3.773278334453079618E-23, 0.9999999999976377785, 2.173523156925979975E-06 ) ) ;
#83931 = EDGE_CURVE ( 'NONE', #33363, #74029, #43505, .T. ) ;
#83930 = CARTESIAN_POINT ( 'NONE',  ( 14.10018531369908423, 13.67006465538575277, 11.49999999999998934 ) ) ;
#83932 = B_SPLINE_SURFACE_WITH_KNOTS ( 'NONE', 3, 3, ( 
 ( #98502, #13761, #98998, #29492 ),
 ( #37114, #91890, #99497, #60967 ),
 ( #74674, #53352, #91392, #90902 ),
 ( #75172, #13268, #14262, #44739 ),
 ( #69063, #52845, #36123, #60474 ),
 ( #92391, #68569, #67584, #5170 ),
 ( #67094, #37614, #76654, #7157 ) ),
 .UNSPECIFIED., .F., .F., .F.,
 ( 4, 3, 4 ),
 ( 4, 4 ),
 ( 0.7945040050992242531, 0.8970133687736501216, 0.9995227324480759901 ),
 ( 0.4596107907157971906, 0.4608357021111512686 ),
 .UNSPECIFIED. ) ;
#83933 = DIRECTION ( 'NONE',  ( -0.000000000000000000, 1.000000000000000000, 0.000000000000000000 ) ) ;
#83934 = ORIENTED_EDGE ( 'NONE', *, *, #61591, .T. ) ;
#83935 = CARTESIAN_POINT ( 'NONE',  ( -17.67581969798968444, -12.36387604476075097, -1.500000000000002220 ) ) ;
#83936 = CARTESIAN_POINT ( 'NONE',  ( -43.62287095715004881, -23.47593901973091235, -1.443836447539011525 ) ) ;
#83937 = CARTESIAN_POINT ( 'NONE',  ( 26.73860345374794178, 1.477225279485574028, 19.84760796525321425 ) ) ;
#83938 = LINE ( 'NONE', #69723, #41022 ) ;
#83939 = CARTESIAN_POINT ( 'NONE',  ( -100.2462005486704442, -25.18439338411695161, 3.306208445075104585 ) ) ;
#83940 = CARTESIAN_POINT ( 'NONE',  ( -23.02147672596084149, 0.6323230698326208765, -1.500000000000002220 ) ) ;
#83941 = PERSON_AND_ORGANIZATION ( #70597, #27821 ) ;
#83942 = CARTESIAN_POINT ( 'NONE',  ( -56.22287095715007155, -23.47596703998600276, 11.44779298504227860 ) ) ;
#83943 = CARTESIAN_POINT ( 'NONE',  ( -96.52287095715006160, -23.47596703998600631, 11.44779298504228215 ) ) ;
#83944 = CARTESIAN_POINT ( 'NONE',  ( -14.78635263257777233, 13.65558988533819473, 11.49999999999999645 ) ) ;
#83945 = CARTESIAN_POINT ( 'NONE',  ( -109.7637679387061809, -25.10927417198714906, 2.928686727655255062 ) ) ;
#83946 = DIRECTION ( 'NONE',  ( 0.000000000000000000, -1.000000000000000000, 4.297590679709308564E-16 ) ) ;
#83947 = CARTESIAN_POINT ( 'NONE',  ( -46.52287095715005449, -24.51283580621365843, 0.6167428607019604936 ) ) ;
#83948 = FACE_OUTER_BOUND ( 'NONE', #46100, .T. ) ;
#83949 = CARTESIAN_POINT ( 'NONE',  ( -110.7296117302316532, -25.29779169913011572, 3.360882835270145641 ) ) ;
#83950 = CARTESIAN_POINT ( 'NONE',  ( 12.81631318294326505, -15.22695477405695996, 11.49999999999998934 ) ) ;
#83951 = DIRECTION ( 'NONE',  ( 0.000000000000000000, 1.478457507934778393E-16, -1.000000000000000000 ) ) ;
#83952 = CARTESIAN_POINT ( 'NONE',  ( -14.06767371131996214, 13.90018863433869889, -1.500000000000002220 ) ) ;
#83953 = CIRCLE ( 'NONE', #22364, 2.249999999999998668 ) ;
#83954 = CARTESIAN_POINT ( 'NONE',  ( -126.6234820425866872, -24.66019654487200796, 8.947790411086103290 ) ) ;
#83955 = EDGE_CURVE ( 'NONE', #1549, #1657, #48191, .T. ) ;
#83956 = CARTESIAN_POINT ( 'NONE',  ( -0.6227173540047638012, -6.376774720514413630, 19.48351902941045211 ) ) ;
#83957 = B_SPLINE_CURVE_WITH_KNOTS ( 'NONE', 3,
 ( #28023, #44250, #96528, #59471, #28510, #35142 ),
 .UNSPECIFIED., .F., .F.,
 ( 4, 2, 4 ),
 ( 6.384118695446109541E-06, 0.001386860460836795116, 0.002767336802978144061 ),
 .UNSPECIFIED. ) ;
#83958 = CARTESIAN_POINT ( 'NONE',  ( -32.30247028140506416, -6.475225279485573360, 27.60502002861223048 ) ) ;
#83959 = CARTESIAN_POINT ( 'NONE',  ( -14.21563987850626276, 15.01860006206015008, 11.49999999999999645 ) ) ;
#83960 = CARTESIAN_POINT ( 'NONE',  ( -58.52287095715007581, -24.50216790748205398, 0.6166512839542500624 ) ) ;
#83961 = EDGE_CURVE ( 'NONE', #38812, #29553, #90168, .T. ) ;
#83962 = CARTESIAN_POINT ( 'NONE',  ( -79.52287095715006160, -23.47596703998600631, 11.44779298504228571 ) ) ;
#83963 = CARTESIAN_POINT ( 'NONE',  ( 1.118074629359579797, -22.68859683979520980, 11.49999999999999645 ) ) ;
#83964 = EDGE_LOOP ( 'NONE', ( #33934, #92732, #82903, #67876 ) ) ;
#83965 = CARTESIAN_POINT ( 'NONE',  ( 3.421177667410919110, -6.376774720514426953, 28.69411518427638441 ) ) ;
#83966 = CARTESIAN_POINT ( 'NONE',  ( -74.62287095715004170, -24.66019654487199375, 8.947790411086129936 ) ) ;
#83967 = AXIS2_PLACEMENT_3D ( 'NONE', #58403, #72625, #10719 ) ;
#83968 = CARTESIAN_POINT ( 'NONE',  ( -18.82377384687745447, 7.257840063761761051, 11.49999999999998934 ) ) ;
#83969 = CARTESIAN_POINT ( 'NONE',  ( -63.56611337692685737, -23.48783264082476308, -1.443836473390093245 ) ) ;
#83970 = CARTESIAN_POINT ( 'NONE',  ( -54.62287095715005592, -29.50250243563736774, 8.947779886222146928 ) ) ;
#83971 = ORIENTED_EDGE ( 'NONE', *, *, #92093, .F. ) ;
#83972 = EDGE_LOOP ( 'NONE', ( #37817, #48058, #72924, #13021 ) ) ;
#83973 = CARTESIAN_POINT ( 'NONE',  ( -0.2112149364088803105, -5.876774720514410077, 19.49357334786886398 ) ) ;
#83974 = CARTESIAN_POINT ( 'NONE',  ( 21.34038654641452482, 8.310931564070170197, 11.49999999999998934 ) ) ;
#83975 = CARTESIAN_POINT ( 'NONE',  ( -50.83488094104556154, -25.27420580424551133, 3.373740132572621953 ) ) ;
#83976 = CARTESIAN_POINT ( 'NONE',  ( 7.043455336710909620, -20.48365140995157674, -1.500000000000002220 ) ) ;
#83977 = AXIS2_PLACEMENT_3D ( 'NONE', #3608, #55899, #10712 ) ;
#83978 = DIRECTION ( 'NONE',  ( 0.000000000000000000, 2.173523156925980399E-06, -0.9999999999976378895 ) ) ;
#83979 = CARTESIAN_POINT ( 'NONE',  ( -23.24941632505786870, -6.376774720514426953, 27.45402280011862572 ) ) ;
#83980 = CARTESIAN_POINT ( 'NONE',  ( -17.10473743203234775, -12.04273770408705246, 11.49999999999999645 ) ) ;
#83981 = VERTEX_POINT ( 'NONE', #20148 ) ;
#83982 = FACE_OUTER_BOUND ( 'NONE', #73919, .T. ) ;
#83983 = CARTESIAN_POINT ( 'NONE',  ( -15.01370250125036421, 16.05796621403891677, -1.500000000000002220 ) ) ;
#83984 = CARTESIAN_POINT ( 'NONE',  ( -105.6347233272999944, -23.85049219812686871, 10.88485053497526955 ) ) ;
#83985 = CARTESIAN_POINT ( 'NONE',  ( -41.82812249501711932, -25.10925988035710077, 3.843615596726369432 ) ) ;
#83986 = ORIENTED_EDGE ( 'NONE', *, *, #85580, .F. ) ;
#83987 = B_SPLINE_CURVE_WITH_KNOTS ( 'NONE', 3,
 ( #43337, #27611, #74276, #4767 ),
 .UNSPECIFIED., .F., .F.,
 ( 4, 4 ),
 ( 0.000000000000000000, 0.0001000000000000028644 ),
 .UNSPECIFIED. ) ;
#83988 = CARTESIAN_POINT ( 'NONE',  ( 4.740341618695937065, -6.376774720514404748, 18.75174579344860248 ) ) ;
#83989 = FACE_OUTER_BOUND ( 'NONE', #77400, .T. ) ;
#83990 = VERTEX_POINT ( 'NONE', #35881 ) ;
#83991 = PLANE ( 'NONE',  #98732 ) ;
#83992 = ORIENTED_EDGE ( 'NONE', *, *, #6645, .F. ) ;
#83993 = VERTEX_POINT ( 'NONE', #52604 ) ;
#83994 = CARTESIAN_POINT ( 'NONE',  ( -59.52287095715009002, -23.47593901973090524, -1.443836447538997092 ) ) ;
#83995 = CARTESIAN_POINT ( 'NONE',  ( -2.794871794871795156, -6.376774720514417183, 20.36318108974359475 ) ) ;
#83996 = CARTESIAN_POINT ( 'NONE',  ( -57.59300200441531103, -24.15543982623907127, -0.2315651400026663420 ) ) ;
#83997 = CARTESIAN_POINT ( 'NONE',  ( 0.3735783541106268979, -20.45636175344465713, -1.500000000000002220 ) ) ;
#83998 = B_SPLINE_CURVE_WITH_KNOTS ( 'NONE', 3,
 ( #76177, #68585, #77674, #60980, #83799, #14279 ),
 .UNSPECIFIED., .F., .F.,
 ( 4, 2, 4 ),
 ( 0.000000000000000000, 0.001380764517853250118, 0.002761529035706500237 ),
 .UNSPECIFIED. ) ;
#83999 = ORIENTED_EDGE ( 'NONE', *, *, #75926, .F. ) ;
#84000 = CARTESIAN_POINT ( 'NONE',  ( -93.58953762381672448, -24.64965694238575011, 8.947790433994196491 ) ) ;
#84001 = CARTESIAN_POINT ( 'NONE',  ( 8.160000000000000142, 7.891155995661686795, 5.788828319098143993 ) ) ;
#84002 = CARTESIAN_POINT ( 'NONE',  ( -98.62287095715004170, -24.65952944569304606, 1.056160979905700792 ) ) ;
#84003 = CARTESIAN_POINT ( 'NONE',  ( -25.77888769185907947, -24.80838911334880592, 6.758736707713437930 ) ) ;
#84004 = EDGE_LOOP ( 'NONE', ( #2154, #56032, #32863, #98259 ) ) ;
#84005 = LINE ( 'NONE', #29725, #79232 ) ;
#84006 = CARTESIAN_POINT ( 'NONE',  ( -64.62287095715005592, -23.48786465467241413, 11.44779295918254824 ) ) ;
#84007 = CARTESIAN_POINT ( 'NONE',  ( 13.57807927624399902, 15.74560944506941951, 11.49999999999998934 ) ) ;
#84008 = VERTEX_POINT ( 'NONE', #58720 ) ;
#84010 = VERTEX_POINT ( 'NONE', #98260 ) ;
#84009 = DIRECTION ( 'NONE',  ( -1.000000000000000000, 0.000000000000000000, 0.000000000000000000 ) ) ;
#84011 = B_SPLINE_SURFACE_WITH_KNOTS ( 'NONE', 3, 3, ( 
 ( #90136, #51580, #81031, #73422 ),
 ( #3920, #65824, #80672, #71573 ),
 ( #42628, #58352, #3065, #19263 ),
 ( #10666, #17780, #56361, #88798 ),
 ( #89288, #73566, #41628, #72570 ),
 ( #95399, #34005, #65980, #87279 ),
 ( #19754, #50730, #49248, #64981 ) ),
 .UNSPECIFIED., .F., .F., .F.,
 ( 4, 3, 4 ),
 ( 4, 4 ),
 ( 0.0004766839783821298594, 0.1029713700210898308, 0.2054660560637975308 ),
 ( 0.2895676583132508197, 0.2907139888547707884 ),
 .UNSPECIFIED. ) ;
#84012 = CARTESIAN_POINT ( 'NONE',  ( -50.56357725185049645, -25.12217861855133094, 7.098062342091831844 ) ) ;
#84013 = EDGE_LOOP ( 'NONE', ( #48108, #67595, #57963, #5870 ) ) ;
#84014 = EDGE_LOOP ( 'NONE', ( #27624, #97712, #4019, #3512 ) ) ;
#84015 = LINE ( 'NONE', #14503, #5752 ) ;
#84017 = EDGE_CURVE ( 'NONE', #32236, #65202, #38159, .T. ) ;
#84016 = CARTESIAN_POINT ( 'NONE',  ( -55.62287095715004170, -23.47596703998600631, 11.44779298504227505 ) ) ;
#84018 = CARTESIAN_POINT ( 'NONE',  ( 14.43441819135929194, -3.316774720514426456, -28.36222020317710957 ) ) ;
#84019 = CARTESIAN_POINT ( 'NONE',  ( -100.4498239493576506, -25.03152449170482186, 7.563174219377576613 ) ) ;
#84020 = CARTESIAN_POINT ( 'NONE',  ( -92.59142756244220607, -24.15620529776628445, 10.23563542870660292 ) ) ;
#84021 = PLANE ( 'NONE',  #52987 ) ;
#84023 = VERTEX_POINT ( 'NONE', #51112 ) ;
#84022 = CARTESIAN_POINT ( 'NONE',  ( 21.13975321936677787, -6.629177502137091338, 11.49999999999999645 ) ) ;
#84024 = DIRECTION ( 'NONE',  ( 0.000000000000000000, 0.000000000000000000, -1.000000000000000000 ) ) ;
#84025 = ADVANCED_FACE ( 'NONE', ( #52110 ), #12537, .T. ) ;
#84026 = CARTESIAN_POINT ( 'NONE',  ( -22.43363504178351775, 2.973318333978472339, 11.49999999999998934 ) ) ;
#84027 = VECTOR ( 'NONE', #19563, 1000.000000000000000 ) ;
#84028 = EDGE_CURVE ( 'NONE', #83477, #52082, #23603, .T. ) ;
#84030 = EDGE_LOOP ( 'NONE', ( #69670, #84632, #56690, #98458 ) ) ;
#84029 = CARTESIAN_POINT ( 'NONE',  ( -80.52287095715006160, -24.99156044556202616, 7.747789690856173195 ) ) ;
#84031 = EDGE_CURVE ( 'NONE', #61594, #91753, #21140, .T. ) ;
#84032 = ORIENTED_EDGE ( 'NONE', *, *, #88185, .F. ) ;
#84033 = B_SPLINE_CURVE_WITH_KNOTS ( 'NONE', 3,
 ( #31708, #14975, #255, #38314 ),
 .UNSPECIFIED., .F., .F.,
 ( 4, 4 ),
 ( 3.706435412536978550E-09, 0.0004668278787522539683 ),
 .UNSPECIFIED. ) ;
#84034 = EDGE_CURVE ( 'NONE', #9262, #85354, #606, .T. ) ;
#84035 = CARTESIAN_POINT ( 'NONE',  ( 7.160000000000000142, 7.891155995661682354, 6.788828319098143993 ) ) ;
#84036 = CARTESIAN_POINT ( 'NONE',  ( 6.436487395234643749, 19.08016507665710648, -1.500000000000002220 ) ) ;
#84037 = B_SPLINE_CURVE_WITH_KNOTS ( 'NONE', 3,
 ( #7655, #84272, #36605, #85270, #46727, #45230, #76153, #7148, #92383, #91883, #6652, #75652 ),
 .UNSPECIFIED., .F., .F.,
 ( 4, 2, 2, 2, 2, 4 ),
 ( 0.000000000000000000, 0.0001590846665151804601, 0.0003181693330303609203, 0.0006363386660606980966, 0.0009545079990910353271, 0.001272677332121372558 ),
 .UNSPECIFIED. ) ;
#84038 = DIRECTION ( 'NONE',  ( 1.000000000000000000, -0.000000000000000000, 0.000000000000000000 ) ) ;
#84039 = EDGE_LOOP ( 'NONE', ( #21987, #44605, #61796, #72573 ) ) ;
#84040 = AXIS2_PLACEMENT_3D ( 'NONE', #32808, #78970, #16569 ) ;
#84041 = LINE ( 'NONE', #37871, #87662 ) ;
#84042 = CARTESIAN_POINT ( 'NONE',  ( 3.752539591237177508, -22.04708138622333635, -1.500000000000002220 ) ) ;
#84043 = EDGE_CURVE ( 'NONE', #23628, #55431, #96781, .T. ) ;
#84044 = ORIENTED_EDGE ( 'NONE', *, *, #43839, .T. ) ;
#84045 = ORIENTED_EDGE ( 'NONE', *, *, #45717, .F. ) ;
#84046 = LINE ( 'NONE', #39372, #72461 ) ;
#84047 = CARTESIAN_POINT ( 'NONE',  ( -116.6228709571500559, -24.64965695001469115, 8.947790433994175174 ) ) ;
#84048 = DIRECTION ( 'NONE',  ( 0.000000000000000000, -1.000000000000000000, 0.000000000000000000 ) ) ;
#84049 = CARTESIAN_POINT ( 'NONE',  ( -96.62287095714999907, -24.51387760970724372, 9.387446482453412955 ) ) ;
#84050 = DIRECTION ( 'NONE',  ( 0.000000000000000000, 0.000000000000000000, 1.000000000000000000 ) ) ;
#84051 = CARTESIAN_POINT ( 'NONE',  ( 2.510080532074158377, -19.39449211012750496, -1.500000000000002220 ) ) ;
#84052 = LINE ( 'NONE', #14534, #10181 ) ;
#84053 = CARTESIAN_POINT ( 'NONE',  ( -17.67684169981329845, 12.20363403927300183, -1.500000000000002220 ) ) ;
#84054 = CARTESIAN_POINT ( 'NONE',  ( -25.53098197642538736, -24.92775386671257465, 4.942811681260474543 ) ) ;
#84055 = CARTESIAN_POINT ( 'NONE',  ( -120.5228709571500474, -24.63287334234178516, 0.9662140553045437397 ) ) ;
#84056 = LINE ( 'NONE', #99276, #71960 ) ;
#84057 = CARTESIAN_POINT ( 'NONE',  ( -15.36296916364455711, -16.94538937337987150, -1.500000000000002220 ) ) ;
#84058 = PERSON_AND_ORGANIZATION_ROLE ( 'classification_officer' ) ;
#84059 = DIRECTION ( 'NONE',  ( -1.000000000000000000, -3.773278334444166432E-23, -8.201307841325785021E-29 ) ) ;
#84060 = FACE_OUTER_BOUND ( 'NONE', #53811, .T. ) ;
#84061 = CARTESIAN_POINT ( 'NONE',  ( -8.813339738934139689, -17.91118242276673911, 11.49999999999999645 ) ) ;
#84062 = DIRECTION ( 'NONE',  ( 1.000000000000000000, 3.773278334444166432E-23, 8.201307841325785021E-29 ) ) ;
#84063 = CARTESIAN_POINT ( 'NONE',  ( -74.55900445870243232, -23.73791477778911840, 11.05961554403170588 ) ) ;
#84064 = CARTESIAN_POINT ( 'NONE',  ( -75.52287095715007581, -23.47593901973090169, -1.443836447538996870 ) ) ;
#84065 = VERTEX_POINT ( 'NONE', #4934 ) ;
#84066 = DIRECTION ( 'NONE',  ( 0.000000000000000000, -2.173523156925979552E-06, 0.9999999999976378895 ) ) ;
#84067 = EDGE_CURVE ( 'NONE', #76987, #64340, #66851, .T. ) ;
#84068 = PLANE ( 'NONE',  #75024 ) ;
#84069 = CARTESIAN_POINT ( 'NONE',  ( -8.443908442993951269, 20.02826104456839218, -1.500000000000002220 ) ) ;
#84070 = DIRECTION ( 'NONE',  ( 3.773278334444166432E-23, -1.000000000000000000, 0.000000000000000000 ) ) ;
#84071 = CARTESIAN_POINT ( 'NONE',  ( -19.07250549579359244, -4.594354733287289605, -1.500000000000002220 ) ) ;
#84072 = LINE ( 'NONE', #51640, #24775 ) ;
#84073 = VERTEX_POINT ( 'NONE', #89175 ) ;
#84074 = DIRECTION ( 'NONE',  ( 0.06471892502635213928, -0.8378373432121152264, 0.5420701495772458633 ) ) ;
#84075 = CARTESIAN_POINT ( 'NONE',  ( -47.52287095715010423, -24.33927499327855770, 9.819080762295813614 ) ) ;
#84076 = CARTESIAN_POINT ( 'NONE',  ( -11.60840874443078263, -16.91462557209307960, 11.49999999999999645 ) ) ;
#84077 = FACE_OUTER_BOUND ( 'NONE', #59458, .T. ) ;
#84078 = FACE_OUTER_BOUND ( 'NONE', #34526, .T. ) ;
#84079 = B_SPLINE_CURVE_WITH_KNOTS ( 'NONE', 3,
 ( #2040, #31975, #55325, #56335, #62943 ),
 .UNSPECIFIED., .F., .F.,
 ( 4, 1, 4 ),
 ( 0.1431656576382807078, 0.2545924338564266032, 0.2890741368561012825 ),
 .UNSPECIFIED. ) ;
#84080 = ORIENTED_EDGE ( 'NONE', *, *, #43174, .F. ) ;
#84081 =( NAMED_UNIT ( * ) PLANE_ANGLE_UNIT ( ) SI_UNIT ( $, .RADIAN. ) );
#84082 = EDGE_CURVE ( 'NONE', #94218, #76361, #58235, .T. ) ;
#84083 = PLANE ( 'NONE',  #50786 ) ;
#84084 = CARTESIAN_POINT ( 'NONE',  ( 29.70220533433691301, 6.475225279485573360, 28.20564067601639735 ) ) ;
#84085 = FACE_OUTER_BOUND ( 'NONE', #77073, .T. ) ;
#84086 = VECTOR ( 'NONE', #79866, 1000.000000000000000 ) ;
#84087 = B_SPLINE_CURVE_WITH_KNOTS ( 'NONE', 3,
 ( #50779, #88841, #74596, #12692, #34551, #89829 ),
 .UNSPECIFIED., .F., .F.,
 ( 4, 2, 4 ),
 ( -8.871155308958663375E-06, 0.0009003829173646808823, 0.001809636990038320306 ),
 .UNSPECIFIED. ) ;
#84088 = EDGE_CURVE ( 'NONE', #57513, #44666, #27770, .T. ) ;
#84089 = CARTESIAN_POINT ( 'NONE',  ( 22.81105451610979173, -1.684774720501991618, -20.71691820600746681 ) ) ;
#84090 = CARTESIAN_POINT ( 'NONE',  ( 32.23945434255342235, 4.540774721353955989, 2.150384428877208709 ) ) ;
#84091 = AXIS2_PLACEMENT_3D ( 'NONE', #9830, #2736, #10838 ) ;
#84092 = CARTESIAN_POINT ( 'NONE',  ( -8.701767255460435280, 21.38705905713849020, 11.49999999999999645 ) ) ;
#84093 = CARTESIAN_POINT ( 'NONE',  ( -2.657479817400386413, -22.66247145590962120, -1.500000000000002220 ) ) ;
#84094 = CARTESIAN_POINT ( 'NONE',  ( -110.5169826798708925, -24.15602025860899360, 10.28564288303533480 ) ) ;
#84095 = CARTESIAN_POINT ( 'NONE',  ( -75.52287095715011844, -24.62285846331433703, 9.038163153548364193 ) ) ;
#84096 = CARTESIAN_POINT ( 'NONE',  ( -119.5228709571500758, -24.64898659630368627, 1.056161002820833028 ) ) ;
#84097 = VECTOR ( 'NONE', #51148, 1000.000000000000000 ) ;
#84098 = CARTESIAN_POINT ( 'NONE',  ( -119.5228709571500758, -29.50250243563736774, 8.947779886222134493 ) ) ;
#84099 = CYLINDRICAL_SURFACE ( 'NONE', #49735, 1.249999999999997558 ) ;
#84100 = CARTESIAN_POINT ( 'NONE',  ( 12.66425630052701479, 17.85959152241435177, 11.49999999999998934 ) ) ;
#84101 = CC_DESIGN_PERSON_AND_ORGANIZATION_ASSIGNMENT ( #90196, #99298, ( #44192 ) ) ;
#84102 = CARTESIAN_POINT ( 'NONE',  ( -5.824076695599092801, -5.876774720514411854, 19.72913074730691108 ) ) ;
#84103 = B_SPLINE_CURVE_WITH_KNOTS ( 'NONE', 3,
 ( #52680, #7494, #90741, #100320 ),
 .UNSPECIFIED., .F., .F.,
 ( 4, 4 ),
 ( 0.000000000000000000, 9.999999999998897304E-05 ),
 .UNSPECIFIED. ) ;
#84104 = LINE ( 'NONE', #46552, #15513 ) ;
#84105 = PLANE ( 'NONE',  #40592 ) ;
#84106 = CARTESIAN_POINT ( 'NONE',  ( -78.50135358901988525, -24.51314013834315375, 0.6176544820404143987 ) ) ;
#84107 = FACE_OUTER_BOUND ( 'NONE', #69409, .T. ) ;
#84108 = FACE_OUTER_BOUND ( 'NONE', #43940, .T. ) ;
#84109 = EDGE_LOOP ( 'NONE', ( #44883, #94479, #39820, #50528 ) ) ;
#84110 = CIRCLE ( 'NONE', #87367, 251.4258649670780699 ) ;
#84111 = CARTESIAN_POINT ( 'NONE',  ( 2.691128592823461840, 20.25793168094256202, 11.49999999999998934 ) ) ;
#84112 = VERTEX_POINT ( 'NONE', #22627 ) ;
#84113 = ORIENTED_EDGE ( 'NONE', *, *, #81874, .F. ) ;
#84114 = ORIENTED_EDGE ( 'NONE', *, *, #37676, .F. ) ;
#84115 = ORIENTED_EDGE ( 'NONE', *, *, #73948, .F. ) ;
#84116 = CARTESIAN_POINT ( 'NONE',  ( -8.497478458550677516, -21.44862750780143656, 11.49999999999998934 ) ) ;
#84117 = CARTESIAN_POINT ( 'NONE',  ( 33.74607884027702909, -5.965225279485572685, -4.999864028243830916 ) ) ;
#84118 = CARTESIAN_POINT ( 'NONE',  ( -16.64171244834553676, 11.49637152377623828, -1.500000000000002220 ) ) ;
#84119 = EDGE_LOOP ( 'NONE', ( #70099, #5659, #84727, #1785 ) ) ;
#84120 = CARTESIAN_POINT ( 'NONE',  ( -28.20266704546411773, -25.12201335372101596, 4.938174481708933250 ) ) ;
#84121 = CARTESIAN_POINT ( 'NONE',  ( -37.52287095715006870, -23.47593901973090524, -1.443836447538997314 ) ) ;
#84122 = CARTESIAN_POINT ( 'NONE',  ( -94.22287095715005023, -23.47596703998600631, 11.44779298504227860 ) ) ;
#84123 = CARTESIAN_POINT ( 'NONE',  ( -99.59111425744799817, -24.15620529776628445, 10.23563542870660115 ) ) ;
#84125 = EDGE_LOOP ( 'NONE', ( #36207, #5879, #55368, #5891 ) ) ;
#84124 = CARTESIAN_POINT ( 'NONE',  ( 14.05358622956002357, 16.19628355576825385, 11.49999999999999645 ) ) ;
#84126 = CARTESIAN_POINT ( 'NONE',  ( -128.6228709571500417, -24.50216790748099882, 0.6166512839513794697 ) ) ;
#84127 = CARTESIAN_POINT ( 'NONE',  ( -61.57930063205219540, -24.66019654487199375, 8.947790411086119278 ) ) ;
#84128 = ORIENTED_EDGE ( 'NONE', *, *, #18950, .F. ) ;
#84129 = CARTESIAN_POINT ( 'NONE',  ( -19.40401905104624802, 7.283777608679691262, -1.500000000000002220 ) ) ;
#84132 = ORIENTED_EDGE ( 'NONE', *, *, #81234, .F. ) ;
#84131 = AXIS2_PLACEMENT_3D ( 'NONE', #44008, #36895, #99765 ) ;
#84130 = CYLINDRICAL_SURFACE ( 'NONE', #65318, 15.00000000000000178 ) ;
#84133 = CARTESIAN_POINT ( 'NONE',  ( -65.52287095715006160, -23.48783264082476308, -1.443836473390092578 ) ) ;
#84134 = ORIENTED_EDGE ( 'NONE', *, *, #16248, .F. ) ;
#84135 = CARTESIAN_POINT ( 'NONE',  ( 4.948119756536996761, -6.376774720514410077, 19.52858994054604125 ) ) ;
#84136 = CARTESIAN_POINT ( 'NONE',  ( -35.52287095715006870, -23.47596703998600631, 11.44779298504229281 ) ) ;
#84137 = CARTESIAN_POINT ( 'NONE',  ( -18.27885182143903720, 12.20952002138517045, 11.49999999999999645 ) ) ;
#84138 = CARTESIAN_POINT ( 'NONE',  ( -89.58353286622173073, -24.66019654487199730, 8.947790411086115725 ) ) ;
#84139 = CARTESIAN_POINT ( 'NONE',  ( 9.831018646898828095, -20.30805102056165623, -1.500000000000002220 ) ) ;
#84140 = CARTESIAN_POINT ( 'NONE',  ( -7.180602670292889123, -19.69607742855361465, 11.49999999999998934 ) ) ;
#84141 = DIRECTION ( 'NONE',  ( -3.773278334444166432E-23, 1.000000000000000000, 0.000000000000000000 ) ) ;
#84142 = B_SPLINE_CURVE_WITH_KNOTS ( 'NONE', 3,
 ( #46014, #76933, #62241, #40892, #77433, #7935, #48520, #16041, #38884, #2343, #86063, #24159, #55129, #25157, #56637, #78940, #39888, #16537, #93667 ),
 .UNSPECIFIED., .F., .F.,
 ( 4, 1, 1, 1, 1, 1, 1, 1, 1, 1, 1, 1, 1, 1, 1, 1, 4 ),
 ( 0.000000000000000000, 0.07834298519369982394, 0.1505633028794195749, 0.2161510566599787464, 0.2756797924514269305, 0.3287070503654637710, 0.3759044348322068685, 0.4173018977400307916, 0.4526927480535820614, 0.5172652917530110583, 0.5812165680623054831, 0.6453218939728019299, 0.7120244933797625908, 0.7801300447160447460, 0.8502182262116649847, 0.9226485217347383250, 1.000000000000000000 ),
 .UNSPECIFIED. ) ;
#84143 = CARTESIAN_POINT ( 'NONE',  ( -30.64752034897746924, -23.47593901973090169, -1.443836447538997758 ) ) ;
#84144 = ORIENTED_EDGE ( 'NONE', *, *, #65508, .F. ) ;
#84145 = EDGE_CURVE ( 'NONE', #95252, #62723, #54636, .T. ) ;
#84146 = ORIENTED_EDGE ( 'NONE', *, *, #86313, .T. ) ;
#84147 = ORIENTED_EDGE ( 'NONE', *, *, #70736, .F. ) ;
#84148 = EDGE_CURVE ( 'NONE', #77901, #13356, #84046, .T. ) ;
#84149 = CARTESIAN_POINT ( 'NONE',  ( -66.60300269009690055, -23.73766607897669800, -1.055555164236460897 ) ) ;
#84150 = CARTESIAN_POINT ( 'NONE',  ( 19.30674495121141376, 9.566621930910674365, -1.500000000000002220 ) ) ;
#84151 = CARTESIAN_POINT ( 'NONE',  ( -28.98875734969026041, -5.965225279485572685, 23.37402280011862743 ) ) ;
#84152 = ORIENTED_EDGE ( 'NONE', *, *, #66637, .F. ) ;
#84153 = CARTESIAN_POINT ( 'NONE',  ( -16.61111445048470614, -13.04167290785011701, 11.49999999999998934 ) ) ;
#84154 = CARTESIAN_POINT ( 'NONE',  ( -67.62287095715005592, -23.47593901973091235, -1.443836447539006196 ) ) ;
#84155 = LINE ( 'NONE', #22243, #1122 ) ;
#84156 = CARTESIAN_POINT ( 'NONE',  ( -83.51756172583068860, -23.73791477778911840, 11.05961554403170588 ) ) ;
#84157 = CARTESIAN_POINT ( 'NONE',  ( 9.422519371942208011, -6.475225279485576024, -27.03574706870085720 ) ) ;
#84158 = CARTESIAN_POINT ( 'NONE',  ( -0.8460708837923186509, -5.876774720514410966, 19.21968329462762526 ) ) ;
#84159 = CARTESIAN_POINT ( 'NONE',  ( 9.107982344273736430, -20.20341329189913537, -1.500000000000002220 ) ) ;
#84160 = CARTESIAN_POINT ( 'NONE',  ( -71.60196529453079961, -23.73766607897669800, -1.055555164236456012 ) ) ;
#84161 = EDGE_CURVE ( 'NONE', #55189, #83112, #29763, .T. ) ;
#84162 = ORIENTED_EDGE ( 'NONE', *, *, #67890, .T. ) ;
#84163 = FACE_OUTER_BOUND ( 'NONE', #76389, .T. ) ;
#84164 = DIRECTION ( 'NONE',  ( -0.000000000000000000, 1.000000000000000000, -0.000000000000000000 ) ) ;
#84165 = CARTESIAN_POINT ( 'NONE',  ( -43.52287095715006160, -29.50250243563736774, 8.947779886222148704 ) ) ;
#84166 = AXIS2_PLACEMENT_3D ( 'NONE', #42242, #64079, #57460 ) ;
#84167 = CARTESIAN_POINT ( 'NONE',  ( -97.52287095715010423, -23.95044443724993144, 10.65354141964649415 ) ) ;
#84168 = AXIS2_PLACEMENT_3D ( 'NONE', #27077, #12336, #43306 ) ;
#84169 = CARTESIAN_POINT ( 'NONE',  ( -19.16120753946698585, -3.443109951913609024, -1.500000000000002220 ) ) ;
#84170 = VECTOR ( 'NONE', #28326, 1000.000000000000227 ) ;
#84171 = CARTESIAN_POINT ( 'NONE',  ( -10.59417575825165159, 18.57464501519095279, 11.49999999999998934 ) ) ;
#84172 = DIRECTION ( 'NONE',  ( 0.000000000000000000, -1.000000000000000000, 0.000000000000000000 ) ) ;
#84173 = CARTESIAN_POINT ( 'NONE',  ( -37.52287095715006870, -29.50248528299804818, 1.056150453629031594 ) ) ;
#84174 = CARTESIAN_POINT ( 'NONE',  ( -122.6228709571500417, -24.64965695001469115, 8.947790433994175174 ) ) ;
#84175 = CARTESIAN_POINT ( 'NONE',  ( -100.4326965455115186, -25.18440011175262683, 3.293943117858023406 ) ) ;
#84176 = CARTESIAN_POINT ( 'NONE',  ( 13.52301212282245935, 18.22803923376396540, -1.500000000000002220 ) ) ;
#84177 = VECTOR ( 'NONE', #39345, 1000.000000000000114 ) ;
#84178 = ORIENTED_EDGE ( 'NONE', *, *, #20118, .F. ) ;
#84179 = CARTESIAN_POINT ( 'NONE',  ( -31.62287095715005236, -23.47593901973091235, -1.443836447539013301 ) ) ;
#84180 = CARTESIAN_POINT ( 'NONE',  ( -57.62287095715002039, -24.51387760970723662, 9.387446482453421837 ) ) ;
#84181 = CARTESIAN_POINT ( 'NONE',  ( -15.05033210666397103, 12.90603908704162173, 11.49999999999999645 ) ) ;
#84182 = CARTESIAN_POINT ( 'NONE',  ( -35.52287095715006870, -25.00158670708909270, 2.256160236439166411 ) ) ;
#84183 = ORIENTED_EDGE ( 'NONE', *, *, #5921, .T. ) ;
#84184 = CARTESIAN_POINT ( 'NONE',  ( -5.903826827417286260, -6.376774720514418959, 20.39230070883895252 ) ) ;
#84185 = DIRECTION ( 'NONE',  ( 0.000000000000000000, -2.173523156925980399E-06, 0.9999999999976378895 ) ) ;
#84186 = CARTESIAN_POINT ( 'NONE',  ( -3.891998276399621481, 21.28400606017829233, -1.500000000000002220 ) ) ;
#84187 = CARTESIAN_POINT ( 'NONE',  ( -49.27110903475092130, -25.10935255461681237, 3.423268907010238671 ) ) ;
#84188 = CARTESIAN_POINT ( 'NONE',  ( 16.99290379607386114, -9.356058476803225332, -1.500000000000002220 ) ) ;
#84189 = FACE_OUTER_BOUND ( 'NONE', #7115, .T. ) ;
#84190 = CARTESIAN_POINT ( 'NONE',  ( -35.62287095715007723, -24.83602698348160231, 1.605859176311266845 ) ) ;
#84191 = CARTESIAN_POINT ( 'NONE',  ( 0.4224338394261131779, -19.80333402765648998, -1.500000000000002220 ) ) ;
#84192 = EDGE_CURVE ( 'NONE', #52696, #34410, #90332, .T. ) ;
#84193 = ORIENTED_EDGE ( 'NONE', *, *, #30242, .T. ) ;
#84194 = CARTESIAN_POINT ( 'NONE',  ( -2.359408512905806443, -20.17289352931189583, 11.49999999999999645 ) ) ;
#84195 = CARTESIAN_POINT ( 'NONE',  ( -80.53629819409418644, -25.00158670708910691, 2.256160236439221034 ) ) ;
#84196 = ADVANCED_FACE ( 'NONE', ( #77415 ), #810, .F. ) ;
#84197 = CARTESIAN_POINT ( 'NONE',  ( 33.63243172119919677, -3.340070231344590912, -11.49682753434936622 ) ) ;
#84198 = ORIENTED_EDGE ( 'NONE', *, *, #37188, .T. ) ;
#84199 = B_SPLINE_SURFACE_WITH_KNOTS ( 'NONE', 3, 1, ( 
 ( #47799, #9222 ),
 ( #27468, #3140 ),
 ( #33575, #18348 ),
 ( #4628, #34582 ),
 ( #49821, #96467 ),
 ( #95469, #64553 ),
 ( #25957, #35078 ),
 ( #41704, #26957 ),
 ( #19826, #96969 ),
 ( #4127, #74623 ),
 ( #66050, #58427 ),
 ( #57931, #82236 ),
 ( #34082, #95970 ),
 ( #88362, #49315 ),
 ( #56929, #73145 ),
 ( #43683, #72646 ),
 ( #89856, #12716 ),
 ( #3633, #80753 ),
 ( #89359, #35580 ) ),
 .UNSPECIFIED., .F., .F., .F.,
 ( 4, 1, 1, 1, 1, 1, 1, 1, 1, 1, 1, 1, 1, 1, 1, 1, 4 ),
 ( 2, 2 ),
 ( 0.000000000000000000, 0.07655893299405017172, 0.1491613519791141207, 0.2188268461269970711, 0.2855671390889793493, 0.3503131057192113151, 0.4141251538580798530, 0.4771791613162286727, 0.5403680185081830567, 0.6022023899907512634, 0.6620336537315649750, 0.7199344070495802272, 0.7759074326823265366, 0.8311148643832972915, 0.8866674470119635387, 0.9425523618334878950, 1.000000000000000000 ),
 ( 0.000000000000000000, 1.000000000000000000 ),
 .UNSPECIFIED. ) ;
#84200 = CARTESIAN_POINT ( 'NONE',  ( -102.5550590363431525, -23.96169478059713853, 10.65365249895717881 ) ) ;
#84201 = CARTESIAN_POINT ( 'NONE',  ( -62.55620429048337883, -24.64898659630528144, 1.056161002820822370 ) ) ;
#84202 = CARTESIAN_POINT ( 'NONE',  ( -48.88506298778586512, -25.31602037465095023, 5.954471470684543633 ) ) ;
#84203 = CARTESIAN_POINT ( 'NONE',  ( -40.57795224265260714, -24.83644354573577928, 8.397322867130096569 ) ) ;
#84204 = DIRECTION ( 'NONE',  ( 1.000000000000000000, 3.773278334444167608E-23, 8.201307809403802430E-29 ) ) ;
#84205 = CARTESIAN_POINT ( 'NONE',  ( -10.42242239376218116, -17.14354752861867937, -1.500000000000002220 ) ) ;
#84206 = CARTESIAN_POINT ( 'NONE',  ( 15.97264540888996365, 5.965225279485572685, -27.93485543958161443 ) ) ;
#84207 = ORIENTED_EDGE ( 'NONE', *, *, #59173, .F. ) ;
#84208 = DIRECTION ( 'NONE',  ( 0.000000000000000000, 0.000000000000000000, 1.000000000000000000 ) ) ;
#84209 = CARTESIAN_POINT ( 'NONE',  ( 21.34038654641452482, 8.310931564070170197, 11.49999999999999645 ) ) ;
#84210 = CARTESIAN_POINT ( 'NONE',  ( -20.46125754976198508, 9.905080999540670561, -1.500000000000002220 ) ) ;
#84211 = CARTESIAN_POINT ( 'NONE',  ( -49.53524246831344868, -25.31297094192622055, 4.168640163678797528 ) ) ;
#84212 = CARTESIAN_POINT ( 'NONE',  ( -50.92287095715005307, -23.47596703998600631, 11.44779298504227683 ) ) ;
#84213 = CARTESIAN_POINT ( 'NONE',  ( -59.62287095715002039, -24.33832256526968507, 0.1851278514119832352 ) ) ;
#84214 = CARTESIAN_POINT ( 'NONE',  ( 0.000000000000000000, -5.876774720514426953, -1.399999999999999911 ) ) ;
#84215 = CIRCLE ( 'NONE', #24255, 91.74549126261079834 ) ;
#84216 = EDGE_CURVE ( 'NONE', #58299, #3088, #92622, .T. ) ;
#84217 = ADVANCED_FACE ( 'NONE', ( #99747 ), #16520, .T. ) ;
#84218 = CARTESIAN_POINT ( 'NONE',  ( -118.6228709571501128, -24.35013146730204525, 9.818937971375097717 ) ) ;
#84219 = CARTESIAN_POINT ( 'NONE',  ( 22.81105451610979173, -1.682774720514426114, -18.46691820600746681 ) ) ;
#84220 = EDGE_LOOP ( 'NONE', ( #38158, #73397, #1134, #80316 ) ) ;
#84221 = AXIS2_PLACEMENT_3D ( 'NONE', #39062, #38566, #71912 ) ;
#84222 = CARTESIAN_POINT ( 'NONE',  ( -9.871001836803966256, -17.81128643866572148, 11.49999999999998934 ) ) ;
#84223 = ORIENTED_EDGE ( 'NONE', *, *, #99166, .T. ) ;
#84224 = CARTESIAN_POINT ( 'NONE',  ( 12.10309942457327992, -19.51426552955538085, 11.49999999999998934 ) ) ;
#84225 = DIRECTION ( 'NONE',  ( 1.000000000000000000, 0.000000000000000000, 0.000000000000000000 ) ) ;
#84227 = VERTEX_POINT ( 'NONE', #47490 ) ;
#84226 = EDGE_CURVE ( 'NONE', #5121, #88129, #37877, .T. ) ;
#84228 = CIRCLE ( 'NONE', #85835, 1.836000000000000743 ) ;
#84229 = CARTESIAN_POINT ( 'NONE',  ( -38.62287095715004881, -23.94994826722515668, -0.6494450866351730856 ) ) ;
#84230 = CARTESIAN_POINT ( 'NONE',  ( -77.60588210490597305, -23.48786465467240703, 11.44779295918254647 ) ) ;
#84231 = VECTOR ( 'NONE', #17476, 1000.000000000000000 ) ;
#84232 = CARTESIAN_POINT ( 'NONE',  ( -51.53636606068200621, -24.51419770103156637, 9.386484678747175181 ) ) ;
#84234 = ORIENTED_EDGE ( 'NONE', *, *, #28353, .T. ) ;
#84233 = CARTESIAN_POINT ( 'NONE',  ( 20.00388196354723291, 7.160935007556333609, 11.49999999999999645 ) ) ;
#84235 = VECTOR ( 'NONE', #84827, 1000.000000000000000 ) ;
#84236 = ORIENTED_EDGE ( 'NONE', *, *, #62191, .T. ) ;
#84237 = CARTESIAN_POINT ( 'NONE',  ( 22.20243239366838850, -0.07139729354238147363, 11.49999999999998934 ) ) ;
#84238 = CARTESIAN_POINT ( 'NONE',  ( -4.647353109605855792, 20.10343637636090719, -1.500000000000002220 ) ) ;
#84240 = ORIENTED_EDGE ( 'NONE', *, *, #18647, .T. ) ;
#84239 = VECTOR ( 'NONE', #50482, 1000.000000000000114 ) ;
#84241 = EDGE_LOOP ( 'NONE', ( #31454, #97003, #26623, #48470 ) ) ;
#84242 = CARTESIAN_POINT ( 'NONE',  ( -109.4178292903974352, -25.27682816490595386, 5.278454515681120895 ) ) ;
#84243 = CARTESIAN_POINT ( 'NONE',  ( -39.58139524285506639, -25.16756951564716260, 3.109746001908771262 ) ) ;
#84244 = ORIENTED_EDGE ( 'NONE', *, *, #31572, .F. ) ;
#84245 = CARTESIAN_POINT ( 'NONE',  ( -51.62287095715003460, -24.51387760970725083, 9.387446482453428942 ) ) ;
#84246 = ORIENTED_EDGE ( 'NONE', *, *, #55296, .T. ) ;
#84247 = CARTESIAN_POINT ( 'NONE',  ( -19.38764004357182813, -6.376774720514426953, -21.62823517627351322 ) ) ;
#84248 = EDGE_CURVE ( 'NONE', #91990, #47093, #45008, .T. ) ;
#84249 = CARTESIAN_POINT ( 'NONE',  ( -88.52287095715009002, -24.66019654487200441, 8.947790411086119278 ) ) ;
#84250 = CARTESIAN_POINT ( 'NONE',  ( 18.01467621842780176, -10.50282939286117667, -1.500000000000002220 ) ) ;
#84251 = ADVANCED_FACE ( 'NONE', ( #76418 ), #55671, .T. ) ;
#84252 = CARTESIAN_POINT ( 'NONE',  ( -13.65724274058436194, -16.95215541261048742, 11.49999999999999645 ) ) ;
#84253 = DIRECTION ( 'NONE',  ( -3.773278334453079030E-23, 0.9999999999976377785, 2.173523156925979128E-06 ) ) ;
#84254 = CARTESIAN_POINT ( 'NONE',  ( -78.51706125329930330, -23.73791477778911840, 11.05961554403170588 ) ) ;
#84255 = CARTESIAN_POINT ( 'NONE',  ( 3.503984654965784706, -22.18958196551723816, 11.49999999999998934 ) ) ;
#84256 = LINE ( 'NONE', #75638, #64414 ) ;
#84257 = VERTEX_POINT ( 'NONE', #68330 ) ;
#84258 = CARTESIAN_POINT ( 'NONE',  ( 282.9764569301858046, 4.132774720514426292, 20.79159422840526616 ) ) ;
#84259 = CARTESIAN_POINT ( 'NONE',  ( 5.471383689419965890, -0.3587747205144057872, -29.02273493113404612 ) ) ;
#84260 = B_SPLINE_CURVE_WITH_KNOTS ( 'NONE', 3,
 ( #51816, #38071, #61429, #52312, #44699, #59936 ),
 .UNSPECIFIED., .F., .F.,
 ( 4, 2, 4 ),
 ( 1.570755371633974110E-05, 0.001396183895866088187, 0.002776660238015836880 ),
 .UNSPECIFIED. ) ;
#84261 = VERTEX_POINT ( 'NONE', #62225 ) ;
#84262 = ORIENTED_EDGE ( 'NONE', *, *, #34486, .T. ) ;
#84264 = ADVANCED_FACE ( 'NONE', ( #85036 ), #92647, .F. ) ;
#84263 = CARTESIAN_POINT ( 'NONE',  ( 8.971512145086530055, -9.528487854913503696, 1.946419068999508966E-15 ) ) ;
#84265 = ORIENTED_EDGE ( 'NONE', *, *, #74190, .F. ) ;
#84266 = B_SPLINE_CURVE_WITH_KNOTS ( 'NONE', 3,
 ( #25216, #77987, #63307, #888, #94226, #40458 ),
 .UNSPECIFIED., .F., .F.,
 ( 4, 2, 4 ),
 ( 6.391158118970787649E-06, 0.001387004593080793302, 0.002767618028042615873 ),
 .UNSPECIFIED. ) ;
#84267 = CARTESIAN_POINT ( 'NONE',  ( 7.684279652734260502, -19.92951104315265809, -1.500000000000002220 ) ) ;
#84268 = ADVANCED_FACE ( 'NONE', ( #79929 ), #40377, .F. ) ;
#84269 = VERTEX_POINT ( 'NONE', #47996 ) ;
#84270 = CARTESIAN_POINT ( 'NONE',  ( -0.5131542516139314669, 21.03015271272555253, -1.500000000000002220 ) ) ;
#84271 = CARTESIAN_POINT ( 'NONE',  ( -30.54636096246643007, -24.57768521104549464, 0.8299800598022480935 ) ) ;
#84272 = CARTESIAN_POINT ( 'NONE',  ( -99.52886026165788280, -25.25974063076742127, 3.946325710025691436 ) ) ;
#84273 = CARTESIAN_POINT ( 'NONE',  ( -65.52287095715007581, -24.62285846331437966, 9.038163153548230966 ) ) ;
#84274 = CARTESIAN_POINT ( 'NONE',  ( 21.96865551644221881, -1.217672407684077918, -1.500000000000002220 ) ) ;
#84275 = CARTESIAN_POINT ( 'NONE',  ( -87.62358872278186084, -24.65952944569305316, 1.056160979905705455 ) ) ;
#84276 = ORIENTED_EDGE ( 'NONE', *, *, #9322, .F. ) ;
#84277 = LINE ( 'NONE', #54849, #69688 ) ;
#84278 = EDGE_CURVE ( 'NONE', #70502, #25228, #8919, .T. ) ;
#84279 = ADVANCED_FACE ( 'NONE', ( #57118 ), #10419, .F. ) ;
#84280 = DIRECTION ( 'NONE',  ( -1.000000000000000000, -0.000000000000000000, -0.000000000000000000 ) ) ;
#84281 = CARTESIAN_POINT ( 'NONE',  ( 1.949999999999999956, 0.1924999999999999489, 0.1925000000000000044 ) ) ;
#84282 = DIRECTION ( 'NONE',  ( 0.000000000000000000, -1.000000000000000000, 0.000000000000000000 ) ) ;
#84283 = CARTESIAN_POINT ( 'NONE',  ( -12.14505723179402530, 17.47690347785001919, 11.49999999999998934 ) ) ;
#84284 = CARTESIAN_POINT ( 'NONE',  ( -68.62287095715005592, -29.50250243563736774, 8.947779886222143375 ) ) ;
#84285 = CARTESIAN_POINT ( 'NONE',  ( -107.5502766971892470, -24.51419770103159124, 9.386484678747168076 ) ) ;
#84286 = VECTOR ( 'NONE', #83365, 1000.000000000000000 ) ;
#84287 = CARTESIAN_POINT ( 'NONE',  ( 15.30669619680802995, -3.489325088183165224, -28.51986054853846753 ) ) ;
#84288 = FACE_OUTER_BOUND ( 'NONE', #82741, .T. ) ;
#84289 = CARTESIAN_POINT ( 'NONE',  ( -11.50411854321151672, 19.32100693743031528, -1.500000000000002220 ) ) ;
#84290 = CARTESIAN_POINT ( 'NONE',  ( -109.9100400679505611, -25.06174035403189038, 7.474877196992075312 ) ) ;
#84291 = ORIENTED_EDGE ( 'NONE', *, *, #72017, .F. ) ;
#84292 = CARTESIAN_POINT ( 'NONE',  ( 30.53060340732035982, -6.376774720514426953, 20.86760796525322093 ) ) ;
#84293 = CARTESIAN_POINT ( 'NONE',  ( -0.6043519431218743465, -19.59835197619436187, 11.49999999999999645 ) ) ;
#84294 = CARTESIAN_POINT ( 'NONE',  ( -61.64687923781919920, -25.14083923594766645, 2.947789366383931853 ) ) ;
#84295 = CARTESIAN_POINT ( 'NONE',  ( -41.32836283488544638, -2.682774720514426559, 39.26872235229541985 ) ) ;
#84296 = ORIENTED_EDGE ( 'NONE', *, *, #26293, .T. ) ;
#84297 = CARTESIAN_POINT ( 'NONE',  ( -68.94623785908815705, -25.26418252652374719, 6.008735871699613540 ) ) ;
#84298 = CARTESIAN_POINT ( 'NONE',  ( -125.7765793602851119, -25.31364603714071748, 6.500954295741695255 ) ) ;
#84299 = CARTESIAN_POINT ( 'NONE',  ( -124.6238243596118167, -24.51419770103158768, 9.386484678747164523 ) ) ;
#84300 = CARTESIAN_POINT ( 'NONE',  ( -50.62287095715005592, -23.47593901973091235, -1.443836447539009749 ) ) ;
#84301 = CARTESIAN_POINT ( 'NONE',  ( -2.117704968268854682, 19.61795684621070990, -1.500000000000002220 ) ) ;
#84302 = AXIS2_PLACEMENT_3D ( 'NONE', #77254, #59200, #53951 ) ;
#84303 = ORIENTED_EDGE ( 'NONE', *, *, #67766, .F. ) ;
#84304 = AXIS2_PLACEMENT_3D ( 'NONE', #63793, #25192, #56169 ) ;
#84305 = B_SPLINE_CURVE_WITH_KNOTS ( 'NONE', 3,
 ( #76480, #98320, #44554, #6986 ),
 .UNSPECIFIED., .F., .F.,
 ( 4, 4 ),
 ( 0.001505373688938434684, 0.001772001984008341434 ),
 .UNSPECIFIED. ) ;
#84306 = CARTESIAN_POINT ( 'NONE',  ( 10.68713020350923060, 6.376774720514513106, -28.05292731626249392 ) ) ;
#84307 = DIRECTION ( 'NONE',  ( -0.000000000000000000, 1.000000000000000000, -0.000000000000000000 ) ) ;
#84308 = VECTOR ( 'NONE', #14537, 1000.000000000000227 ) ;
#84309 = ADVANCED_FACE ( 'NONE', ( #63739 ), #15084, .T. ) ;
#84310 = DATE_TIME_ROLE ( 'classification_date' ) ;
#84311 = EDGE_CURVE ( 'NONE', #11314, #9142, #20026, .T. ) ;
#84312 = ORIENTED_EDGE ( 'NONE', *, *, #98537, .T. ) ;
#84313 = DIRECTION ( 'NONE',  ( 1.000000000000000000, -0.000000000000000000, -0.000000000000000000 ) ) ;
#84314 = CARTESIAN_POINT ( 'NONE',  ( -96.62287095715005592, -29.50250786944525672, 11.44777988621623166 ) ) ;
#84315 = CARTESIAN_POINT ( 'NONE',  ( -55.49534339757938284, -24.40034930558990922, 0.3402023900116048494 ) ) ;
#84316 = CARTESIAN_POINT ( 'NONE',  ( -99.48801098274306298, -25.26638478602427540, 7.273530140502286301 ) ) ;
#84317 = CARTESIAN_POINT ( 'NONE',  ( -1.733151984336291695, -5.876774720514408301, 19.29154511076646017 ) ) ;
#84318 = CARTESIAN_POINT ( 'NONE',  ( -109.6228709571500559, -29.50250243563736774, 8.947779886222136270 ) ) ;
#84319 = CARTESIAN_POINT ( 'NONE',  ( -112.5228709571500758, -23.72747288104470087, -1.053458166803225238 ) ) ;
#84320 = CARTESIAN_POINT ( 'NONE',  ( 8.874027960929927517, 17.90919871486395465, 11.49999999999998934 ) ) ;
#84321 = CARTESIAN_POINT ( 'NONE',  ( -125.6228709571500559, -23.85229601348998330, 10.88205029486206499 ) ) ;
#84322 = CARTESIAN_POINT ( 'NONE',  ( -45.56056934063202846, -23.85049219812685095, 10.88485053497527133 ) ) ;
#84323 = ORIENTED_EDGE ( 'NONE', *, *, #24132, .T. ) ;
#84324 = CARTESIAN_POINT ( 'NONE',  ( -66.52287095715009002, -24.51283580621365843, 0.6167428607019661557 ) ) ;
#84325 = CARTESIAN_POINT ( 'NONE',  ( 15.58962545129235799, -6.475225279485573360, -26.91365498785467025 ) ) ;
#84326 = DIRECTION ( 'NONE',  ( -0.7512896232465786639, 0.000000000000000000, -0.6599726524652470561 ) ) ;
#84327 = CARTESIAN_POINT ( 'NONE',  ( -81.63319430079627637, -24.15543982623907482, -0.2315651400026469686 ) ) ;
#84328 = CARTESIAN_POINT ( 'NONE',  ( -28.13975365244298388, -25.26026296467510335, 1.675769660708008590 ) ) ;
#84329 = CARTESIAN_POINT ( 'NONE',  ( -1.955883090540335045, -5.876774720514411854, 19.49432735726521315 ) ) ;
#84330 = EDGE_CURVE ( 'NONE', #70350, #99563, #9920, .T. ) ;
#84331 = DIRECTION ( 'NONE',  ( -1.418030089354338178E-16, 1.000000000000000000, 0.000000000000000000 ) ) ;
#84332 = CARTESIAN_POINT ( 'NONE',  ( -91.52287095715006160, -29.50248528299804818, 1.056150453629040253 ) ) ;
#84333 = VERTEX_POINT ( 'NONE', #2326 ) ;
#84335 = EDGE_CURVE ( 'NONE', #53188, #50179, #4215, .T. ) ;
#84334 = CARTESIAN_POINT ( 'NONE',  ( -9.609455416251792670, -17.83980533922896683, 11.49999999999998934 ) ) ;
#84336 = CARTESIAN_POINT ( 'NONE',  ( -61.52287095715009002, -24.33832256527048798, 0.1851278514138564868 ) ) ;
#84337 = CARTESIAN_POINT ( 'NONE',  ( -49.62287095715005592, -23.48783264082478084, -1.443836473390070596 ) ) ;
#84338 = EDGE_CURVE ( 'NONE', #15988, #53767, #26147, .T. ) ;
#84339 = EDGE_CURVE ( 'NONE', #90885, #61887, #88555, .T. ) ;
#84340 = CARTESIAN_POINT ( 'NONE',  ( -83.58953762381672448, -23.48783264082478794, -1.443836473390065711 ) ) ;
#84341 = EDGE_CURVE ( 'NONE', #77364, #38437, #70829, .T. ) ;
#84342 = ORIENTED_EDGE ( 'NONE', *, *, #47805, .F. ) ;
#84343 = LINE ( 'NONE', #91453, #93934 ) ;
#84344 = CARTESIAN_POINT ( 'NONE',  ( -61.92287095715006728, -23.47596703998600631, 11.44779298504227683 ) ) ;
#84345 = CARTESIAN_POINT ( 'NONE',  ( -3.374260732160392795, -19.82512954709321562, -1.500000000000002220 ) ) ;
#84346 = CARTESIAN_POINT ( 'NONE',  ( -17.90976863334866920, 11.11529090135583075, 11.49999999999999645 ) ) ;
#84347 = ADVANCED_FACE ( 'NONE', ( #73333 ), #91906, .T. ) ;
#84348 = DIRECTION ( 'NONE',  ( -3.773278334453080206E-23, 0.9999999999976377785, 2.173523156925979975E-06 ) ) ;
#84349 = CARTESIAN_POINT ( 'NONE',  ( 10.71795340210964120, -19.33932934982082585, -1.500000000000002220 ) ) ;
#84350 = VECTOR ( 'NONE', #63835, 1000.000000000000000 ) ;
#84351 = CARTESIAN_POINT ( 'NONE',  ( 20.20254288951482735, -3.758238384022974277, 11.49999999999998934 ) ) ;
#84352 = CARTESIAN_POINT ( 'NONE',  ( -96.52287095715001897, -23.94994826722564696, -0.6494450866342700301 ) ) ;
#84353 = CARTESIAN_POINT ( 'NONE',  ( -60.53292719975349456, -24.83618233451449697, 1.606449574219535936 ) ) ;
#84354 = VERTEX_POINT ( 'NONE', #7170 ) ;
#84355 = DIRECTION ( 'NONE',  ( -3.773278334453079618E-23, 0.9999999999976377785, 2.173523156925979975E-06 ) ) ;
#84356 = EDGE_LOOP ( 'NONE', ( #65317, #25645, #74700, #11036 ) ) ;
#84357 = CARTESIAN_POINT ( 'NONE',  ( -5.877732331298974877, -6.376774720514411854, 19.69174559449349005 ) ) ;
#84358 = B_SPLINE_CURVE_WITH_KNOTS ( 'NONE', 3,
 ( #46857, #68199, #53488, #92023, #45860, #14892, #77779, #76778 ),
 .UNSPECIFIED., .F., .F.,
 ( 4, 2, 2, 4 ),
 ( 0.000000000000000000, 0.002001079623178218889, 0.003001619434767332454, 0.004002159246356446452 ),
 .UNSPECIFIED. ) ;
#84359 = CARTESIAN_POINT ( 'NONE',  ( -87.52287095715006160, -24.66019654487200086, 8.947790411086115725 ) ) ;
#84360 = ORIENTED_EDGE ( 'NONE', *, *, #70749, .T. ) ;
#84361 = ORIENTED_EDGE ( 'NONE', *, *, #89457, .F. ) ;
#84362 = B_SPLINE_CURVE_WITH_KNOTS ( 'NONE', 3,
 ( #34196, #73258, #65169, #56544, #872, #8483 ),
 .UNSPECIFIED., .F., .F.,
 ( 4, 2, 4 ),
 ( 0.000000000000000000, 0.001380764517854765182, 0.002761529035709530365 ),
 .UNSPECIFIED. ) ;
#84363 = VERTEX_POINT ( 'NONE', #68087 ) ;
#84364 = CARTESIAN_POINT ( 'NONE',  ( -65.58953762381672448, -23.48783264082478084, -1.443836473390067265 ) ) ;
#84365 = CARTESIAN_POINT ( 'NONE',  ( -49.28933921805457885, -25.11422830839963183, 7.151346021204567194 ) ) ;
#84366 = CARTESIAN_POINT ( 'NONE',  ( 0.09189959430841809773, -6.376774720514410077, 19.67013632031035542 ) ) ;
#84367 = CARTESIAN_POINT ( 'NONE',  ( 14.23986175545555355, -14.96101607593195304, -1.500000000000002220 ) ) ;
#84368 = EDGE_CURVE ( 'NONE', #69591, #47870, #69631, .T. ) ;
#84369 = EDGE_CURVE ( 'NONE', #35109, #69268, #28459, .T. ) ;
#84370 = CARTESIAN_POINT ( 'NONE',  ( -0.6006773669993965559, 21.62980403441659760, 11.49999999999999645 ) ) ;
#84371 = VERTEX_POINT ( 'NONE', #42399 ) ;
#84372 = CARTESIAN_POINT ( 'NONE',  ( -116.4728709571500502, -29.48149383318413896, 5.000941583504024734 ) ) ;
#84373 = DIRECTION ( 'NONE',  ( 0.09721092304694055330, 0.000000000000000000, -0.9952638024365006997 ) ) ;
#84374 = CARTESIAN_POINT ( 'NONE',  ( -19.80502325505778671, 10.42642913751328670, -1.500000000000002220 ) ) ;
#84375 = CARTESIAN_POINT ( 'NONE',  ( -79.60383831484530504, -25.27875002055017717, 6.693228756426554682 ) ) ;
#84376 = CARTESIAN_POINT ( 'NONE',  ( -84.58831393107031715, -24.34968618360934300, 0.1864209137778835568 ) ) ;
#84377 = ORIENTED_EDGE ( 'NONE', *, *, #77029, .T. ) ;
#84378 = CARTESIAN_POINT ( 'NONE',  ( 32.69168087260868560, -4.943943141208723802, -11.74984035242545133 ) ) ;
#84379 = AXIS2_PLACEMENT_3D ( 'NONE', #59605, #4813, #13404 ) ;
#84380 = CARTESIAN_POINT ( 'NONE',  ( -49.63954908479055206, -24.15620529776627379, 10.23563542870661003 ) ) ;
#84381 = CIRCLE ( 'NONE', #66607, 2.040000000000000036 ) ;
#84382 = CARTESIAN_POINT ( 'NONE',  ( -27.70544111104076990, -24.61528742064533049, 1.628749860405701799 ) ) ;
#84383 = CARTESIAN_POINT ( 'NONE',  ( -9.975069251262826953, -18.38325097723136992, 11.49999999999998934 ) ) ;
#84384 = ORIENTED_EDGE ( 'NONE', *, *, #10825, .F. ) ;
#84387 = ORIENTED_EDGE ( 'NONE', *, *, #2471, .F. ) ;
#84386 = EDGE_CURVE ( 'NONE', #73893, #16766, #74482, .T. ) ;
#84385 = CARTESIAN_POINT ( 'NONE',  ( -67.51596021373018175, -23.73791477778911840, 11.05961554403170766 ) ) ;
#84388 = ORIENTED_EDGE ( 'NONE', *, *, #77247, .T. ) ;
#84389 = CARTESIAN_POINT ( 'NONE',  ( -50.62287095715009144, -24.62285846362214059, 9.038163152653526211 ) ) ;
#84390 = CARTESIAN_POINT ( 'NONE',  ( 12.09327641706010326, 17.40255341615222306, -1.500000000000002220 ) ) ;
#84391 = EDGE_CURVE ( 'NONE', #98350, #33363, #79030, .T. ) ;
#84392 = ORIENTED_EDGE ( 'NONE', *, *, #70413, .F. ) ;
#84393 = DIRECTION ( 'NONE',  ( 1.000000000000000000, 0.000000000000000000, 0.000000000000000000 ) ) ;
#84394 = DIRECTION ( 'NONE',  ( -0.000000000000000000, 2.173523156925979552E-06, -0.9999999999976378895 ) ) ;
#84395 = CARTESIAN_POINT ( 'NONE',  ( 18.19902423439809525, 11.99547645517801442, -1.500000000000002220 ) ) ;
#84396 = CARTESIAN_POINT ( 'NONE',  ( -32.52287095715006160, -29.50250243563736774, 8.947779886222150481 ) ) ;
#84397 = CARTESIAN_POINT ( 'NONE',  ( -36.62287095715005592, -23.47593901973091235, -1.443836447539011525 ) ) ;
#84398 = CARTESIAN_POINT ( 'NONE',  ( 7.402957069319889172, -6.376774720514418959, 20.34212842306459024 ) ) ;
#84399 = CARTESIAN_POINT ( 'NONE',  ( -6.661741538832703036, 20.79550341630197607, -1.500000000000002220 ) ) ;
#84400 = CARTESIAN_POINT ( 'NONE',  ( -78.98851047203717712, -25.23623852701372883, 6.393657086652656751 ) ) ;
#84401 = ORIENTED_EDGE ( 'NONE', *, *, #59093, .F. ) ;
#84402 = CARTESIAN_POINT ( 'NONE',  ( -41.62287095715006302, -23.72747288104469732, -1.053458166803227458 ) ) ;
#84403 = CARTESIAN_POINT ( 'NONE',  ( -22.05275734969026047, -0.3587747205144262708, 31.02402280011862246 ) ) ;
#84404 = CARTESIAN_POINT ( 'NONE',  ( 32.68381218857752657, -4.917472161913310380, -3.063707678755676511 ) ) ;
#84406 = EDGE_LOOP ( 'NONE', ( #84901, #58517, #67983, #61682 ) ) ;
#84405 = ADVANCED_FACE ( 'NONE', ( #75675 ), #65737, .T. ) ;
#84407 = EDGE_CURVE ( 'NONE', #7353, #38251, #63533, .T. ) ;
#84408 = ORIENTED_EDGE ( 'NONE', *, *, #98122, .T. ) ;
#84409 = EDGE_CURVE ( 'NONE', #833, #27644, #22381, .T. ) ;
#84410 = ORIENTED_EDGE ( 'NONE', *, *, #38420, .F. ) ;
#84411 = LINE ( 'NONE', #91521, #64352 ) ;
#84412 = CARTESIAN_POINT ( 'NONE',  ( -17.78888362263414535, -11.56919986243916654, -1.500000000000002220 ) ) ;
#84413 = CARTESIAN_POINT ( 'NONE',  ( -94.62789440740766622, -24.34968618360933945, 0.1864209137778861103 ) ) ;
#84414 = CARTESIAN_POINT ( 'NONE',  ( -78.99318656846928377, -25.03138047770763208, 6.404755157858139647 ) ) ;
#84415 = CARTESIAN_POINT ( 'NONE',  ( -28.52287095715005805, -23.32378116302990279, 11.44779301262222049 ) ) ;
#84416 = DIRECTION ( 'NONE',  ( 4.448048651795327725E-16, -1.000000000000000000, 7.118365844322534241E-16 ) ) ;
#84417 = CARTESIAN_POINT ( 'NONE',  ( -19.00951991574052968, 3.723548053296564575, 11.49999999999998934 ) ) ;
#84418 = ADVANCED_FACE ( 'NONE', ( #38119 ), #89055, .F. ) ;
#84419 = CARTESIAN_POINT ( 'NONE',  ( -40.93620634839454908, -25.20650829394578096, 6.812666491500989352 ) ) ;
#84420 = ORIENTED_EDGE ( 'NONE', *, *, #69765, .F. ) ;
#84421 = CARTESIAN_POINT ( 'NONE',  ( 18.80106323769845389, 4.952424739525837616, 11.49999999999999645 ) ) ;
#84422 = CARTESIAN_POINT ( 'NONE',  ( 22.02124265030973760, 6.143225279485574397, 16.20402280011862217 ) ) ;
#84423 = ORIENTED_EDGE ( 'NONE', *, *, #61849, .T. ) ;
#84424 = CARTESIAN_POINT ( 'NONE',  ( 2.936453026386435017, -5.876774720514407413, 18.60215244312560401 ) ) ;
#84425 = FACE_OUTER_BOUND ( 'NONE', #24084, .T. ) ;
#84426 = DIRECTION ( 'NONE',  ( 0.000000000000000000, 0.000000000000000000, -1.000000000000000000 ) ) ;
#84427 = CARTESIAN_POINT ( 'NONE',  ( -93.64042061265114114, -23.48786465467241058, 11.44779295918254469 ) ) ;
#84428 = CARTESIAN_POINT ( 'NONE',  ( -2.340448316220725467, 19.49152957720520618, -1.500000000000002220 ) ) ;
#84429 = CARTESIAN_POINT ( 'NONE',  ( -41.46533095918948675, -25.27805952104409215, 4.218578510459923159 ) ) ;
#84430 = ORIENTED_EDGE ( 'NONE', *, *, #5, .T. ) ;
#84431 = CARTESIAN_POINT ( 'NONE',  ( 17.62533924669398999, -12.40915598911231577, -1.500000000000002220 ) ) ;
#84432 = CARTESIAN_POINT ( 'NONE',  ( -33.52200571196073042, -23.48786465467240347, 11.44779295918255535 ) ) ;
#84433 = LINE ( 'NONE', #4091, #68528 ) ;
#84434 = AXIS2_PLACEMENT_3D ( 'NONE', #42774, #27035, #17420 ) ;
#84435 = CARTESIAN_POINT ( 'NONE',  ( -78.22287095715005023, -23.47593901973090169, -1.443836447538997092 ) ) ;
#84436 = CARTESIAN_POINT ( 'NONE',  ( -22.27228905017084060, 5.866681652885556986, -1.500000000000002220 ) ) ;
#84437 = APPROVAL_ROLE ( '' ) ;
#84438 = CARTESIAN_POINT ( 'NONE',  ( -93.63681820332803341, -23.73766607897670511, -1.055555164236453791 ) ) ;
#84439 = DIRECTION ( 'NONE',  ( -0.000000000000000000, -1.000000000000000000, -0.000000000000000000 ) ) ;
#84440 = CARTESIAN_POINT ( 'NONE',  ( 19.72175082351460063, -4.362005935662174316, 11.49999999999999645 ) ) ;
#84441 = CARTESIAN_POINT ( 'NONE',  ( -126.5562042904833930, -23.48783264082479150, -1.443836473390057273 ) ) ;
#84442 = DIRECTION ( 'NONE',  ( -0.000000000000000000, -1.000000000000000000, -0.000000000000000000 ) ) ;
#84443 = CARTESIAN_POINT ( 'NONE',  ( -110.4629859055347936, -25.29823811875587225, 2.835693564650067611 ) ) ;
#84444 = CARTESIAN_POINT ( 'NONE',  ( -29.49875734969025842, 5.965225279485572685, 25.61802280011862720 ) ) ;
#84445 = PLANE ( 'NONE',  #75390 ) ;
#84446 = CARTESIAN_POINT ( 'NONE',  ( 14.98761344906185577, -13.09354923471379983, 11.49999999999998934 ) ) ;
#84447 = FACE_OUTER_BOUND ( 'NONE', #11035, .T. ) ;
#84448 = CARTESIAN_POINT ( 'NONE',  ( 16.35176858736616978, 11.14859404531058473, -1.500000000000002220 ) ) ;
#84449 = CARTESIAN_POINT ( 'NONE',  ( -56.62787117652145241, -24.51314013834315730, 0.6176544820404098468 ) ) ;
#84450 = VECTOR ( 'NONE', #44395, 1000.000000000000114 ) ;
#84451 = AXIS2_PLACEMENT_3D ( 'NONE', #11063, #18665, #87690 ) ;
#84452 = DIRECTION ( 'NONE',  ( -1.000000000000000000, -3.773278334444167608E-23, -8.201307833595939069E-29 ) ) ;
#84453 = CARTESIAN_POINT ( 'NONE',  ( -1.488488975859286523, -6.376774720514411854, 19.49847411603315095 ) ) ;
#84454 = CARTESIAN_POINT ( 'NONE',  ( -6.358105417860958397, -19.66046682221446318, 11.49999999999999645 ) ) ;
#84455 = FACE_OUTER_BOUND ( 'NONE', #97662, .T. ) ;
#84456 = CARTESIAN_POINT ( 'NONE',  ( -106.6321223050444900, -23.73766607897671577, -1.055555164236449572 ) ) ;
#84457 = CARTESIAN_POINT ( 'NONE',  ( 15.30562342774392093, -16.77826389816909725, 11.49999999999999645 ) ) ;
#84459 = EDGE_CURVE ( 'NONE', #40793, #72161, #99508, .T. ) ;
#84458 = EDGE_LOOP ( 'NONE', ( #92235, #80720, #58460, #78384 ) ) ;
#84460 = CARTESIAN_POINT ( 'NONE',  ( -93.62287095715005592, -24.65952944569304606, 1.056160979905701236 ) ) ;
#84462 = EDGE_CURVE ( 'NONE', #77005, #97841, #49870, .T. ) ;
#84461 = LINE ( 'NONE', #85965, #51666 ) ;
#84463 = EDGE_CURVE ( 'NONE', #68021, #87155, #564, .T. ) ;
#84464 = CARTESIAN_POINT ( 'NONE',  ( -5.623992922573770592, 19.38241096367466199, 11.49999999999998934 ) ) ;
#84465 = B_SPLINE_CURVE_WITH_KNOTS ( 'NONE', 3,
 ( #65031, #2612, #95944, #57410 ),
 .UNSPECIFIED., .F., .F.,
 ( 4, 4 ),
 ( 0.000000000000000000, 0.0009166666666666628549 ),
 .UNSPECIFIED. ) ;
#84466 = CARTESIAN_POINT ( 'NONE',  ( 9.071512145086501278, -0.9000000000000000222, -3.687490859131162591 ) ) ;
#84467 = EDGE_CURVE ( 'NONE', #21835, #66467, #1886, .T. ) ;
#84468 = CARTESIAN_POINT ( 'NONE',  ( -95.62287095715007013, -23.84047902841601996, -0.8780736468305821996 ) ) ;
#84469 = ADVANCED_FACE ( 'NONE', ( #47249 ), #71090, .T. ) ;
#84470 = VERTEX_POINT ( 'NONE', #31011 ) ;
#84471 = EDGE_CURVE ( 'NONE', #16750, #48546, #7794, .T. ) ;
#84472 = ORIENTED_EDGE ( 'NONE', *, *, #22011, .T. ) ;
#84473 = CARTESIAN_POINT ( 'NONE',  ( 0.3791100739519297491, -5.876774720514418071, 20.35309744218306349 ) ) ;
#84474 = CARTESIAN_POINT ( 'NONE',  ( -16.32851894532483783, 16.03542138455653898, 11.49999999999998934 ) ) ;
#84475 = CARTESIAN_POINT ( 'NONE',  ( -102.6228709571500559, -29.50250243563736774, 8.947779886222138046 ) ) ;
#84476 = CARTESIAN_POINT ( 'NONE',  ( -2.787017431591729988, -21.48445716988565835, -1.500000000000002220 ) ) ;
#84477 = LINE ( 'NONE', #15457, #43135 ) ;
#84478 = CARTESIAN_POINT ( 'NONE',  ( -34.64978355792892017, -23.96119346886880663, -0.6495511937831990323 ) ) ;
#84479 = CARTESIAN_POINT ( 'NONE',  ( -7.158894406585330827, 19.61798520005962487, 11.49999999999999645 ) ) ;
#84480 = EDGE_LOOP ( 'NONE', ( #9, #35456, #90604, #61881 ) ) ;
#84481 = ADVANCED_FACE ( 'NONE', ( #92904 ), #86303, .T. ) ;
#84482 = FACE_OUTER_BOUND ( 'NONE', #62320, .T. ) ;
#84483 = CARTESIAN_POINT ( 'NONE',  ( -14.32918165687622825, -16.72005635474405949, -1.500000000000002220 ) ) ;
#84484 = CARTESIAN_POINT ( 'NONE',  ( -105.5468779439268587, -24.92592662359561473, 8.075495903018000021 ) ) ;
#84485 = CARTESIAN_POINT ( 'NONE',  ( -40.50110916354886825, -25.10925768751217291, 2.834725980302106763 ) ) ;
#84486 = EDGE_LOOP ( 'NONE', ( #56533, #27482, #9273, #91361 ) ) ;
#84487 = CARTESIAN_POINT ( 'NONE',  ( 4.931982383686722926, -6.376774720514411854, 19.38944687450761961 ) ) ;
#84488 = CARTESIAN_POINT ( 'NONE',  ( -90.59505941600714607, -24.15602025860896873, 10.28564288303535434 ) ) ;
#84489 = VERTEX_POINT ( 'NONE', #77172 ) ;
#84490 = CARTESIAN_POINT ( 'NONE',  ( -93.22287095715005023, -23.47596703998600631, 11.44779298504227860 ) ) ;
#84491 = ORIENTED_EDGE ( 'NONE', *, *, #31789, .T. ) ;
#84492 = VERTEX_POINT ( 'NONE', #23381 ) ;
#84493 = CARTESIAN_POINT ( 'NONE',  ( -71.54133414514889466, -24.51419770103159124, 9.386484678747166299 ) ) ;
#84494 = CARTESIAN_POINT ( 'NONE',  ( -101.7776484685884242, -25.10936053256603273, 3.986250973267613240 ) ) ;
#84495 = CARTESIAN_POINT ( 'NONE',  ( -4.243469080022288509, -6.376774720514411854, 19.94806476610987644 ) ) ;
#84496 = CARTESIAN_POINT ( 'NONE',  ( -18.53176153473302179, -8.692061069824589481, -1.500000000000002220 ) ) ;
#84497 = ADVANCED_FACE ( 'NONE', ( #84796 ), #40137, .T. ) ;
#84498 = ORIENTED_EDGE ( 'NONE', *, *, #25363, .F. ) ;
#84499 = CARTESIAN_POINT ( 'NONE',  ( -2.711489738547795625, -6.376774720514410077, 19.27798293355755632 ) ) ;
#84500 = CARTESIAN_POINT ( 'NONE',  ( -44.51366543650918572, -23.73766607897669800, -1.055555164236459120 ) ) ;
#84501 = CARTESIAN_POINT ( 'NONE',  ( 22.74089357256066890, 1.477225279485574028, -19.20396252371061863 ) ) ;
#84502 = CARTESIAN_POINT ( 'NONE',  ( 1.165341552704713513, 22.26021350444069213, 11.49999999999998934 ) ) ;
#84503 = CARTESIAN_POINT ( 'NONE',  ( -80.64675904551151575, -25.20074414427590881, 3.409327697718777195 ) ) ;
#84504 = CARTESIAN_POINT ( 'NONE',  ( 7.089543269230769162, -5.876774720514413630, 19.75741185897435415 ) ) ;
#84505 = EDGE_CURVE ( 'NONE', #30477, #46180, #100008, .T. ) ;
#84506 = ORIENTED_EDGE ( 'NONE', *, *, #66142, .F. ) ;
#84507 = DIRECTION ( 'NONE',  ( -3.773278334453079030E-23, 0.9999999999976377785, 2.173523156925979128E-06 ) ) ;
#84508 = CARTESIAN_POINT ( 'NONE',  ( -29.66400988275576367, -25.26247693264633654, 6.487135408686464544 ) ) ;
#84509 = CARTESIAN_POINT ( 'NONE',  ( 5.313885144808909722, 20.14914662543312929, 11.49999999999998934 ) ) ;
#84510 = ORIENTED_EDGE ( 'NONE', *, *, #18771, .T. ) ;
#84512 = EDGE_LOOP ( 'NONE', ( #51644, #537, #73778, #81899 ) ) ;
#84511 = CARTESIAN_POINT ( 'NONE',  ( 4.653733606810938284, -6.376774720514411854, 19.95301661664751336 ) ) ;
#84513 = CARTESIAN_POINT ( 'NONE',  ( -51.21833214457227257, -25.25854513373207055, 6.843755114720857513 ) ) ;
#84514 = VERTEX_POINT ( 'NONE', #46749 ) ;
#84515 = VERTEX_POINT ( 'NONE', #24898 ) ;
#84516 = PLANE ( 'NONE',  #88416 ) ;
#84517 = CARTESIAN_POINT ( 'NONE',  ( -55.62287095715007013, -23.84081130438200091, 10.88220057463249191 ) ) ;
#84518 = CARTESIAN_POINT ( 'NONE',  ( -110.2093792378192063, -25.30161501422653814, 5.585409209247975681 ) ) ;
#84519 = CARTESIAN_POINT ( 'NONE',  ( 22.02124265030973760, -6.376774720514428729, 19.20402280011862217 ) ) ;
#84520 = CARTESIAN_POINT ( 'NONE',  ( -110.5228709571500332, -24.14321612903118464, -0.2833117244520817479 ) ) ;
#84521 = CARTESIAN_POINT ( 'NONE',  ( -0.7395115731254252589, 18.09566585216508727, -9.000000000000000000 ) ) ;
#84523 = VERTEX_POINT ( 'NONE', #8183 ) ;
#84522 = CARTESIAN_POINT ( 'NONE',  ( 10.50125231818214289, 19.49540335892314502, 11.49999999999999645 ) ) ;
#84524 = CARTESIAN_POINT ( 'NONE',  ( -78.62287095715005592, -24.64965695001468404, 8.947790433994182280 ) ) ;
#84525 = CARTESIAN_POINT ( 'NONE',  ( -14.08738070862771963, 17.71811851510361535, 11.49999999999998934 ) ) ;
#84526 = EDGE_CURVE ( 'NONE', #20835, #65831, #1582, .T. ) ;
#84528 = ORIENTED_EDGE ( 'NONE', *, *, #96407, .T. ) ;
#84527 = CARTESIAN_POINT ( 'NONE',  ( -92.52287095715009002, -23.73907113217727272, -1.053371485780262296 ) ) ;
#84529 = AXIS2_PLACEMENT_3D ( 'NONE', #24797, #40033, #64403 ) ;
#84530 = EDGE_LOOP ( 'NONE', ( #56927, #36369, #90417, #86138 ) ) ;
#84531 = CC_DESIGN_APPROVAL ( #47005, ( #47237 ) ) ;
#84532 = DIRECTION ( 'NONE',  ( -3.773278334453079030E-23, 0.9999999999976377785, 2.173523156925979128E-06 ) ) ;
#84533 = EDGE_CURVE ( 'NONE', #67210, #58474, #32015, .T. ) ;
#84534 = CARTESIAN_POINT ( 'NONE',  ( -7.184633862932894743, 18.80532529184710100, 11.49999999999998934 ) ) ;
#84535 = DIRECTION ( 'NONE',  ( -0.7071067811865513475, 0.7071067811865437980, 0.000000000000000000 ) ) ;
#84536 = ORIENTED_EDGE ( 'NONE', *, *, #39641, .T. ) ;
#84537 = CARTESIAN_POINT ( 'NONE',  ( -39.55620429048340014, -23.48786465467240347, 11.44779295918255180 ) ) ;
#84538 = CARTESIAN_POINT ( 'NONE',  ( 22.34790896907852442, -0.4833156648990815651, -1.500000000000002220 ) ) ;
#84539 = VERTEX_POINT ( 'NONE', #62989 ) ;
#84540 = ORIENTED_EDGE ( 'NONE', *, *, #80491, .F. ) ;
#84541 = CARTESIAN_POINT ( 'NONE',  ( -35.22287095715007155, -23.47593901973090169, -1.443836447538997980 ) ) ;
#84542 = CARTESIAN_POINT ( 'NONE',  ( -82.62287095715005592, -29.50250786944525672, 11.44777988621623521 ) ) ;
#84543 = CARTESIAN_POINT ( 'NONE',  ( -32.30247028140506416, 1.684774720514426560, 27.60502002861223048 ) ) ;
#84544 = CARTESIAN_POINT ( 'NONE',  ( -68.52287095715006160, -23.48786465467241058, 11.44779295918254647 ) ) ;
#84545 = B_SPLINE_CURVE_WITH_KNOTS ( 'NONE', 3,
 ( #57146, #3362, #66761, #66263 ),
 .UNSPECIFIED., .F., .F.,
 ( 4, 4 ),
 ( 0.3407433164617006960, 0.3497497477338162297 ),
 .UNSPECIFIED. ) ;
#84546 = CARTESIAN_POINT ( 'NONE',  ( -40.62287095715004170, -29.50248789122583659, 2.256150453626215580 ) ) ;
#84547 = CARTESIAN_POINT ( 'NONE',  ( 15.26536572251939461, -12.21375333317339695, 11.49999999999998934 ) ) ;
#84548 = LINE ( 'NONE', #9422, #47407 ) ;
#84549 = CARTESIAN_POINT ( 'NONE',  ( -8.581294335678165908, -19.67629172487136557, 11.49999999999998934 ) ) ;
#84550 = PLANE ( 'NONE',  #94979 ) ;
#84551 = DIRECTION ( 'NONE',  ( -3.773278334453079618E-23, 0.9999999999976377785, 2.173523156925978705E-06 ) ) ;
#84552 = DIRECTION ( 'NONE',  ( -0.6599726524652352877, 0.000000000000000000, 0.7512896232465892110 ) ) ;
#84553 = CARTESIAN_POINT ( 'NONE',  ( -9.150087108448493822, 20.98025145036519845, -1.500000000000002220 ) ) ;
#84554 = CIRCLE ( 'NONE', #22964, 1.050000000000000488 ) ;
#84555 = B_SPLINE_CURVE_WITH_KNOTS ( 'NONE', 3,
 ( #34923, #58757, #64404, #65404, #95322, #3981 ),
 .UNSPECIFIED., .F., .F.,
 ( 4, 2, 4 ),
 ( 3.102663313537988147E-09, 0.002226959955260804196, 0.004453916807858295489 ),
 .UNSPECIFIED. ) ;
#84556 = PERSON_AND_ORGANIZATION ( #70597, #27821 ) ;
#84557 = CARTESIAN_POINT ( 'NONE',  ( -96.55485876771541598, -23.96169478059713498, 10.65365249895717881 ) ) ;
#84558 = LINE ( 'NONE', #22642, #62059 ) ;
#84559 = CARTESIAN_POINT ( 'NONE',  ( -19.95465934538571062, -0.7993260556091378310, 11.49999999999999645 ) ) ;
#84560 = PLANE ( 'NONE',  #34875 ) ;
#84561 = CARTESIAN_POINT ( 'NONE',  ( -124.6228709571500559, -23.48783264082479505, -1.443836473390058828 ) ) ;
#84562 = CARTESIAN_POINT ( 'NONE',  ( 4.468667172983064262, -5.876774720514401196, 18.40700896291420463 ) ) ;
#84563 = DIRECTION ( 'NONE',  ( -0.000000000000000000, -1.000000000000000000, -0.000000000000000000 ) ) ;
#84564 = ORIENTED_EDGE ( 'NONE', *, *, #83022, .F. ) ;
#84565 = CARTESIAN_POINT ( 'NONE',  ( -109.5228709571500616, -24.64898659630530275, 1.056161002820831474 ) ) ;
#84566 = CARTESIAN_POINT ( 'NONE',  ( -59.52287095715006160, -29.50250786944525672, 11.44777988621623876 ) ) ;
#84567 = CARTESIAN_POINT ( 'NONE',  ( -21.62197530259306788, 2.132803791230205359, 11.49999999999998934 ) ) ;
#84568 = DIRECTION ( 'NONE',  ( -3.773278334453080206E-23, 0.9999999999976377785, 2.173523156925979975E-06 ) ) ;
#84569 = CARTESIAN_POINT ( 'NONE',  ( -19.52990877098713796, 1.257015143768854815, -1.500000000000002220 ) ) ;
#84570 = FACE_OUTER_BOUND ( 'NONE', #44059, .T. ) ;
#84571 = CARTESIAN_POINT ( 'NONE',  ( -40.52112337587701063, -25.18518878011527207, 3.295773480853921189 ) ) ;
#84572 = PERSON_AND_ORGANIZATION ( #44001, #81497 ) ;
#84573 = CARTESIAN_POINT ( 'NONE',  ( -91.56188894598993500, -23.48786465467241413, 11.44779295918254469 ) ) ;
#84574 = CARTESIAN_POINT ( 'NONE',  ( 3.181132013147180970, -6.376774720514426065, 21.64201922499777808 ) ) ;
#84575 = CARTESIAN_POINT ( 'NONE',  ( -14.38416181709762043, 14.64695106392160895, 11.49999999999999645 ) ) ;
#84576 = CARTESIAN_POINT ( 'NONE',  ( -94.52287095715001897, -24.33832256527048088, 0.1851278514138636755 ) ) ;
#84577 = AXIS2_PLACEMENT_3D ( 'NONE', #63012, #93427, #8712 ) ;
#84578 = LINE ( 'NONE', #90202, #38355 ) ;
#84579 = EDGE_CURVE ( 'NONE', #43445, #8718, #40530, .T. ) ;
#84580 = ORIENTED_EDGE ( 'NONE', *, *, #58858, .T. ) ;
#84581 =( LENGTH_UNIT ( ) NAMED_UNIT ( * ) SI_UNIT ( .MILLI., .METRE. ) );
#84582 = CARTESIAN_POINT ( 'NONE',  ( -109.3914004513356701, -25.29449945578133452, 4.479052194644536300 ) ) ;
#84583 = DIRECTION ( 'NONE',  ( -7.960204194457801640E-17, -1.000000000000000000, 0.000000000000000000 ) ) ;
#84585 = ADVANCED_FACE ( 'NONE', ( #41146 ), #27412, .T. ) ;
#84584 = CARTESIAN_POINT ( 'NONE',  ( -125.5541636680248274, -24.92592662359561828, 8.075495903018000021 ) ) ;
#84586 = DIRECTION ( 'NONE',  ( 2.352173255807804438E-16, -2.352173255807796056E-16, -1.000000000000000000 ) ) ;
#84587 = PLANE ( 'NONE',  #85642 ) ;
#84588 = EDGE_CURVE ( 'NONE', #73442, #48696, #35027, .T. ) ;
#84589 = CARTESIAN_POINT ( 'NONE',  ( -124.6228709571500701, -23.73934037231757799, 11.05740245334328087 ) ) ;
#84590 = EDGE_CURVE ( 'NONE', #94756, #70772, #49269, .T. ) ;
#84591 = VECTOR ( 'NONE', #62259, 1000.000000000000114 ) ;
#84592 = CARTESIAN_POINT ( 'NONE',  ( 17.08057647167376913, 15.47633299359885761, 11.49999999999999645 ) ) ;
#84593 = CARTESIAN_POINT ( 'NONE',  ( -15.22011711465338912, -17.00649957279452451, 11.49999999999998934 ) ) ;
#84594 = CARTESIAN_POINT ( 'NONE',  ( -104.5228709571500758, -24.64898659630529565, 1.056161002820829697 ) ) ;
#84595 = ADVANCED_FACE ( 'NONE', ( #17800 ), #42156, .F. ) ;
#84596 = CARTESIAN_POINT ( 'NONE',  ( -67.52287095715006160, -24.65952944569304961, 1.056160979905697239 ) ) ;
#84597 = CARTESIAN_POINT ( 'NONE',  ( -58.87764846858842560, -25.13069340115296058, 2.947789388436138580 ) ) ;
#84598 = LOCAL_TIME ( 0, 54, 15.00000000000000000, #97671 ) ;
#84599 = CARTESIAN_POINT ( 'NONE',  ( 21.16571772479873204, -7.350578744355993344, 11.49999999999999645 ) ) ;
#84600 = FACE_OUTER_BOUND ( 'NONE', #58086, .T. ) ;
#84601 = EDGE_CURVE ( 'NONE', #50993, #55725, #53816, .T. ) ;
#84602 = B_SPLINE_CURVE_WITH_KNOTS ( 'NONE', 3,
 ( #73801, #35251, #27639, #92013 ),
 .UNSPECIFIED., .F., .F.,
 ( 4, 4 ),
 ( 0.4601144809659691859, 0.4691209122380847751 ),
 .UNSPECIFIED. ) ;
#84603 = CARTESIAN_POINT ( 'NONE',  ( -34.62287095715007013, -23.47596703998600276, 11.44779298504227505 ) ) ;
#84604 = CARTESIAN_POINT ( 'NONE',  ( -8.017166757594178961, 20.41873492177044724, 11.49999999999998934 ) ) ;
#84605 = CARTESIAN_POINT ( 'NONE',  ( -5.205649524681222218, -6.376774720514408301, 19.16400979764067714 ) ) ;
#84606 = CARTESIAN_POINT ( 'NONE',  ( -11.16000000000000014, -9.652339641703484574, -1.621096496867199033 ) ) ;
#84607 = DIRECTION ( 'NONE',  ( 0.000000000000000000, -1.000000000000000000, 0.000000000000000000 ) ) ;
#84608 = LINE ( 'NONE', #37935, #92953 ) ;
#84609 = PLANE ( 'NONE',  #27416 ) ;
#84610 = ORIENTED_EDGE ( 'NONE', *, *, #19402, .F. ) ;
#84611 = CARTESIAN_POINT ( 'NONE',  ( -17.80769721941407369, -10.09151516499986734, -1.500000000000002220 ) ) ;
#84612 = ORIENTED_EDGE ( 'NONE', *, *, #71459, .T. ) ;
#84613 = ORIENTED_EDGE ( 'NONE', *, *, #52862, .T. ) ;
#84614 = EDGE_LOOP ( 'NONE', ( #70957, #7365, #21947, #98544 ) ) ;
#84615 = ORIENTED_EDGE ( 'NONE', *, *, #78059, .F. ) ;
#84616 = CARTESIAN_POINT ( 'NONE',  ( -20.21456430084473155, -11.12997698910670152, 11.49999999999998934 ) ) ;
#84617 = FACE_OUTER_BOUND ( 'NONE', #51058, .T. ) ;
#84618 = CARTESIAN_POINT ( 'NONE',  ( 20.23688964843749005, 1.552196809742036221, -1.500000000000002220 ) ) ;
#84619 = EDGE_LOOP ( 'NONE', ( #2118, #82546, #10635, #49413 ) ) ;
#84620 = CARTESIAN_POINT ( 'NONE',  ( -28.21574693287574931, -24.80510216826755610, 2.243760839632586102 ) ) ;
#84621 = CARTESIAN_POINT ( 'NONE',  ( -46.58953762381672448, -24.64898659630528499, 1.056161002820820372 ) ) ;
#84622 = CARTESIAN_POINT ( 'NONE',  ( -126.6228709571500559, -29.50250243563736774, 8.947779886222132717 ) ) ;
#84623 = CARTESIAN_POINT ( 'NONE',  ( -70.58659607870677632, -24.63355581998385091, 0.9682620441943861067 ) ) ;
#84625 = ORIENTED_EDGE ( 'NONE', *, *, #90093, .T. ) ;
#84624 = CARTESIAN_POINT ( 'NONE',  ( 10.55508701655855575, -18.62573008410804221, 11.49999999999999645 ) ) ;
#84626 = LINE ( 'NONE', #44075, #74398 ) ;
#84627 = CARTESIAN_POINT ( 'NONE',  ( -61.59281505598787021, -24.15620529776628089, 10.23563542870660825 ) ) ;
#84628 = ORIENTED_EDGE ( 'NONE', *, *, #15046, .F. ) ;
#84629 = CARTESIAN_POINT ( 'NONE',  ( -10.81534556030752725, -17.66751395530895152, -1.500000000000002220 ) ) ;
#84630 = ORIENTED_EDGE ( 'NONE', *, *, #95387, .F. ) ;
#84632 = ORIENTED_EDGE ( 'NONE', *, *, #6844, .F. ) ;
#84631 = PLANE ( 'NONE',  #91200 ) ;
#84633 = VECTOR ( 'NONE', #3938, 1000.000000000000000 ) ;
#84634 = B_SPLINE_SURFACE_WITH_KNOTS ( 'NONE', 3, 3, ( 
 ( #33170, #64151, #95075, #25560 ),
 ( #87461, #13815, #82832, #91947 ),
 ( #4728, #74718, #22417, #67142 ),
 ( #84327, #14313, #12818, #5716 ),
 ( #28548, #13315, #44294, #75711 ),
 ( #20427, #59023, #30038, #97567 ),
 ( #21422, #53403, #83836, #5220 ) ),
 .UNSPECIFIED., .F., .F., .F.,
 ( 4, 3, 4 ),
 ( 4, 4 ),
 ( 0.0004766839783841440902, 0.1029713700210908162, 0.2054660560637974753 ),
 ( 0.4896185478418259018, 0.4908571814961936175 ),
 .UNSPECIFIED. ) ;
#84635 = CARTESIAN_POINT ( 'NONE',  ( -28.54454667017215641, -23.99501971000362843, -0.2315644524145782090 ) ) ;
#84636 = VERTEX_POINT ( 'NONE', #80695 ) ;
#84637 = ORIENTED_EDGE ( 'NONE', *, *, #74300, .F. ) ;
#84638 = CARTESIAN_POINT ( 'NONE',  ( 3.825381322105384285, -6.376774720514401196, 18.16071977647550995 ) ) ;
#84639 = CARTESIAN_POINT ( 'NONE',  ( -65.51286458321119710, -23.85016227208580730, -0.8807180028928343063 ) ) ;
#84640 = CARTESIAN_POINT ( 'NONE',  ( 8.537626919312410578, 20.26776412955123163, 11.49999999999999645 ) ) ;
#84641 = CARTESIAN_POINT ( 'NONE',  ( -89.56219111058589988, -23.48786465467241413, 11.44779295918254292 ) ) ;
#84642 = CARTESIAN_POINT ( 'NONE',  ( 3.584315319034878211, 22.25550262085195286, -1.500000000000002220 ) ) ;
#84643 = B_SPLINE_CURVE_WITH_KNOTS ( 'NONE', 3,
 ( #27829, #74498, #3507, #34945, #96839, #50178 ),
 .UNSPECIFIED., .F., .F.,
 ( 4, 2, 4 ),
 ( 0.000000000000000000, 0.001380901958385392448, 0.002761803916770784895 ),
 .UNSPECIFIED. ) ;
#84644 = CARTESIAN_POINT ( 'NONE',  ( -18.08314111433443827, -10.61732331186343004, 11.49999999999998934 ) ) ;
#84645 = CARTESIAN_POINT ( 'NONE',  ( -111.6228709571500559, -24.64898659630368627, 1.056161002820831474 ) ) ;
#84646 = DIRECTION ( 'NONE',  ( 0.000000000000000000, -1.000000000000000000, 0.000000000000000000 ) ) ;
#84647 = ORIENTED_EDGE ( 'NONE', *, *, #43205, .F. ) ;
#84648 = AXIS2_PLACEMENT_3D ( 'NONE', #65269, #80459, #81469 ) ;
#84649 = VERTEX_POINT ( 'NONE', #73094 ) ;
#84650 = ORIENTED_EDGE ( 'NONE', *, *, #32369, .F. ) ;
#84651 = CARTESIAN_POINT ( 'NONE',  ( -36.62287095715005592, -23.48783264082477729, -1.443836473390072372 ) ) ;
#84652 = ADVANCED_FACE ( 'NONE', ( #88313 ), #3089, .T. ) ;
#84653 = CARTESIAN_POINT ( 'NONE',  ( -19.98823316618875268, 7.996883007359760320, -1.500000000000002220 ) ) ;
#84654 = EDGE_CURVE ( 'NONE', #63531, #19596, #71981, .T. ) ;
#84655 = DIRECTION ( 'NONE',  ( 0.000000000000000000, 0.000000000000000000, 1.000000000000000000 ) ) ;
#84656 = ORIENTED_EDGE ( 'NONE', *, *, #66279, .T. ) ;
#84657 = CARTESIAN_POINT ( 'NONE',  ( -21.11812214938331422, 0.5215410354952813021, -1.500000000000002220 ) ) ;
#84658 = CARTESIAN_POINT ( 'NONE',  ( -67.55620429048337883, -23.47593901973091235, -1.443836447539006196 ) ) ;
#84659 = CARTESIAN_POINT ( 'NONE',  ( -130.5728709571500588, -23.47593901973090524, -1.443836447538995982 ) ) ;
#84660 = CARTESIAN_POINT ( 'NONE',  ( -83.64500779952560094, -23.48786465467241413, 11.44779295918254469 ) ) ;
#84661 = CARTESIAN_POINT ( 'NONE',  ( -32.52287095715006160, -29.50247984919015209, -1.443849546365062242 ) ) ;
#84662 = CARTESIAN_POINT ( 'NONE',  ( -99.80419109892318374, -25.13411624585489434, 2.967105462742589239 ) ) ;
#84663 = CARTESIAN_POINT ( 'NONE',  ( 4.116201370682176730, 21.75534844777131838, -1.500000000000002220 ) ) ;
#84664 = CARTESIAN_POINT ( 'NONE',  ( -71.59237387687302601, -24.15543982623907127, -0.2315651400026636497 ) ) ;
#84665 = EDGE_LOOP ( 'NONE', ( #29415, #98831, #50556, #57942 ) ) ;
#84666 = DIRECTION ( 'NONE',  ( 1.000000000000000000, -7.960204194457801640E-17, 0.000000000000000000 ) ) ;
#84667 = LINE ( 'NONE', #100368, #65418 ) ;
#84668 = CARTESIAN_POINT ( 'NONE',  ( 13.91401389203221406, 0.3587747205144265483, 158.0376437107427137 ) ) ;
#84669 = CARTESIAN_POINT ( 'NONE',  ( 0.000000000000000000, -6.943225279485572443, 0.000000000000000000 ) ) ;
#84670 = AXIS2_PLACEMENT_3D ( 'NONE', #91654, #60235, #84048 ) ;
#84671 = CARTESIAN_POINT ( 'NONE',  ( 16.20606029192996900, -10.75321813762353251, 11.49999999999998934 ) ) ;
#84672 = PLANE ( 'NONE',  #67398 ) ;
#84673 = CARTESIAN_POINT ( 'NONE',  ( -18.60337119584764665, 10.53494341765418874, -1.500000000000002220 ) ) ;
#84674 = CARTESIAN_POINT ( 'NONE',  ( -62.61044358207880123, -23.48783264082476308, -1.443836473390090580 ) ) ;
#84675 = CARTESIAN_POINT ( 'NONE',  ( -106.5562042904834072, -23.48783264082478794, -1.443836473390061492 ) ) ;
#84676 = CARTESIAN_POINT ( 'NONE',  ( -122.5228709571500616, -24.64965694238408034, 8.947790433994191162 ) ) ;
#84677 = DIRECTION ( 'NONE',  ( 3.773278334444166432E-23, -1.000000000000000000, 0.000000000000000000 ) ) ;
#84678 = CARTESIAN_POINT ( 'NONE',  ( 22.16846167567618053, -4.910139430472912458, -1.500000000000002220 ) ) ;
#84679 = AXIS2_PLACEMENT_3D ( 'NONE', #73345, #87561, #49012 ) ;
#84680 = CARTESIAN_POINT ( 'NONE',  ( -99.22287095715006444, -23.47596703998600276, 11.44779298504227860 ) ) ;
#84681 = CARTESIAN_POINT ( 'NONE',  ( -127.6228709571500559, -24.65952944569305316, 1.056160979905707897 ) ) ;
#84682 = CARTESIAN_POINT ( 'NONE',  ( -14.51517298184297289, -13.48802281452852725, 11.49999999999999645 ) ) ;
#84683 = VECTOR ( 'NONE', #87154, 999.9999999999998863 ) ;
#84684 = DIRECTION ( 'NONE',  ( 1.000000000000000000, 0.000000000000000000, 0.000000000000000000 ) ) ;
#84685 = VERTEX_POINT ( 'NONE', #79688 ) ;
#84686 = B_SPLINE_CURVE_WITH_KNOTS ( 'NONE', 3,
 ( #24886, #17281, #15772, #55864 ),
 .UNSPECIFIED., .F., .F.,
 ( 4, 4 ),
 ( 0.01050750315080129817, 0.01951393442291685446 ),
 .UNSPECIFIED. ) ;
#84687 = CARTESIAN_POINT ( 'NONE',  ( 15.04337798821885208, -2.682774720514427003, -27.31760573472296016 ) ) ;
#84688 = CARTESIAN_POINT ( 'NONE',  ( -32.62287095715004881, -29.50250243563736774, 8.947779886222150481 ) ) ;
#84689 = CARTESIAN_POINT ( 'NONE',  ( -5.517532219241116032, 20.92096086382833064, -1.500000000000002220 ) ) ;
#84690 = FACE_OUTER_BOUND ( 'NONE', #28900, .T. ) ;
#84691 = CARTESIAN_POINT ( 'NONE',  ( 2.844571010020486845, -19.19604305453586690, -1.500000000000002220 ) ) ;
#84692 = FACE_OUTER_BOUND ( 'NONE', #26467, .T. ) ;
#84693 = DIRECTION ( 'NONE',  ( 1.000000000000000000, 3.773278334444166432E-23, 8.201307841325785021E-29 ) ) ;
#84694 = CARTESIAN_POINT ( 'NONE',  ( 4.164567180745167185, 19.39263604865329071, -1.500000000000002220 ) ) ;
#84695 = EDGE_LOOP ( 'NONE', ( #73211, #54311, #73515, #26235 ) ) ;
#84696 = CARTESIAN_POINT ( 'NONE',  ( -16.58479117878708209, 11.75282063728064053, 11.49999999999999645 ) ) ;
#84697 = CARTESIAN_POINT ( 'NONE',  ( 22.02124265030973760, -7.835183881457444599, 17.60402280011862075 ) ) ;
#84699 = VECTOR ( 'NONE', #77670, 1000.000000000000000 ) ;
#84698 = CARTESIAN_POINT ( 'NONE',  ( -111.6228709571500559, -29.50250786944525672, 11.44777988621622988 ) ) ;
#84700 = ORIENTED_EDGE ( 'NONE', *, *, #32422, .F. ) ;
#84701 = CARTESIAN_POINT ( 'NONE',  ( -0.04154859658887635060, -22.51212076658054428, 1.420893871182737023 ) ) ;
#84702 = PLANE ( 'NONE',  #57420 ) ;
#84703 = DIRECTION ( 'NONE',  ( -0.09721092304694051167, 0.000000000000000000, 0.9952638024365005887 ) ) ;
#84704 = CARTESIAN_POINT ( 'NONE',  ( -128.6228709571499849, -23.73907113216991860, -1.053371485793219042 ) ) ;
#84705 = CARTESIAN_POINT ( 'NONE',  ( -0.5315124411682757843, -6.376774720514411854, 19.46509473978807847 ) ) ;
#84706 = CARTESIAN_POINT ( 'NONE',  ( -12.91570554291229023, -15.35452705144416896, -1.500000000000002220 ) ) ;
#84707 = DIRECTION ( 'NONE',  ( 0.000000000000000000, -1.000000000000000000, 1.478457507934778393E-16 ) ) ;
#84708 = CIRCLE ( 'NONE', #32872, 2.249999999999998668 ) ;
#84710 = VERTEX_POINT ( 'NONE', #67979 ) ;
#84709 = EDGE_CURVE ( 'NONE', #2149, #5650, #44111, .T. ) ;
#84711 = CARTESIAN_POINT ( 'NONE',  ( -24.90875734969025501, -5.965225279485572685, 26.43402280011862615 ) ) ;
#84712 = EDGE_CURVE ( 'NONE', #76106, #25473, #43048, .T. ) ;
#84713 = CARTESIAN_POINT ( 'NONE',  ( 22.85676281555306844, 1.471244944367766649, 11.49999999999999645 ) ) ;
#84714 = CARTESIAN_POINT ( 'NONE',  ( -13.58842472641693711, -18.21064416987719525, -1.500000000000002220 ) ) ;
#84715 = EDGE_LOOP ( 'NONE', ( #53183, #68018, #60155, #56422 ) ) ;
#84716 = DIRECTION ( 'NONE',  ( -0.000000000000000000, 1.000000000000000000, -0.000000000000000000 ) ) ;
#84717 = AXIS2_PLACEMENT_3D ( 'NONE', #64767, #97673, #41399 ) ;
#84718 = EDGE_CURVE ( 'NONE', #81032, #8388, #45633, .T. ) ;
#84719 = CARTESIAN_POINT ( 'NONE',  ( -28.52287095715007226, -23.32374950011072912, -1.443835813551990643 ) ) ;
#84720 = DIRECTION ( 'NONE',  ( -0.000000000000000000, 1.000000000000000000, -0.000000000000000000 ) ) ;
#84721 = EDGE_CURVE ( 'NONE', #14974, #82488, #53119, .T. ) ;
#84722 = CARTESIAN_POINT ( 'NONE',  ( -71.62287095715005592, -24.64898659630528854, 1.056161002820824368 ) ) ;
#84723 = CARTESIAN_POINT ( 'NONE',  ( 32.85081302853804885, 3.622774720514426949, -13.10817780685210643 ) ) ;
#84724 = DIRECTION ( 'NONE',  ( -0.000000000000000000, 2.173523156925979552E-06, -0.9999999999976378895 ) ) ;
#84725 = VERTEX_POINT ( 'NONE', #82184 ) ;
#84726 = CARTESIAN_POINT ( 'NONE',  ( 20.34676669208793953, -0.1217515720461415790, -1.500000000000002220 ) ) ;
#84727 = ORIENTED_EDGE ( 'NONE', *, *, #40866, .T. ) ;
#84728 = EDGE_CURVE ( 'NONE', #68982, #94726, #90803, .T. ) ;
#84729 = CARTESIAN_POINT ( 'NONE',  ( 12.94906671069258763, 19.00495796004926419, 11.49999999999998934 ) ) ;
#84730 = CARTESIAN_POINT ( 'NONE',  ( -54.51465898514846486, -23.73791477778911485, 11.05961554403171121 ) ) ;
#84731 = ORIENTED_EDGE ( 'NONE', *, *, #31497, .T. ) ;
#84732 = CARTESIAN_POINT ( 'NONE',  ( -108.5492781676227594, -24.66019654487200086, 8.947790411086106843 ) ) ;
#84733 = DIRECTION ( 'NONE',  ( -3.773278334453079618E-23, 0.9999999999976377785, 2.173523156925979975E-06 ) ) ;
#84734 = B_SPLINE_CURVE_WITH_KNOTS ( 'NONE', 3,
 ( #89556, #6803, #81938, #97169 ),
 .UNSPECIFIED., .F., .F.,
 ( 4, 4 ),
 ( 0.1005718158719557526, 0.1095782471440711753 ),
 .UNSPECIFIED. ) ;
#84735 = VECTOR ( 'NONE', #3234, 1000.000000000000114 ) ;
#84736 = CARTESIAN_POINT ( 'NONE',  ( -51.49549738738706850, -24.35071581493542681, 9.817618358456028815 ) ) ;
#84738 = ORIENTED_EDGE ( 'NONE', *, *, #35904, .T. ) ;
#84737 = CARTESIAN_POINT ( 'NONE',  ( -6.410030533929251817, 20.24415959294862333, 11.49999999999999645 ) ) ;
#84739 = ORGANIZATION ( 'NAUO-ORG9', 'UNSPECIFIED', 'UNSPECIFIED' ) ;
#84740 = ORIENTED_EDGE ( 'NONE', *, *, #53757, .T. ) ;
#84741 = CARTESIAN_POINT ( 'NONE',  ( 14.71430157977438924, -16.63553917435140406, 11.49999999999998934 ) ) ;
#84742 = CARTESIAN_POINT ( 'NONE',  ( -9.157874670058189892, -18.46812626297970539, 11.49999999999998934 ) ) ;
#84743 = VERTEX_POINT ( 'NONE', #21768 ) ;
#84745 = VERTEX_POINT ( 'NONE', #84179 ) ;
#84744 = CIRCLE ( 'NONE', #3716, 3.349999999999998757 ) ;
#84746 = CARTESIAN_POINT ( 'NONE',  ( -103.5228709571500758, -29.50248528299804818, 1.056150453629042030 ) ) ;
#84747 = CARTESIAN_POINT ( 'NONE',  ( 3.769931535195356620, -5.876774720514428729, 21.83933825178638699 ) ) ;
#84748 = EDGE_LOOP ( 'NONE', ( #33642, #90258, #84536, #44679 ) ) ;
#84749 = CARTESIAN_POINT ( 'NONE',  ( -91.64132767522438883, -23.48783264082477018, -1.443836473390090802 ) ) ;
#84750 = VERTEX_POINT ( 'NONE', #51749 ) ;
#84751 = VECTOR ( 'NONE', #32856, 1000.000000000000000 ) ;
#84752 = CARTESIAN_POINT ( 'NONE',  ( -126.8949125657483421, -25.24693556693654273, 3.801660433955577290 ) ) ;
#84753 = CARTESIAN_POINT ( 'NONE',  ( -44.52287095715006160, -23.72747288104469732, -1.053458166803227902 ) ) ;
#84754 = CARTESIAN_POINT ( 'NONE',  ( 19.92439739378097840, -5.974006126113303949, -1.500000000000002220 ) ) ;
#84755 = CARTESIAN_POINT ( 'NONE',  ( -4.706806674773570620, -21.25045708977441450, 11.49999999999999645 ) ) ;
#84756 = CARTESIAN_POINT ( 'NONE',  ( -27.96875734969026084, 6.376774720514426953, 26.43402280011862615 ) ) ;
#84757 = DIRECTION ( 'NONE',  ( 0.000000000000000000, 0.000000000000000000, 1.000000000000000000 ) ) ;
#84758 = CARTESIAN_POINT ( 'NONE',  ( -21.13723655771239152, -7.639886366525781014, 11.49999999999998934 ) ) ;
#84759 = CARTESIAN_POINT ( 'NONE',  ( 30.53060340732037048, 2.682774720514426559, -2.322449884495168870 ) ) ;
#84761 = ORIENTED_EDGE ( 'NONE', *, *, #32492, .T. ) ;
#84760 = ADVANCED_FACE ( 'NONE', ( #97899 ), #46598, .T. ) ;
#84762 = DIRECTION ( 'NONE',  ( 0.000000000000000000, -1.000000000000000000, 0.000000000000000000 ) ) ;
#84763 = CARTESIAN_POINT ( 'NONE',  ( -69.52287095715009002, -23.72773821059536914, 11.05748984161097326 ) ) ;
#84764 = B_SPLINE_SURFACE_WITH_KNOTS ( 'NONE', 3, 3, ( 
 ( #67699, #12387, #96626, #43360 ),
 ( #5777, #11401, #4788, #74781 ),
 ( #3802, #5279, #36239, #67201 ),
 ( #98114, #27128, #58093, #50465 ),
 ( #28620, #59584, #90514, #13378 ),
 ( #68184, #61582, #75776, #13879 ),
 ( #45844, #38217, #85388, #658 ) ),
 .UNSPECIFIED., .F., .F., .F.,
 ( 4, 3, 4 ),
 ( 4, 4 ),
 ( 0.7945040050992244751, 0.8970133687736503436, 0.9995227324480761011 ),
 ( 0.5396311249913389174, 0.5408929790830778739 ),
 .UNSPECIFIED. ) ;
#84765 = VERTEX_POINT ( 'NONE', #14669 ) ;
#84766 = ORIENTED_EDGE ( 'NONE', *, *, #21357, .F. ) ;
#84767 = EDGE_CURVE ( 'NONE', #26340, #23597, #7686, .T. ) ;
#84768 = ORIENTED_EDGE ( 'NONE', *, *, #87711, .F. ) ;
#84769 = CARTESIAN_POINT ( 'NONE',  ( 20.65877813657638740, 5.380652674160894655, -1.500000000000002220 ) ) ;
#84770 = ORIENTED_EDGE ( 'NONE', *, *, #32938, .F. ) ;
#84771 = CARTESIAN_POINT ( 'NONE',  ( -17.33045254171255678, -11.89390297951003816, 11.49999999999998934 ) ) ;
#84772 = CARTESIAN_POINT ( 'NONE',  ( -30.48808003178038462, -24.57318328807190966, 0.8299800598022502029 ) ) ;
#84773 = CARTESIAN_POINT ( 'NONE',  ( -41.46524908126663433, -25.28892609849224016, 4.157779739328558932 ) ) ;
#84774 = LINE ( 'NONE', #92384, #75720 ) ;
#84775 = CARTESIAN_POINT ( 'NONE',  ( -11.46427080702723522, -18.74017919159951973, -1.500000000000002220 ) ) ;
#84776 = CARTESIAN_POINT ( 'NONE',  ( -76.52287095715007581, -24.65952944569304606, 1.056160979905698794 ) ) ;
#84777 = EDGE_LOOP ( 'NONE', ( #45196, #32577, #74054, #82965 ) ) ;
#84778 = FACE_OUTER_BOUND ( 'NONE', #64182, .T. ) ;
#84779 = VECTOR ( 'NONE', #59695, 1000.000000000000000 ) ;
#84780 = CARTESIAN_POINT ( 'NONE',  ( -96.52287095715006160, -24.64898659630528499, 1.056161002820829697 ) ) ;
#84781 = CARTESIAN_POINT ( 'NONE',  ( 31.62401270459618630, -4.290926300276496796, 26.86768354919275836 ) ) ;
#84782 = AXIS2_PLACEMENT_3D ( 'NONE', #20557, #90082, #66269 ) ;
#84783 = CARTESIAN_POINT ( 'NONE',  ( -130.5728709571500303, -23.78062553189673523, -0.9709657327914292813 ) ) ;
#84784 = CARTESIAN_POINT ( 'NONE',  ( -0.07952141725841599396, -22.02053276243675128, 9.703205396196688426 ) ) ;
#84785 = CARTESIAN_POINT ( 'NONE',  ( -7.839647760473957838, 19.78794240023834661, -1.500000000000002220 ) ) ;
#84786 = CARTESIAN_POINT ( 'NONE',  ( -98.63223543337561239, -23.96169478059713853, 10.65365249895717881 ) ) ;
#84787 = B_SPLINE_CURVE_WITH_KNOTS ( 'NONE', 3,
 ( #18375, #56458, #65580, #96495, #17373, #26991 ),
 .UNSPECIFIED., .F., .F.,
 ( 4, 2, 4 ),
 ( 1.570887131794638196E-05, 0.001396322306279761940, 0.002776935741241577573 ),
 .UNSPECIFIED. ) ;
#84788 = PLANE ( 'NONE',  #80515 ) ;
#84789 = B_SPLINE_CURVE_WITH_KNOTS ( 'NONE', 3,
 ( #17419, #71714, #2212, #33141 ),
 .UNSPECIFIED., .F., .F.,
 ( 4, 4 ),
 ( 0.000000000000000000, 9.999999999998897304E-05 ),
 .UNSPECIFIED. ) ;
#84790 = CARTESIAN_POINT ( 'NONE',  ( -29.58953762381672092, -23.39424308723205570, 11.44779302747772221 ) ) ;
#84791 = CARTESIAN_POINT ( 'NONE',  ( -29.62287095715005592, -23.40871900810292772, -1.443836166241315055 ) ) ;
#84792 = PRODUCT_RELATED_PRODUCT_CATEGORY ( 'detail', '', ( #50676 ) ) ;
#84793 = CARTESIAN_POINT ( 'NONE',  ( 19.74966320730700176, -10.79507447929251107, -1.500000000000002220 ) ) ;
#84794 = CARTESIAN_POINT ( 'NONE',  ( -108.8765244897739279, -25.30561928443788133, 5.929683345795315752 ) ) ;
#84795 = ORIENTED_EDGE ( 'NONE', *, *, #26630, .F. ) ;
#84796 = FACE_OUTER_BOUND ( 'NONE', #85426, .T. ) ;
#84797 = CARTESIAN_POINT ( 'NONE',  ( 5.117700956428186565, 18.95590836763280862, 11.49999999999999645 ) ) ;
#84798 = CARTESIAN_POINT ( 'NONE',  ( 10.34999999999998010, 27.69999999999999929, 0.000000000000000000 ) ) ;
#84799 = CARTESIAN_POINT ( 'NONE',  ( -119.5228709571500474, -23.47593901973090524, -1.443836447538996204 ) ) ;
#84800 = ORIENTED_EDGE ( 'NONE', *, *, #67017, .T. ) ;
#84801 = CARTESIAN_POINT ( 'NONE',  ( -88.58338171500136582, -24.66019654487199730, 8.947790411086115725 ) ) ;
#84802 = CARTESIAN_POINT ( 'NONE',  ( -127.4728709571500360, -25.40558663563398767, 5.000950440326727531 ) ) ;
#84803 = EDGE_CURVE ( 'NONE', #72503, #4570, #66501, .T. ) ;
#84804 = CARTESIAN_POINT ( 'NONE',  ( -100.0218067620262303, -25.31439551943679689, 5.284572029636154689 ) ) ;
#84805 = CIRCLE ( 'NONE', #44336, 19.30000000000000071 ) ;
#84806 = CARTESIAN_POINT ( 'NONE',  ( -9.297559507673007317, 17.40068379117045083, -1.500000000000002220 ) ) ;
#84807 = ORIENTED_EDGE ( 'NONE', *, *, #78108, .T. ) ;
#84808 = CARTESIAN_POINT ( 'NONE',  ( 8.159923944583882260, 6.376774720514430506, -28.14238247108524149 ) ) ;
#84809 = CARTESIAN_POINT ( 'NONE',  ( -28.84663072490566194, 5.965225279485572685, 28.73989617533406715 ) ) ;
#84810 = AXIS2_PLACEMENT_3D ( 'NONE', #42797, #20926, #82827 ) ;
#84811 = PERSON_AND_ORGANIZATION ( #70597, #27821 ) ;
#84812 = ORIENTED_EDGE ( 'NONE', *, *, #75756, .T. ) ;
#84813 = CARTESIAN_POINT ( 'NONE',  ( -124.5228709571500758, -23.72773821059536914, 11.05748984161097326 ) ) ;
#84814 = DIRECTION ( 'NONE',  ( 0.000000000000000000, 0.9999999999976377785, 2.173523156925979975E-06 ) ) ;
#84815 = DIRECTION ( 'NONE',  ( -0.000000000000000000, -1.000000000000000000, 0.000000000000000000 ) ) ;
#84816 = CARTESIAN_POINT ( 'NONE',  ( -98.89303308397303738, -25.26638225912975599, 6.110950151213043746 ) ) ;
#84817 = CARTESIAN_POINT ( 'NONE',  ( -67.62287095715009855, -23.94994826722514958, -0.6494450866351695328 ) ) ;
#84818 = CARTESIAN_POINT ( 'NONE',  ( -94.52287095715006160, -24.65952944569304961, 1.056160979905700570 ) ) ;
#84819 = CIRCLE ( 'NONE', #23254, 2.000000000000000000 ) ;
#84820 = CARTESIAN_POINT ( 'NONE',  ( -61.52287095715006870, -23.96127896941632329, -0.6493128931038057994 ) ) ;
#84822 = EDGE_CURVE ( 'NONE', #53102, #68625, #46431, .T. ) ;
#84821 = CARTESIAN_POINT ( 'NONE',  ( -18.23705311251027794, 8.147635122911419003, 11.49999999999998934 ) ) ;
#84823 = CARTESIAN_POINT ( 'NONE',  ( -45.52287095715007581, -23.47593901973090169, -1.443836447538997092 ) ) ;
#84824 = CARTESIAN_POINT ( 'NONE',  ( -45.47439281453883808, -24.92592662359561118, 8.075495903018000021 ) ) ;
#84825 = ORIENTED_EDGE ( 'NONE', *, *, #61879, .T. ) ;
#84826 = B_SPLINE_CURVE_WITH_KNOTS ( 'NONE', 3,
 ( #31171, #62140, #23546, #49929, #40792, #18454 ),
 .UNSPECIFIED., .F., .F.,
 ( 4, 2, 4 ),
 ( 0.000000000000000000, 0.001380901958385392448, 0.002761803916770784895 ),
 .UNSPECIFIED. ) ;
#84827 = DIRECTION ( 'NONE',  ( -0.000000000000000000, 1.000000000000000000, 1.020425574104004246E-16 ) ) ;
#84828 = B_SPLINE_CURVE_WITH_KNOTS ( 'NONE', 3,
 ( #16530, #319, #2336, #17546, #86558, #47506 ),
 .UNSPECIFIED., .F., .F.,
 ( 4, 2, 4 ),
 ( 6.384118678620252359E-06, 0.001386860460828383875, 0.002767336802978147530 ),
 .UNSPECIFIED. ) ;
#84829 = CARTESIAN_POINT ( 'NONE',  ( -109.3592350823140720, -25.29012917042550512, 4.175497848340549822 ) ) ;
#84830 = ADVANCED_FACE ( 'NONE', ( #14162 ), #76553, .F. ) ;
#84831 = CARTESIAN_POINT ( 'NONE',  ( -120.6228709571500417, -24.63287334234178516, 0.9662140553045625024 ) ) ;
#84832 = CARTESIAN_POINT ( 'NONE',  ( 4.712727796232553779, -3.316774720514426456, -25.55789472434992859 ) ) ;
#84833 = EDGE_CURVE ( 'NONE', #18228, #67714, #27904, .T. ) ;
#84834 = CARTESIAN_POINT ( 'NONE',  ( -119.6228709571500275, -24.33832256527049154, 0.1851278514138672837 ) ) ;
#84835 = CARTESIAN_POINT ( 'NONE',  ( -83.55087393305831256, -24.15543982623907127, -0.2315651400026649820 ) ) ;
#84836 = B_SPLINE_SURFACE_WITH_KNOTS ( 'NONE', 3, 3, ( 
 ( #83954, #91562, #52018, #66767 ),
 ( #13939, #68240, #74838, #97190 ),
 ( #5336, #51524, #97686, #90079 ),
 ( #29668, #89581, #20551, #98175 ),
 ( #12938, #20062, #43905, #59640 ),
 ( #21049, #98673, #44412, #22041 ),
 ( #5835, #29169, #60144, #45408 ) ),
 .UNSPECIFIED., .F., .F., .F.,
 ( 4, 3, 4 ),
 ( 4, 4 ),
 ( 0.7945040050992230318, 0.8970133687736492334, 0.9995227324480754350 ),
 ( 0.03950403576920281934, 0.04053499800853590379 ),
 .UNSPECIFIED. ) ;
#84837 = CARTESIAN_POINT ( 'NONE',  ( -77.52287095715006160, -23.47596703998600631, 11.44779298504228571 ) ) ;
#84838 = CARTESIAN_POINT ( 'NONE',  ( -40.52287095715005449, -24.99156044556202261, 7.747789690856173195 ) ) ;
#84839 = ORIENTED_EDGE ( 'NONE', *, *, #31526, .F. ) ;
#84840 = CARTESIAN_POINT ( 'NONE',  ( -0.6865706486018943178, -20.24796467851281179, -1.500000000000002220 ) ) ;
#84841 = CARTESIAN_POINT ( 'NONE',  ( -101.6228709571500559, -23.47593901973091235, -1.443836447539001089 ) ) ;
#84842 = EDGE_CURVE ( 'NONE', #78009, #5411, #59562, .T. ) ;
#84843 = DIRECTION ( 'NONE',  ( -1.000000000000000000, 0.000000000000000000, 0.000000000000000000 ) ) ;
#84844 = VECTOR ( 'NONE', #29615, 1000.000000000000000 ) ;
#84845 = DIRECTION ( 'NONE',  ( 0.000000000000000000, 0.000000000000000000, -1.000000000000000000 ) ) ;
#84846 = ORIENTED_EDGE ( 'NONE', *, *, #44736, .T. ) ;
#84847 = DIRECTION ( 'NONE',  ( 0.000000000000000000, 0.9999999999976377785, 2.173523156925979975E-06 ) ) ;
#84848 = CARTESIAN_POINT ( 'NONE',  ( 17.00595499256408871, 10.69956108467327205, -1.500000000000002220 ) ) ;
#84849 = VECTOR ( 'NONE', #99325, 1000.000000000000114 ) ;
#84850 = CARTESIAN_POINT ( 'NONE',  ( 10.44912437418449969, 18.32051524777507723, 11.49999999999999645 ) ) ;
#84851 = DIRECTION ( 'NONE',  ( 1.334402673828313339E-16, 0.000000000000000000, -1.000000000000000000 ) ) ;
#84852 = CARTESIAN_POINT ( 'NONE',  ( -11.88820881604258339, -18.65297325734525913, -1.500000000000002220 ) ) ;
#84853 = CARTESIAN_POINT ( 'NONE',  ( 20.52540449432101610, 0.9483640940595650104, 11.49999999999998934 ) ) ;
#84854 = CARTESIAN_POINT ( 'NONE',  ( -95.60349032644573697, -23.48783264082477373, -1.443836473390088804 ) ) ;
#84855 = CARTESIAN_POINT ( 'NONE',  ( -126.6228709571500275, -24.50216790748207529, 0.6166512839542536151 ) ) ;
#84856 = ORIENTED_EDGE ( 'NONE', *, *, #96458, .T. ) ;
#84857 = DIRECTION ( 'NONE',  ( 0.000000000000000000, -2.173523156925979552E-06, 0.9999999999976378895 ) ) ;
#84858 = ORIENTED_EDGE ( 'NONE', *, *, #45630, .F. ) ;
#84859 = CARTESIAN_POINT ( 'NONE',  ( -51.62287095715006302, -24.50216790748205753, 0.6166512839542510616 ) ) ;
#84860 = CARTESIAN_POINT ( 'NONE',  ( -87.58953762381672448, -24.66019654487199730, 8.947790411086121054 ) ) ;
#84861 = ORIENTED_EDGE ( 'NONE', *, *, #24368, .T. ) ;
#84862 = EDGE_LOOP ( 'NONE', ( #54769, #72239, #92944, #17375 ) ) ;
#84863 = ORIENTED_EDGE ( 'NONE', *, *, #28808, .T. ) ;
#84864 = FACE_OUTER_BOUND ( 'NONE', #25344, .T. ) ;
#84865 = CARTESIAN_POINT ( 'NONE',  ( -31.52287095715006160, -23.47593901973090169, -1.443836447538997536 ) ) ;
#84866 = CARTESIAN_POINT ( 'NONE',  ( 0.3180806761505774460, -6.376774720514415407, 20.02963804100705403 ) ) ;
#84867 = CARTESIAN_POINT ( 'NONE',  ( -18.22997975830956108, -9.740667652671243459, -1.500000000000002220 ) ) ;
#84868 = EDGE_CURVE ( 'NONE', #30829, #33008, #34407, .T. ) ;
#84869 = CARTESIAN_POINT ( 'NONE',  ( 18.62697458635512859, 10.92912097662538251, 11.49999999999999645 ) ) ;
#84870 = ORIENTED_EDGE ( 'NONE', *, *, #27114, .F. ) ;
#84871 = CARTESIAN_POINT ( 'NONE',  ( -83.62287095714999907, -24.33832256526968862, 0.1851278514119905905 ) ) ;
#84872 = CARTESIAN_POINT ( 'NONE',  ( -60.62287095715006302, -24.62226745350437085, 0.9660975649728084091 ) ) ;
#84873 = CARTESIAN_POINT ( 'NONE',  ( -8.633843874998758494, 20.65557450359631630, -1.500000000000002220 ) ) ;
#84874 = CARTESIAN_POINT ( 'NONE',  ( -79.85862890617264043, -25.27875051067252699, 6.918725483278709731 ) ) ;
#84875 = DIRECTION ( 'NONE',  ( 3.773278334444166432E-23, -1.000000000000000000, 0.000000000000000000 ) ) ;
#84876 = ORIENTED_EDGE ( 'NONE', *, *, #73062, .T. ) ;
#84877 = PLANE ( 'NONE',  #69549 ) ;
#84878 = CARTESIAN_POINT ( 'NONE',  ( -49.58722086695681952, -24.35071581493542325, 9.817618358456035921 ) ) ;
#84879 = CARTESIAN_POINT ( 'NONE',  ( -29.49875734969025842, -5.965225279485572685, 23.37402280011862743 ) ) ;
#84880 = CARTESIAN_POINT ( 'NONE',  ( -13.90609606471210391, -15.62508359690603221, 11.49999999999998934 ) ) ;
#84881 = ORIENTED_EDGE ( 'NONE', *, *, #87524, .F. ) ;
#84882 = CARTESIAN_POINT ( 'NONE',  ( -86.55120064081188502, -24.15543982623907837, -0.2315651400026493834 ) ) ;
#84883 = EDGE_LOOP ( 'NONE', ( #56564, #41490, #81017, #76790 ) ) ;
#84884 = EDGE_CURVE ( 'NONE', #99016, #50353, #52248, .T. ) ;
#84885 = CARTESIAN_POINT ( 'NONE',  ( -109.6235285740488479, -24.66019654487200441, 8.947790411086113949 ) ) ;
#84886 = CARTESIAN_POINT ( 'NONE',  ( 21.17954554857512761, 0.9134790845329443520, -1.500000000000002220 ) ) ;
#84887 = VERTEX_POINT ( 'NONE', #83175 ) ;
#84888 = CARTESIAN_POINT ( 'NONE',  ( -93.62287095715005592, -29.50250243563736774, 8.947779886222139822 ) ) ;
#84889 = DIRECTION ( 'NONE',  ( 0.000000000000000000, -1.000000000000000000, 1.478457507934778393E-16 ) ) ;
#84890 = CARTESIAN_POINT ( 'NONE',  ( -21.42251255223715134, 3.917230396363152067, -1.500000000000002220 ) ) ;
#84891 = CARTESIAN_POINT ( 'NONE',  ( -7.567681410454951241, -6.376774720514411854, 19.71630089903357330 ) ) ;
#84892 = VECTOR ( 'NONE', #89801, 1000.000000000000000 ) ;
#84893 = CARTESIAN_POINT ( 'NONE',  ( -35.52287095715006870, -24.99156044556120193, 7.747789690856173195 ) ) ;
#84894 = CARTESIAN_POINT ( 'NONE',  ( -79.35269453762862213, -25.26523176223116351, 6.110756246060513597 ) ) ;
#84895 = CARTESIAN_POINT ( 'NONE',  ( -0.06377455873143267340, 21.83884041771831619, -1.500000000000002220 ) ) ;
#84896 = CARTESIAN_POINT ( 'NONE',  ( -0.5218785734906133955, -6.376774720514408301, 19.14848118821636547 ) ) ;
#84897 = ORIENTED_EDGE ( 'NONE', *, *, #54068, .T. ) ;
#84898 = CARTESIAN_POINT ( 'NONE',  ( 7.480769230769231726, -5.876774720514430506, 20.77403846153845635 ) ) ;
#84899 = DIRECTION ( 'NONE',  ( -3.773278334453079618E-23, 0.9999999999976377785, 2.173523156925979975E-06 ) ) ;
#84900 = DIRECTION ( 'NONE',  ( 1.000000000000000000, 3.773278334444167608E-23, 8.201307833595939069E-29 ) ) ;
#84901 = ORIENTED_EDGE ( 'NONE', *, *, #62600, .F. ) ;
#84902 = EDGE_LOOP ( 'NONE', ( #65619, #83647, #60347, #98080 ) ) ;
#84903 = ORIENTED_EDGE ( 'NONE', *, *, #48534, .F. ) ;
#84904 = PLANE ( 'NONE',  #30260 ) ;
#84905 = CARTESIAN_POINT ( 'NONE',  ( 13.55612473118199723, -16.30799122071102403, 11.49999999999998934 ) ) ;
#84906 = CARTESIAN_POINT ( 'NONE',  ( -94.62356957389862089, -24.65952944569304606, 1.056160979905703234 ) ) ;
#84907 = CARTESIAN_POINT ( 'NONE',  ( -79.05725560372792415, -25.03138091265075715, 6.604864886565241733 ) ) ;
#84908 = DIRECTION ( 'NONE',  ( -1.000000000000000000, 0.000000000000000000, 0.000000000000000000 ) ) ;
#84909 = DIRECTION ( 'NONE',  ( 0.7512896232465892110, 0.000000000000000000, 0.6599726524652350657 ) ) ;
#84910 = EDGE_CURVE ( 'NONE', #69181, #5121, #55255, .T. ) ;
#84911 = CARTESIAN_POINT ( 'NONE',  ( -13.40542139710017899, 13.98966777563825481, 11.49999999999998934 ) ) ;
#84912 = CARTESIAN_POINT ( 'NONE',  ( -39.97884473287227536, -25.31392318313163159, 5.203682277190879724 ) ) ;
#84913 = ORIENTED_EDGE ( 'NONE', *, *, #43162, .F. ) ;
#84914 = CARTESIAN_POINT ( 'NONE',  ( 19.29218144733592055, -2.436590042558338443, 11.49999999999999645 ) ) ;
#84915 = DIRECTION ( 'NONE',  ( -3.773278334453080206E-23, 0.9999999999976377785, 2.173523156925979975E-06 ) ) ;
#84916 = EDGE_CURVE ( 'NONE', #76505, #24959, #16169, .T. ) ;
#84917 = CARTESIAN_POINT ( 'NONE',  ( 14.52511747680497933, 5.965225279485572685, -27.86035006098926559 ) ) ;
#84918 = ORIENTED_EDGE ( 'NONE', *, *, #32938, .T. ) ;
#84919 = AXIS2_PLACEMENT_3D ( 'NONE', #48690, #24327, #48180 ) ;
#84920 = DIRECTION ( 'NONE',  ( 0.09824042138329590335, -4.470611911092166224E-17, 0.9951627101165079203 ) ) ;
#84921 = EDGE_CURVE ( 'NONE', #73116, #82155, #7562, .T. ) ;
#84922 = LINE ( 'NONE', #15905, #46580 ) ;
#84923 = EDGE_CURVE ( 'NONE', #21553, #57117, #72529, .T. ) ;
#84924 = FACE_OUTER_BOUND ( 'NONE', #40991, .T. ) ;
#84925 = CARTESIAN_POINT ( 'NONE',  ( -34.52287095715006160, -23.48786465467240347, 11.44779295918255357 ) ) ;
#84926 = CARTESIAN_POINT ( 'NONE',  ( 16.02095076306289201, 11.36058263404076030, 11.49999999999998934 ) ) ;
#84927 = CARTESIAN_POINT ( 'NONE',  ( -41.46611000704998418, -25.31583576900412424, 4.188173601412459313 ) ) ;
#84929 = EDGE_CURVE ( 'NONE', #76612, #64842, #93695, .T. ) ;
#84928 = ORIENTED_EDGE ( 'NONE', *, *, #4256, .F. ) ;
#84930 = CARTESIAN_POINT ( 'NONE',  ( -11.65619939812097527, 18.16556634249905855, 11.49999999999998934 ) ) ;
#84931 = CARTESIAN_POINT ( 'NONE',  ( -15.82668884360736961, -6.475225279485576024, 42.07822029717483758 ) ) ;
#84932 = CARTESIAN_POINT ( 'NONE',  ( -20.27875734969026311, -7.835183881457444599, 25.40402280011862146 ) ) ;
#84933 = CARTESIAN_POINT ( 'NONE',  ( 23.91005183030481263, 2.682774720514426559, -14.40591128290692069 ) ) ;
#84934 = CARTESIAN_POINT ( 'NONE',  ( 20.16173082093541424, 11.17373015621797627, -1.500000000000002220 ) ) ;
#84935 = CALENDAR_DATE ( 2026, 9, 10 ) ;
#84936 = CARTESIAN_POINT ( 'NONE',  ( -120.5228709571500616, -23.47593901973090524, -1.443836447538996204 ) ) ;
#84937 = CARTESIAN_POINT ( 'NONE',  ( 6.573941812937369455, -7.905506363763796338E-18, 0.2639660507643297183 ) ) ;
#84938 = CARTESIAN_POINT ( 'NONE',  ( -121.5888783905858190, -24.51419770103157347, 9.386484678747175181 ) ) ;
#84939 = CARTESIAN_POINT ( 'NONE',  ( -100.9084866940463883, -25.05508145465318748, 7.506936236879250934 ) ) ;
#84940 = CARTESIAN_POINT ( 'NONE',  ( 5.641025641025643189, -5.876774720514419847, 20.78665865384615330 ) ) ;
#84941 = CARTESIAN_POINT ( 'NONE',  ( -129.5220747276651139, -23.96119346886880663, -0.6495511937831975890 ) ) ;
#84942 = B_SPLINE_CURVE_WITH_KNOTS ( 'NONE', 3,
 ( #95600, #39808, #9861, #72276, #17473, #24577 ),
 .UNSPECIFIED., .F., .F.,
 ( 4, 2, 4 ),
 ( 6.391158118972359742E-06, 0.001387004593080793519, 0.002767618028042614572 ),
 .UNSPECIFIED. ) ;
#84943 = CARTESIAN_POINT ( 'NONE',  ( -99.19491584893809488, -25.26400770206901214, 4.406300587698978255 ) ) ;
#84945 = ADVANCED_FACE ( 'NONE', ( #68962 ), #8567, .T. ) ;
#84944 = CARTESIAN_POINT ( 'NONE',  ( 4.300141163375406528, 19.41444791797076874, -1.500000000000002220 ) ) ;
#84946 = CARTESIAN_POINT ( 'NONE',  ( -28.98875734969026041, 5.965225279485572685, 26.43402280011862615 ) ) ;
#84947 = CARTESIAN_POINT ( 'NONE',  ( -12.28770250403618114, -15.54288071925545722, -1.500000000000002220 ) ) ;
#84948 = CARTESIAN_POINT ( 'NONE',  ( -56.63256988609624898, -24.34968618360933590, 0.1864209137778786995 ) ) ;
#84949 = CARTESIAN_POINT ( 'NONE',  ( -39.22373867983765194, -25.29116667761266513, 3.518977199090397079 ) ) ;
#84950 = CARTESIAN_POINT ( 'NONE',  ( -5.576923076923074873, -6.376774720514427841, 21.75000000000000711 ) ) ;
#84951 = CARTESIAN_POINT ( 'NONE',  ( 18.38559056850662543, 9.607341378227904016, 11.49999999999999645 ) ) ;
#84952 = CARTESIAN_POINT ( 'NONE',  ( -41.32836283488544638, 2.682774720514426559, 39.26872235229541985 ) ) ;
#84953 = EDGE_CURVE ( 'NONE', #65212, #3035, #952, .T. ) ;
#84954 = PLANE ( 'NONE',  #89508 ) ;
#84955 = CARTESIAN_POINT ( 'NONE',  ( 16.28376985728763415, 15.88423345705086298, 11.49999999999999645 ) ) ;
#84956 = VERTEX_POINT ( 'NONE', #15166 ) ;
#84957 = CARTESIAN_POINT ( 'NONE',  ( -0.6703829557040269504, 4.102177322343282917, -2.677392948487098267E-15 ) ) ;
#84958 = ADVANCED_FACE ( 'NONE', ( #99886 ), #30897, .F. ) ;
#84959 = CARTESIAN_POINT ( 'NONE',  ( -106.6228709571501128, -23.94994826722566117, -0.6494450866342750261 ) ) ;
#84960 = CARTESIAN_POINT ( 'NONE',  ( 20.15506735835773000, -1.303320585059813741, 11.49999999999998934 ) ) ;
#84961 = FACE_OUTER_BOUND ( 'NONE', #84883, .T. ) ;
#84962 = EDGE_CURVE ( 'NONE', #78010, #55098, #24776, .T. ) ;
#84963 = CARTESIAN_POINT ( 'NONE',  ( -52.52287095715006160, -24.50321055353804311, 9.387540953477529371 ) ) ;
#84964 = ORIENTED_EDGE ( 'NONE', *, *, #32810, .T. ) ;
#84965 = EDGE_CURVE ( 'NONE', #100338, #14117, #2971, .T. ) ;
#84966 = EDGE_LOOP ( 'NONE', ( #93451, #95127, #12247, #56615 ) ) ;
#84967 = CARTESIAN_POINT ( 'NONE',  ( 0.3545156366401029935, -6.376774720514413630, 20.17598923696321478 ) ) ;
#84968 = CARTESIAN_POINT ( 'NONE',  ( -12.24191887126339751, 19.33842681661653984, -1.500000000000002220 ) ) ;
#84970 = EDGE_CURVE ( 'NONE', #58107, #11670, #52554, .T. ) ;
#84969 = CARTESIAN_POINT ( 'NONE',  ( -51.28182533633388829, -25.27420685139605894, 3.855515792242854012 ) ) ;
#84971 = CARTESIAN_POINT ( 'NONE',  ( -21.09935167195790839, -4.734744157926700225, -1.500000000000002220 ) ) ;
#84972 = FACE_OUTER_BOUND ( 'NONE', #40717, .T. ) ;
#84973 = FACE_OUTER_BOUND ( 'NONE', #10150, .T. ) ;
#84974 = CARTESIAN_POINT ( 'NONE',  ( -7.049398010371669798, 19.71092172866906012, 11.49999999999999645 ) ) ;
#84975 = VERTEX_POINT ( 'NONE', #23780 ) ;
#84976 = CARTESIAN_POINT ( 'NONE',  ( -124.5211395258430400, -23.96119346886880663, -0.6495511937832024740 ) ) ;
#84977 = CARTESIAN_POINT ( 'NONE',  ( -21.99024891984110752, 1.279939690139831665, 11.49999999999998934 ) ) ;
#84978 = B_SPLINE_CURVE_WITH_KNOTS ( 'NONE', 3,
 ( #79933, #47999, #9923, #2831, #79431, #32760, #25139, #56121 ),
 .UNSPECIFIED., .F., .F.,
 ( 4, 2, 2, 4 ),
 ( 0.000000000000000000, 0.003897507692133500394, 0.005846261538200250157, 0.007795015384267000788 ),
 .UNSPECIFIED. ) ;
#84979 = CARTESIAN_POINT ( 'NONE',  ( -105.6382438712245460, -23.48786465467241769, 11.44779295918254114 ) ) ;
#84980 = CARTESIAN_POINT ( 'NONE',  ( -30.47287095715008576, -24.38457522042859438, 9.689408350323725827 ) ) ;
#84981 = VERTEX_POINT ( 'NONE', #54252 ) ;
#84982 = CARTESIAN_POINT ( 'NONE',  ( 4.403244164709623654, -6.376774720514404748, 18.35516266052912826 ) ) ;
#84983 = DIRECTION ( 'NONE',  ( -0.000000000000000000, 2.173523156925979552E-06, -0.9999999999976378895 ) ) ;
#84984 = ORIENTED_EDGE ( 'NONE', *, *, #83202, .T. ) ;
#84985 = PLANE ( 'NONE',  #54994 ) ;
#84986 = ORIENTED_EDGE ( 'NONE', *, *, #72694, .T. ) ;
#84987 = ORIENTED_EDGE ( 'NONE', *, *, #61154, .F. ) ;
#84988 = CARTESIAN_POINT ( 'NONE',  ( -71.54955542377307154, -24.15620529776628445, 10.23563542870660115 ) ) ;
#84989 = CARTESIAN_POINT ( 'NONE',  ( -101.7667076177128678, -25.10936043410780982, 3.940952065299377249 ) ) ;
#84990 = CARTESIAN_POINT ( 'NONE',  ( -4.533825836049095059, -6.376774720514411854, 19.59623724171353132 ) ) ;
#84991 = CARTESIAN_POINT ( 'NONE',  ( -12.74120943341865342, -16.01528480738631899, -1.500000000000002220 ) ) ;
#84992 = AXIS2_PLACEMENT_3D ( 'NONE', #87235, #10115, #41075 ) ;
#84993 = ORIENTED_EDGE ( 'NONE', *, *, #6847, .T. ) ;
#84994 = CARTESIAN_POINT ( 'NONE',  ( -110.5895376238167387, -24.99156044556202971, 7.747789690856174083 ) ) ;
#84995 = CARTESIAN_POINT ( 'NONE',  ( -44.56061633354861584, -23.73766607897669800, -1.055555164236459120 ) ) ;
#84996 = DIRECTION ( 'NONE',  ( 0.000000000000000000, 1.478457507934778393E-16, -1.000000000000000000 ) ) ;
#84997 = CARTESIAN_POINT ( 'NONE',  ( 17.40631026334068565, 13.93540124644318645, 11.49999999999998934 ) ) ;
#84998 = CARTESIAN_POINT ( 'NONE',  ( -24.97666371003640506, 0.3587747205143964613, -15.72894043976419454 ) ) ;
#84999 = CARTESIAN_POINT ( 'NONE',  ( -91.52287095715006160, -24.33832256527048088, 0.1851278514138647024 ) ) ;
#85000 = VERTEX_POINT ( 'NONE', #40012 ) ;
#85001 = DIRECTION ( 'NONE',  ( -1.000000000000000000, -0.000000000000000000, -0.000000000000000000 ) ) ;
#85002 = CARTESIAN_POINT ( 'NONE',  ( -39.52287095715006870, -23.48786465467241058, 11.44779295918255180 ) ) ;
#85003 = CARTESIAN_POINT ( 'NONE',  ( -14.80784184970232431, -14.63167926507950689, -1.500000000000002220 ) ) ;
#85004 = VERTEX_POINT ( 'NONE', #77556 ) ;
#85006 = ORIENTED_EDGE ( 'NONE', *, *, #27621, .T. ) ;
#85005 = DIRECTION ( 'NONE',  ( 0.000000000000000000, 0.000000000000000000, -1.000000000000000000 ) ) ;
#85007 = CARTESIAN_POINT ( 'NONE',  ( -98.52287095715009002, -24.51387760970724727, 9.387446482453409402 ) ) ;
#85008 = ORIENTED_EDGE ( 'NONE', *, *, #14916, .T. ) ;
#85009 = ORIENTED_EDGE ( 'NONE', *, *, #71038, .F. ) ;
#85010 = CARTESIAN_POINT ( 'NONE',  ( -31.62287095715005236, -29.50248528299804818, 1.056150453629029817 ) ) ;
#85011 = CARTESIAN_POINT ( 'NONE',  ( -121.5895376238167245, -23.48786465467241769, 11.44779295918253759 ) ) ;
#85012 = CARTESIAN_POINT ( 'NONE',  ( 6.948977015814011615, -5.356774720514426491, -25.20533573604597066 ) ) ;
#85013 = LINE ( 'NONE', #30736, #4808 ) ;
#85014 = CARTESIAN_POINT ( 'NONE',  ( -92.63718633548049297, -23.73791477778911840, 11.05961554403170588 ) ) ;
#85015 = PLANE ( 'NONE',  #90206 ) ;
#85017 = EDGE_LOOP ( 'NONE', ( #62679, #60499, #35706, #16737 ) ) ;
#85016 = CARTESIAN_POINT ( 'NONE',  ( 0.7529269182969693386, -22.20201975079678647, 11.49999999999999645 ) ) ;
#85018 = CARTESIAN_POINT ( 'NONE',  ( -105.5562042904834215, -23.47596703998600631, 11.44779298504227683 ) ) ;
#85019 = ORIENTED_EDGE ( 'NONE', *, *, #53378, .T. ) ;
#85020 = CARTESIAN_POINT ( 'NONE',  ( 21.71957326813621592, -6.446789169762093152, -1.500000000000002220 ) ) ;
#85021 = B_SPLINE_CURVE_WITH_KNOTS ( 'NONE', 3,
 ( #86512, #16996, #47963, #88522 ),
 .UNSPECIFIED., .F., .F.,
 ( 4, 4 ),
 ( 0.7303074191294323114, 0.7393138504015477341 ),
 .UNSPECIFIED. ) ;
#85023 = ORIENTED_EDGE ( 'NONE', *, *, #81295, .F. ) ;
#85022 = CARTESIAN_POINT ( 'NONE',  ( -115.5567998953322046, -23.85049219812686871, 10.88485053497526778 ) ) ;
#85024 = EDGE_LOOP ( 'NONE', ( #61895, #89219, #26709, #35133 ) ) ;
#85025 = VECTOR ( 'NONE', #30903, 1000.000000000000000 ) ;
#85026 = LINE ( 'NONE', #30747, #75806 ) ;
#85027 = EDGE_CURVE ( 'NONE', #54547, #44198, #39007, .T. ) ;
#85028 = CARTESIAN_POINT ( 'NONE',  ( -14.78635263257777233, 13.65558988533819473, 11.49999999999998934 ) ) ;
#85029 = B_SPLINE_SURFACE_WITH_KNOTS ( 'NONE', 3, 3, ( 
 ( #16181, #54263, #8072, #39019 ),
 ( #93297, #55266, #39527, #31916 ),
 ( #93807, #24300, #86198, #16681 ),
 ( #1976, #26799, #79584, #19175 ),
 ( #32919, #81087, #10074, #57762 ),
 ( #88208, #26302, #9573, #27301 ),
 ( #10569, #87198, #11563, #40538 ) ),
 .UNSPECIFIED., .F., .F., .F.,
 ( 4, 3, 4 ),
 ( 4, 4 ),
 ( 0.7945040050992245861, 0.8970133687736504546, 0.9995227324480763231 ),
 ( 0.7396819606801936509, 0.7410361715128946924 ),
 .UNSPECIFIED. ) ;
#85030 = LINE ( 'NONE', #45989, #21381 ) ;
#85031 = VERTEX_POINT ( 'NONE', #38012 ) ;
#85032 = CARTESIAN_POINT ( 'NONE',  ( -89.81226385320383088, -25.26364009184147008, 3.993462176398974162 ) ) ;
#85033 = CARTESIAN_POINT ( 'NONE',  ( 18.00092565640838416, -13.26076702590692769, -1.500000000000002220 ) ) ;
#85034 = EDGE_LOOP ( 'NONE', ( #23939, #863, #1146, #77628 ) ) ;
#85035 = ORIENTED_EDGE ( 'NONE', *, *, #79352, .T. ) ;
#85036 = FACE_OUTER_BOUND ( 'NONE', #64973, .T. ) ;
#85037 = CARTESIAN_POINT ( 'NONE',  ( -4.495793269230770939, -5.876774720514410077, 19.27714342948718595 ) ) ;
#85038 = DIRECTION ( 'NONE',  ( -0.6401411605457395515, 0.000000000000000000, -0.7682573101345366862 ) ) ;
#85039 = ADVANCED_FACE ( 'NONE', ( #22765 ), #45318, .T. ) ;
#85040 = ADVANCED_FACE ( 'NONE', ( #19163 ), #42531, .T. ) ;
#85041 = CARTESIAN_POINT ( 'NONE',  ( 2.230654205607476737, -0.1647943925233645579, -7.922169807384186089E-16 ) ) ;
#85042 = ADVANCED_FACE ( 'NONE', ( #1965 ), #6422, .T. ) ;
#85043 = FACE_BOUND ( 'NONE', #8003, .T. ) ;
#85044 = CARTESIAN_POINT ( 'NONE',  ( -5.499840656826012975, 18.73951620154120334, -1.500000000000002220 ) ) ;
#85045 = CARTESIAN_POINT ( 'NONE',  ( -5.706951327759631099, -5.876774720514412742, 19.48569229636961353 ) ) ;
#85046 = EDGE_CURVE ( 'NONE', #97326, #45914, #43416, .T. ) ;
#85047 = CARTESIAN_POINT ( 'NONE',  ( 19.19993882694861753, 9.668096177433461946, 11.49999999999998934 ) ) ;
#85048 = CARTESIAN_POINT ( 'NONE',  ( -36.52287095715006870, -23.73907113216988307, -1.053371485793256124 ) ) ;
#85049 = LINE ( 'NONE', #1833, #93434 ) ;
#85050 = CARTESIAN_POINT ( 'NONE',  ( -71.58953762381672448, -23.48786465467241413, 11.44779295918254469 ) ) ;
#85051 = DIRECTION ( 'NONE',  ( 0.000000000000000000, -1.000000000000000000, 0.000000000000000000 ) ) ;
#85053 = CIRCLE ( 'NONE', #16966, 0.3000000000000016542 ) ;
#85052 = CARTESIAN_POINT ( 'NONE',  ( 19.82229641098322404, 11.46754112681587046, -1.500000000000002220 ) ) ;
#85054 = DATE_TIME_ROLE ( 'creation_date' ) ;
#85055 = CARTESIAN_POINT ( 'NONE',  ( -85.52287095715006160, -23.47596703998600631, 11.44779298504228393 ) ) ;
#85056 = CARTESIAN_POINT ( 'NONE',  ( -51.52764846858840997, -25.25773520710183817, 6.187572766161611781 ) ) ;
#85057 = CARTESIAN_POINT ( 'NONE',  ( -6.237196068801617699, -19.06703463882530158, 11.49999999999999645 ) ) ;
#85058 = CARTESIAN_POINT ( 'NONE',  ( -80.21014334459538020, -25.26612374374091630, 4.508707588862841398 ) ) ;
#85059 = DIRECTION ( 'NONE',  ( -3.773278334453079618E-23, 0.9999999999976377785, 2.173523156925978705E-06 ) ) ;
#85060 = CARTESIAN_POINT ( 'NONE',  ( -4.568292318365942073, 0.3587747205144265483, 30.06720597538392425 ) ) ;
#85061 = FACE_OUTER_BOUND ( 'NONE', #54407, .T. ) ;
#85062 = ORIENTED_EDGE ( 'NONE', *, *, #3191, .T. ) ;
#85063 = CARTESIAN_POINT ( 'NONE',  ( -109.5228709571500758, -23.72747288104470798, -1.053458166803225682 ) ) ;
#85064 = ADVANCED_FACE ( 'NONE', ( #19660 ), #20960, .T. ) ;
#85065 = DIRECTION ( 'NONE',  ( 0.000000000000000000, 0.000000000000000000, 1.000000000000000000 ) ) ;
#85066 = VECTOR ( 'NONE', #79636, 1000.000000000000114 ) ;
#85067 = CARTESIAN_POINT ( 'NONE',  ( -21.04499429308205549, 5.405531755741471045, -1.500000000000002220 ) ) ;
#85068 = CARTESIAN_POINT ( 'NONE',  ( -0.7638880233336634573, -9.374108182320437521, -9.000000000000000000 ) ) ;
#85069 = CARTESIAN_POINT ( 'NONE',  ( -19.57149217635686966, 1.386223266712492297, -1.500000000000002220 ) ) ;
#85070 = VECTOR ( 'NONE', #56689, 1000.000000000000114 ) ;
#85071 = CARTESIAN_POINT ( 'NONE',  ( -128.5562042904833788, -24.64898659630529565, 1.056161002820832806 ) ) ;
#85072 = EDGE_CURVE ( 'NONE', #76499, #27790, #21157, .T. ) ;
#85073 = CARTESIAN_POINT ( 'NONE',  ( -109.6235167689328591, -25.31698100855897593, 4.923693415162312625 ) ) ;
#85074 = PERSON_AND_ORGANIZATION_ROLE ( 'classification_officer' ) ;
#85075 = DIRECTION ( 'NONE',  ( -3.773278334444166432E-23, 1.000000000000000000, 0.000000000000000000 ) ) ;
#85076 = CARTESIAN_POINT ( 'NONE',  ( 2.880689065218799083, -6.376774720514426065, 21.31732089891691828 ) ) ;
#85077 = CARTESIAN_POINT ( 'NONE',  ( -18.72588118538106272, -8.511115862834014223, 11.49999999999999645 ) ) ;
#85078 = CARTESIAN_POINT ( 'NONE',  ( -39.07219716201183246, -25.30584882308033912, 4.512390342206024307 ) ) ;
#85079 = EDGE_CURVE ( 'NONE', #44226, #50353, #54890, .T. ) ;
#85080 = DIRECTION ( 'NONE',  ( 0.000000000000000000, 0.000000000000000000, -1.000000000000000000 ) ) ;
#85081 = ORIENTED_EDGE ( 'NONE', *, *, #9698, .T. ) ;
#85082 = SHAPE_REPRESENTATION_RELATIONSHIP ( 'NONE' , 'NONE' ,  #50921, #12552 ) ;
#85083 = CARTESIAN_POINT ( 'NONE',  ( -46.62287095715006302, -23.96127896941632685, -0.6493128931037863705 ) ) ;
#85084 = CARTESIAN_POINT ( 'NONE',  ( -39.98073487448829155, -25.28892444151557939, 3.395433753900389373 ) ) ;
#85085 = CARTESIAN_POINT ( 'NONE',  ( -125.5196039661687877, -24.83644354573579349, 8.397322867130096569 ) ) ;
#85086 = CARTESIAN_POINT ( 'NONE',  ( -121.6228709571500417, -24.64965695001469115, 8.947790433994175174 ) ) ;
#85087 = PLANE ( 'NONE',  #12759 ) ;
#85088 = CARTESIAN_POINT ( 'NONE',  ( -124.6228709571501412, -24.35013146730204525, 9.818937971375104823 ) ) ;
#85089 = EDGE_CURVE ( 'NONE', #10184, #17176, #75939, .T. ) ;
#85090 = CARTESIAN_POINT ( 'NONE',  ( -21.10450430117995424, 9.351148110661185342, 11.49999999999999645 ) ) ;
#85091 = CARTESIAN_POINT ( 'NONE',  ( 22.73759373355791169, -1.750760473330008171, 11.49999999999998934 ) ) ;
#85092 = CARTESIAN_POINT ( 'NONE',  ( 4.639502537026700679, -5.876774720514415407, 19.60647575951318800 ) ) ;
#85093 = CARTESIAN_POINT ( 'NONE',  ( -67.52287095715004739, -24.51283580621365132, 0.6167428607019708187 ) ) ;
#85094 = CARTESIAN_POINT ( 'NONE',  ( -85.62287095715004170, -24.99156045073393173, 7.747789690856161648 ) ) ;
#85095 = CIRCLE ( 'NONE', #78570, 4.080000000000000071 ) ;
#85096 = CARTESIAN_POINT ( 'NONE',  ( -22.05133119090760019, 4.102169094691678453, 11.49999999999999645 ) ) ;
#85097 = ORIENTED_EDGE ( 'NONE', *, *, #31061, .T. ) ;
#85098 = B_SPLINE_CURVE_WITH_KNOTS ( 'NONE', 3,
 ( #51935, #89990, #5748, #12852, #67172, #59551, #97105, #50941 ),
 .UNSPECIFIED., .F., .F.,
 ( 4, 2, 2, 4 ),
 ( 6.384118678604512793E-06, 0.002007151183507257554, 0.003007534715921582509, 0.004007918248335906597 ),
 .UNSPECIFIED. ) ;
#85099 = LINE ( 'NONE', #85597, #31409 ) ;
#85100 = CARTESIAN_POINT ( 'NONE',  ( -38.62287095715004881, -24.50321055353804311, 9.387540953477525818 ) ) ;
#85101 = ADVANCED_FACE ( 'NONE', ( #27783 ), #29777, .T. ) ;
#85102 = CARTESIAN_POINT ( 'NONE',  ( 9.922928194174257754, 19.57116106031148561, 11.49999999999998934 ) ) ;
#85103 = CARTESIAN_POINT ( 'NONE',  ( -5.366453405989236813, 0.000000000000000000, 21.89999999999999858 ) ) ;
#85104 = CARTESIAN_POINT ( 'NONE',  ( -87.63200167382973405, -24.15620529776628445, 10.23563542870660292 ) ) ;
#85105 = CARTESIAN_POINT ( 'NONE',  ( -38.62287095715005592, -29.50250786944525672, 11.44777988621624232 ) ) ;
#85106 = LINE ( 'NONE', #77482, #33014 ) ;
#85107 = DIRECTION ( 'NONE',  ( 0.000000000000000000, 0.000000000000000000, 1.000000000000000000 ) ) ;
#85108 = VERTEX_POINT ( 'NONE', #20162 ) ;
#85109 = CARTESIAN_POINT ( 'NONE',  ( 5.889875310795558150, 19.62242631308348706, 11.49999999999998934 ) ) ;
#85110 = VERTEX_POINT ( 'NONE', #51124 ) ;
#85111 = EDGE_LOOP ( 'NONE', ( #46988, #9745, #92096, #51598 ) ) ;
#85112 = EDGE_LOOP ( 'NONE', ( #40361, #12724, #35612, #39443 ) ) ;
#85113 = ORIENTED_EDGE ( 'NONE', *, *, #69722, .T. ) ;
#85114 = CARTESIAN_POINT ( 'NONE',  ( 7.103900956763240515, -21.94381868531750968, -1.500000000000002220 ) ) ;
#85115 = DIRECTION ( 'NONE',  ( 0.000000000000000000, 0.000000000000000000, -1.000000000000000000 ) ) ;
#85116 = CARTESIAN_POINT ( 'NONE',  ( 14.62039552936377085, -14.08751720214925207, -1.500000000000002220 ) ) ;
#85117 = VERTEX_POINT ( 'NONE', #74455 ) ;
#85118 = CARTESIAN_POINT ( 'NONE',  ( -27.14006706031606697, -25.03993259027813778, 4.938174481708933250 ) ) ;
#85119 = DIRECTION ( 'NONE',  ( -0.000000000000000000, -1.000000000000000000, -0.000000000000000000 ) ) ;
#85120 = B_SPLINE_CURVE_WITH_KNOTS ( 'NONE', 3,
 ( #48993, #41374, #72326, #89543, #50992, #4810 ),
 .UNSPECIFIED., .F., .F.,
 ( 4, 2, 4 ),
 ( 0.000000000000000000, 0.001380901958385390930, 0.002761803916770781860 ),
 .UNSPECIFIED. ) ;
#85121 = CARTESIAN_POINT ( 'NONE',  ( -28.52287095715006160, -23.56429130584908194, 11.05761041701457792 ) ) ;
#85122 = CARTESIAN_POINT ( 'NONE',  ( -70.62753759711341672, -24.83618233451450052, 1.606449574219541487 ) ) ;
#85124 = ORIENTED_EDGE ( 'NONE', *, *, #77143, .T. ) ;
#85123 = CARTESIAN_POINT ( 'NONE',  ( 20.53733210929814845, -6.371126427052321795, 11.49999999999999645 ) ) ;
#85125 = CARTESIAN_POINT ( 'NONE',  ( -75.58253337940892891, -24.83618233451450763, 1.606449574219540599 ) ) ;
#85126 = CARTESIAN_POINT ( 'NONE',  ( -61.62756372973229446, -24.51419770103157347, 9.386484678747178734 ) ) ;
#85127 = ORIENTED_EDGE ( 'NONE', *, *, #60505, .T. ) ;
#85128 = CARTESIAN_POINT ( 'NONE',  ( 20.29938135082171158, -4.300543036493735372, 11.49999999999998934 ) ) ;
#85129 = AXIS2_PLACEMENT_3D ( 'NONE', #1505, #77101, #86724 ) ;
#85130 = VERTEX_POINT ( 'NONE', #4949 ) ;
#85132 = ORIENTED_EDGE ( 'NONE', *, *, #24438, .F. ) ;
#85131 = CARTESIAN_POINT ( 'NONE',  ( -10.34999999999999254, 3.851859888774471706E-31, 4.499999999999999112 ) ) ;
#85133 = CARTESIAN_POINT ( 'NONE',  ( -111.5539194383848098, -24.15620529776629510, 10.23563542870659582 ) ) ;
#85134 = DIRECTION ( 'NONE',  ( 1.000000000000000000, 3.773278334444167608E-23, 8.201307833595939069E-29 ) ) ;
#85135 = ORIENTED_EDGE ( 'NONE', *, *, #1726, .F. ) ;
#85136 = ORIENTED_EDGE ( 'NONE', *, *, #39215, .F. ) ;
#85137 = CARTESIAN_POINT ( 'NONE',  ( 4.642799911345256270, -5.876774720514406525, 18.59646607068888713 ) ) ;
#85138 = CARTESIAN_POINT ( 'NONE',  ( -111.6228709571500559, -29.50248528299804818, 1.056150453629043584 ) ) ;
#85139 = CARTESIAN_POINT ( 'NONE',  ( -65.62561733370567651, -24.92564183028979130, 1.928384488918254869 ) ) ;
#85140 = CARTESIAN_POINT ( 'NONE',  ( 17.71009474140864981, 13.04663522181963309, 11.49999999999999645 ) ) ;
#85141 = AXIS2_PLACEMENT_3D ( 'NONE', #68303, #45970, #92127 ) ;
#85142 = CARTESIAN_POINT ( 'NONE',  ( 6.044871794871792048, -6.376774720514401196, 18.16025641025640880 ) ) ;
#85143 = CARTESIAN_POINT ( 'NONE',  ( -3.649967738973055376, -22.27025559232234642, -1.500000000000002220 ) ) ;
#85144 = CIRCLE ( 'NONE', #55979, 0.3000000000000016542 ) ;
#85145 = CARTESIAN_POINT ( 'NONE',  ( -20.70934228997045068, 3.328930095467914185, -1.500000000000002220 ) ) ;
#85146 = CARTESIAN_POINT ( 'NONE',  ( -20.77875734969026311, -6.143225279485574397, 27.35402280011862430 ) ) ;
#85147 = ORIENTED_EDGE ( 'NONE', *, *, #53378, .F. ) ;
#85148 = ORIENTED_EDGE ( 'NONE', *, *, #34486, .F. ) ;
#85149 = CARTESIAN_POINT ( 'NONE',  ( -80.62287095715002749, -24.51163499207174112, 0.6490370598554275894 ) ) ;
#85150 = PERSON ( 'NAUO-PER13', 'UNSPECIFIED', 'UNSPECIFIED', ('UNSPECIFIED'), ('UNSPECIFIED'), ('UNSPECIFIED') ) ;
#85151 = CARTESIAN_POINT ( 'NONE',  ( -18.46100929034391314, -11.06139713797464985, -1.500000000000002220 ) ) ;
#85152 = CARTESIAN_POINT ( 'NONE',  ( 6.499999999999992895, 0.9999999999999988898, 3.499999999999998668 ) ) ;
#85153 = ORIENTED_EDGE ( 'NONE', *, *, #63658, .T. ) ;
#85154 = CARTESIAN_POINT ( 'NONE',  ( -5.075574613727041218, 20.51645923614106337, -1.500000000000002220 ) ) ;
#85155 = DIRECTION ( 'NONE',  ( -3.773278334453079030E-23, 0.9999999999976377785, 2.173523156925979128E-06 ) ) ;
#85156 = EDGE_CURVE ( 'NONE', #94497, #88045, #36393, .T. ) ;
#85157 = CARTESIAN_POINT ( 'NONE',  ( -61.66031320541097216, -25.33009847151395633, 4.495758292450051208 ) ) ;
#85158 = CARTESIAN_POINT ( 'NONE',  ( -121.5537572759010061, -24.51314013834315375, 0.6176544820404190617 ) ) ;
#85159 = CARTESIAN_POINT ( 'NONE',  ( 3.300000000000004263, 0.000000000000000000, 0.000000000000000000 ) ) ;
#85160 = CARTESIAN_POINT ( 'NONE',  ( -117.6228709571500559, -24.64898659630368627, 1.056161002820833028 ) ) ;
#85161 = CARTESIAN_POINT ( 'NONE',  ( -22.11188964843745453, -1.696007508606716341, -1.500000000000002220 ) ) ;
#85162 = ADVANCED_FACE ( 'NONE', ( #44511 ), #59238, .F. ) ;
#85163 = PLANE ( 'NONE',  #7892 ) ;
#85164 = EDGE_CURVE ( 'NONE', #82652, #15615, #25571, .T. ) ;
#85165 = ORIENTED_EDGE ( 'NONE', *, *, #81187, .T. ) ;
#85166 = CARTESIAN_POINT ( 'NONE',  ( 8.462785143989153269, -5.965225279485592225, -28.02084008811334215 ) ) ;
#85167 = CARTESIAN_POINT ( 'NONE',  ( -37.66608410079602010, -23.48783264082478084, -1.443836473390075703 ) ) ;
#85168 = CARTESIAN_POINT ( 'NONE',  ( -40.49165087243459737, -25.30353303947430987, 5.543942858925161588 ) ) ;
#85169 = ADVANCED_FACE ( 'NONE', ( #52125 ), #12030, .T. ) ;
#85170 = DIRECTION ( 'NONE',  ( 1.000000000000000000, -0.000000000000000000, 2.417950247244706201E-16 ) ) ;
#85171 = CARTESIAN_POINT ( 'NONE',  ( 6.499999999999992895, -5.174132726397565334E-16, -2.500000000000001332 ) ) ;
#85172 = CARTESIAN_POINT ( 'NONE',  ( -14.69715086760845857, -12.76062437926726290, 11.49999999999998934 ) ) ;
#85173 = AXIS2_PLACEMENT_3D ( 'NONE', #58036, #50911, #65162 ) ;
#85174 = CARTESIAN_POINT ( 'NONE',  ( -6.079122355442096115, 20.50309271558274915, -1.500000000000002220 ) ) ;
#85175 = CARTESIAN_POINT ( 'NONE',  ( -62.55964909848019317, -23.73766607897669445, -1.055555164236454901 ) ) ;
#85176 = LINE ( 'NONE', #15664, #51248 ) ;
#85177 = CARTESIAN_POINT ( 'NONE',  ( -106.6228709571500559, -24.65952944569304606, 1.056160979905703012 ) ) ;
#85178 = CARTESIAN_POINT ( 'NONE',  ( -109.8650282762807393, -25.28040082146351608, 5.784628005357986602 ) ) ;
#85179 = B_SPLINE_CURVE_WITH_KNOTS ( 'NONE', 3,
 ( #78527, #924, #46606, #55727, #77031, #69929 ),
 .UNSPECIFIED., .F., .F.,
 ( 4, 2, 4 ),
 ( 0.000000000000000000, 0.001380901958385383124, 0.002761803916770766247 ),
 .UNSPECIFIED. ) ;
#85180 = CARTESIAN_POINT ( 'NONE',  ( -7.311831771877058905, -21.45741656709679646, -1.500000000000002220 ) ) ;
#85181 = ADVANCED_FACE ( 'NONE', ( #53633 ), #100257, .F. ) ;
#85182 = DIRECTION ( 'NONE',  ( 3.773278334444167608E-23, -1.000000000000000000, 0.000000000000000000 ) ) ;
#85183 = CARTESIAN_POINT ( 'NONE',  ( -127.6228709571500559, -24.34917612406838572, 0.1852690917426747241 ) ) ;
#85184 = CARTESIAN_POINT ( 'NONE',  ( 2.793900936927258272, 19.68708943014846469, 11.49999999999999645 ) ) ;
#85185 = CARTESIAN_POINT ( 'NONE',  ( -69.52287095715011844, -23.73907113216989018, -1.053371485793251239 ) ) ;
#85186 = CARTESIAN_POINT ( 'NONE',  ( -73.62287095715004170, -24.50216790748098461, 0.6166512839513668132 ) ) ;
#85187 = EDGE_LOOP ( 'NONE', ( #12119, #86657, #1996, #1413 ) ) ;
#85188 = CARTESIAN_POINT ( 'NONE',  ( -60.52287095715004028, -24.92579138211018730, 1.929029949965656909 ) ) ;
#85189 = DIRECTION ( 'NONE',  ( -0.000000000000000000, 2.173523156925979552E-06, -0.9999999999976378895 ) ) ;
#85190 = CARTESIAN_POINT ( 'NONE',  ( -68.52287095715009002, -24.51283580621364422, 0.6167428607019779241 ) ) ;
#85191 = CARTESIAN_POINT ( 'NONE',  ( 16.53012286974688294, -13.99140274789385252, 11.49999999999998934 ) ) ;
#85192 = CARTESIAN_POINT ( 'NONE',  ( -124.6228709571500559, -24.64898659630368627, 1.056161002820833028 ) ) ;
#85193 = CARTESIAN_POINT ( 'NONE',  ( 15.33136405852079243, -11.96835230219363311, -1.500000000000002220 ) ) ;
#85194 = DIRECTION ( 'NONE',  ( 0.000000000000000000, 0.000000000000000000, -1.000000000000000000 ) ) ;
#85195 = DIRECTION ( 'NONE',  ( -3.773278334453080206E-23, 0.9999999999976377785, 2.173523156925979975E-06 ) ) ;
#85196 = CARTESIAN_POINT ( 'NONE',  ( 19.41305359857673096, 4.112862643401165919, 11.49999999999998934 ) ) ;
#85197 = ORIENTED_EDGE ( 'NONE', *, *, #41552, .T. ) ;
#85198 = CARTESIAN_POINT ( 'NONE',  ( 18.82434097252966154, -7.598309640217090433, 11.49999999999999645 ) ) ;
#85199 = LINE ( 'NONE', #38029, #24547 ) ;
#85200 = VECTOR ( 'NONE', #79364, 1000.000000000000000 ) ;
#85201 = CARTESIAN_POINT ( 'NONE',  ( -1.044871794871790938, -6.376774720514427841, 21.75000000000000355 ) ) ;
#85202 = EDGE_LOOP ( 'NONE', ( #22729, #93005, #93142, #66064 ) ) ;
#85203 = DIRECTION ( 'NONE',  ( -3.773278334453079030E-23, 0.9999999999976377785, 2.173523156925978705E-06 ) ) ;
#85204 = CARTESIAN_POINT ( 'NONE',  ( -114.5228709571500616, -29.50248528299804818, 1.056150453629043584 ) ) ;
#85205 = CARTESIAN_POINT ( 'NONE',  ( -49.63502199369077772, -25.31601829474233156, 4.997541875046982440 ) ) ;
#85206 = AXIS2_PLACEMENT_3D ( 'NONE', #1927, #48102, #65351 ) ;
#85207 = CARTESIAN_POINT ( 'NONE',  ( -40.62513804936914852, -23.48786465467240347, 11.44779295918255180 ) ) ;
#85208 = VECTOR ( 'NONE', #26665, 1000.000000000000000 ) ;
#85209 = CARTESIAN_POINT ( 'NONE',  ( -59.62287095715004881, -29.50250786944525672, 11.44777988621623876 ) ) ;
#85210 = CARTESIAN_POINT ( 'NONE',  ( 16.71511084712224360, -11.16500066668146829, -1.500000000000002220 ) ) ;
#85211 = VECTOR ( 'NONE', #17920, 1000.000000000000114 ) ;
#85212 = CARTESIAN_POINT ( 'NONE',  ( -89.52287095715009002, -24.66019654487200441, 8.947790411086119278 ) ) ;
#85213 = EDGE_LOOP ( 'NONE', ( #13596, #46579, #82581, #67406 ) ) ;
#85214 = CARTESIAN_POINT ( 'NONE',  ( 8.499999999999989342, 18.99999999999977973, 2.100000000000000089 ) ) ;
#85215 = CIRCLE ( 'NONE', #10622, 2.249999999999998668 ) ;
#85216 = ADVANCED_FACE ( 'NONE', ( #61246 ), #15041, .F. ) ;
#85217 = CARTESIAN_POINT ( 'NONE',  ( 21.75204538223844963, -7.182240389990739438, 11.49999999999999645 ) ) ;
#85218 = CARTESIAN_POINT ( 'NONE',  ( -0.6305239314742796530, -22.70799625201654592, -1.500000000000002220 ) ) ;
#85219 = VERTEX_POINT ( 'NONE', #31778 ) ;
#85220 = DIRECTION ( 'NONE',  ( 0.000000000000000000, 0.000000000000000000, -1.000000000000000000 ) ) ;
#85221 = CARTESIAN_POINT ( 'NONE',  ( -126.5228709571500900, -24.35013146730205236, 9.818937971375095941 ) ) ;
#85222 = DIRECTION ( 'NONE',  ( -3.773278334453079618E-23, 0.9999999999976377785, 2.173523156925979975E-06 ) ) ;
#85223 = CARTESIAN_POINT ( 'NONE',  ( -36.52287095715006870, -29.50250243563736774, 8.947779886222148704 ) ) ;
#85224 = ADVANCED_FACE ( 'NONE', ( #826 ), #85557, .T. ) ;
#85225 = CARTESIAN_POINT ( 'NONE',  ( -128.5896661346126564, -24.35071581493544102, 9.817618358456018157 ) ) ;
#85226 = CARTESIAN_POINT ( 'NONE',  ( 8.499999999999989342, 19.99999999999999289, 2.100000000000000089 ) ) ;
#85227 = ORIENTED_EDGE ( 'NONE', *, *, #93457, .F. ) ;
#85228 = CARTESIAN_POINT ( 'NONE',  ( -6.692510123977180925, 19.25193956699996178, 11.49999999999998934 ) ) ;
#85229 = ORIENTED_EDGE ( 'NONE', *, *, #12659, .F. ) ;
#85230 = CARTESIAN_POINT ( 'NONE',  ( -22.87025945403008365, 2.249016246415321163, 11.49999999999998934 ) ) ;
#85231 = CARTESIAN_POINT ( 'NONE',  ( -54.56007923198101395, -23.73791477778911485, 11.05961554403171121 ) ) ;
#85232 = EDGE_LOOP ( 'NONE', ( #30379, #20019, #28696, #1926, #18649, #45106 ) ) ;
#85233 = PLANE ( 'NONE',  #2369 ) ;
#85234 = CARTESIAN_POINT ( 'NONE',  ( -81.46833269854555226, -25.24078552941144693, 6.350783917184607219 ) ) ;
#85235 = CARTESIAN_POINT ( 'NONE',  ( 11.98973536156539943, 4.132774720514426292, -26.26140391504922178 ) ) ;
#85237 = VERTEX_POINT ( 'NONE', #68844 ) ;
#85236 = CARTESIAN_POINT ( 'NONE',  ( -4.607724273132460802, 20.83226218841027944, 11.49999999999999645 ) ) ;
#85238 = ORIENTED_EDGE ( 'NONE', *, *, #90665, .F. ) ;
#85239 = CARTESIAN_POINT ( 'NONE',  ( 4.265775719338400052, 21.77767432286298543, -1.500000000000002220 ) ) ;
#85240 = CARTESIAN_POINT ( 'NONE',  ( -1.706377481887368486, -20.59057665607738130, 11.49999999999998934 ) ) ;
#85241 = ORIENTED_EDGE ( 'NONE', *, *, #40753, .F. ) ;
#85242 = ORIENTED_EDGE ( 'NONE', *, *, #54639, .F. ) ;
#85243 = FACE_OUTER_BOUND ( 'NONE', #91878, .T. ) ;
#85244 = DIRECTION ( 'NONE',  ( 0.000000000000000000, -1.000000000000000000, 0.000000000000000000 ) ) ;
#85245 = VERTEX_POINT ( 'NONE', #46013 ) ;
#85246 = DIRECTION ( 'NONE',  ( 0.7071067811865507924, 0.000000000000000000, 0.7071067811865442421 ) ) ;
#85247 = ORIENTED_EDGE ( 'NONE', *, *, #63336, .F. ) ;
#85248 = CARTESIAN_POINT ( 'NONE',  ( -56.55620429048339304, -24.64965694238574301, 8.947790433994201820 ) ) ;
#85249 = DIRECTION ( 'NONE',  ( -3.773278334453079030E-23, 0.9999999999976377785, 2.173523156925979128E-06 ) ) ;
#85250 = CARTESIAN_POINT ( 'NONE',  ( 7.312689604342500260, -19.48077458720139532, -1.500000000000002220 ) ) ;
#85251 = CARTESIAN_POINT ( 'NONE',  ( 20.57308398666954119, -7.222494929537193187, 11.49999999999999645 ) ) ;
#85252 = B_SPLINE_CURVE_WITH_KNOTS ( 'NONE', 3,
 ( #87421, #48877, #57498, #79804, #80818, #55995, #1701, #11301, #10301, #33136 ),
 .UNSPECIFIED., .F., .F.,
 ( 4, 2, 2, 2, 4 ),
 ( 0.000000000000000000, 0.0004823517777971119314, 0.0009647035555942238627, 0.001447055333391335848, 0.001929407111188447725 ),
 .UNSPECIFIED. ) ;
#85253 = CARTESIAN_POINT ( 'NONE',  ( 25.53174711415574194, -4.590565211979967586, -10.98894470817409363 ) ) ;
#85254 = CARTESIAN_POINT ( 'NONE',  ( -78.56385301586374226, -23.48786465467241058, 11.44779295918254469 ) ) ;
#85255 = CARTESIAN_POINT ( 'NONE',  ( -19.72384299526936857, -10.77339039931002773, -1.500000000000002220 ) ) ;
#85256 = AXIS2_PLACEMENT_3D ( 'NONE', #61375, #32415, #76565 ) ;
#85257 = CARTESIAN_POINT ( 'NONE',  ( -38.60881210526748220, -23.73766607897670511, -1.055555164236442689 ) ) ;
#85258 = FACE_OUTER_BOUND ( 'NONE', #50838, .T. ) ;
#85259 = CARTESIAN_POINT ( 'NONE',  ( 4.736659488006659480, -5.876774720514420736, 21.25082490164487581 ) ) ;
#85260 = ORIENTED_EDGE ( 'NONE', *, *, #31526, .T. ) ;
#85261 = ORIENTED_EDGE ( 'NONE', *, *, #13103, .F. ) ;
#85262 = ORIENTED_EDGE ( 'NONE', *, *, #80510, .F. ) ;
#85263 = AXIS2_PLACEMENT_3D ( 'NONE', #25322, #17209, #71011 ) ;
#85264 = CARTESIAN_POINT ( 'NONE',  ( -9.778911232092227124, -18.99720643767551209, -1.500000000000002220 ) ) ;
#85265 = VERTEX_POINT ( 'NONE', #7430 ) ;
#85266 = VECTOR ( 'NONE', #34583, 1000.000000000000114 ) ;
#85267 = CARTESIAN_POINT ( 'NONE',  ( -15.31302551872622075, -14.39686070098267479, -1.500000000000002220 ) ) ;
#85268 = CARTESIAN_POINT ( 'NONE',  ( -30.61626898804283670, -24.27850102686685929, 0.04395666736089842014 ) ) ;
#85269 = EDGE_CURVE ( 'NONE', #20866, #65831, #63352, .T. ) ;
#85270 = CARTESIAN_POINT ( 'NONE',  ( -99.56303788721014314, -25.24522941805722098, 3.791487066088053748 ) ) ;
#85271 = VECTOR ( 'NONE', #68926, 1000.000000000000114 ) ;
#85272 = CARTESIAN_POINT ( 'NONE',  ( 2.911360383046243783, -6.376774720514417183, 20.24673073119071276 ) ) ;
#85273 = CARTESIAN_POINT ( 'NONE',  ( -6.887433846447126307, -20.85920400149894149, -1.500000000000002220 ) ) ;
#85274 = CARTESIAN_POINT ( 'NONE',  ( 22.81105451610979173, 6.475225279485573360, -17.31691820600746823 ) ) ;
#85275 = VERTEX_POINT ( 'NONE', #77928 ) ;
#85276 = CARTESIAN_POINT ( 'NONE',  ( 0.5999240985075874333, 1.411520799013914917, 8.999999999999987566 ) ) ;
#85277 = AXIS2_PLACEMENT_3D ( 'NONE', #69590, #67599, #98518 ) ;
#85278 = ADVANCED_FACE ( 'NONE', ( #24158 ), #47008, .T. ) ;
#85279 = FACE_OUTER_BOUND ( 'NONE', #62968, .T. ) ;
#85280 = CARTESIAN_POINT ( 'NONE',  ( -19.40664508603899563, 7.695215611089875729, 11.49999999999999645 ) ) ;
#85281 = AXIS2_PLACEMENT_3D ( 'NONE', #40555, #50659, #42561 ) ;
#85282 = EDGE_CURVE ( 'NONE', #57581, #58432, #41597, .T. ) ;
#85283 = CARTESIAN_POINT ( 'NONE',  ( 31.63284457977613684, -3.861502214243257125, 27.22238481897691287 ) ) ;
#85284 = EDGE_CURVE ( 'NONE', #14950, #11637, #70698, .T. ) ;
#85285 = CARTESIAN_POINT ( 'NONE',  ( -125.5228709571500616, -24.99156044556120904, 7.747789690856173195 ) ) ;
#85286 = CARTESIAN_POINT ( 'NONE',  ( -10.19904512095640037, -23.73149035699961473, 5.002395802403317049 ) ) ;
#85287 = CARTESIAN_POINT ( 'NONE',  ( -3.120219904758775975, 21.05623772282662998, -1.500000000000002220 ) ) ;
#85288 = CARTESIAN_POINT ( 'NONE',  ( -104.5228709571500758, -23.48786465467241769, 11.44779295918254114 ) ) ;
#85289 = ADVANCED_FACE ( 'NONE', ( #32275 ), #70847, .F. ) ;
#85290 = CARTESIAN_POINT ( 'NONE',  ( -107.6248333959935053, -24.51419770103157703, 9.386484678747169852 ) ) ;
#85291 = CARTESIAN_POINT ( 'NONE',  ( -122.5228709571500616, -24.65952944569305316, 1.056160979905705899 ) ) ;
#85292 = CARTESIAN_POINT ( 'NONE',  ( -5.314757719055156038, -5.876774720514411854, 19.55912026249540858 ) ) ;
#85293 = CARTESIAN_POINT ( 'NONE',  ( -18.84819291449097278, 12.34854029719970825, -1.500000000000002220 ) ) ;
#85294 = CARTESIAN_POINT ( 'NONE',  ( -118.6228709571500701, -23.48786465467241769, 11.44779295918253759 ) ) ;
#85295 = VERTEX_POINT ( 'NONE', #63244 ) ;
#85296 = DIRECTION ( 'NONE',  ( 3.469446951953614189E-15, -1.000000000000000000, 0.000000000000000000 ) ) ;
#85297 = CARTESIAN_POINT ( 'NONE',  ( -19.44079195400435012, 3.002763184081948200, 11.49999999999999645 ) ) ;
#85298 = DIRECTION ( 'NONE',  ( 0.06486421869277853025, 0.000000000000000000, -0.9978940991575085961 ) ) ;
#85299 = PLANE ( 'NONE',  #78742 ) ;
#85300 = EDGE_CURVE ( 'NONE', #78143, #76987, #6938, .T. ) ;
#85301 = VERTEX_POINT ( 'NONE', #46504 ) ;
#85302 = CARTESIAN_POINT ( 'NONE',  ( -89.52287095715007581, -23.72773821059536203, 11.05748984161097326 ) ) ;
#85303 = LINE ( 'NONE', #6680, #1043 ) ;
#85304 = CARTESIAN_POINT ( 'NONE',  ( -99.94284412489217573, -25.25095800927872958, 5.308582836096728208 ) ) ;
#85305 = VECTOR ( 'NONE', #6001, 1000.000000000000114 ) ;
#85306 = CARTESIAN_POINT ( 'NONE',  ( 2.412641546452875208, 19.58572291230954221, -1.500000000000002220 ) ) ;
#85307 = ORIENTED_EDGE ( 'NONE', *, *, #65751, .T. ) ;
#85308 = CARTESIAN_POINT ( 'NONE',  ( 9.146648804565860047, 6.376774720514172934, -28.07004961687618660 ) ) ;
#85309 = MECHANICAL_CONTEXT ( 'NONE', #49246, 'mechanical' ) ;
#85310 = ORIENTED_EDGE ( 'NONE', *, *, #15294, .F. ) ;
#85311 = FACE_OUTER_BOUND ( 'NONE', #34093, .T. ) ;
#85312 = FACE_OUTER_BOUND ( 'NONE', #22815, .T. ) ;
#85313 = CARTESIAN_POINT ( 'NONE',  ( -55.57730862517797732, -24.92564183028978775, 1.928384488918253092 ) ) ;
#85314 = LINE ( 'NONE', #7698, #31461 ) ;
#85315 = PLANE ( 'NONE',  #79271 ) ;
#85316 = LINE ( 'NONE', #96444, #18170 ) ;
#85317 = CARTESIAN_POINT ( 'NONE',  ( -113.6228709571500559, -29.50250243563736774, 8.947779886222136270 ) ) ;
#85318 = CARTESIAN_POINT ( 'NONE',  ( 10.17626895549074817, -17.22257424524772418, -1.500000000000002220 ) ) ;
#85319 = EDGE_CURVE ( 'NONE', #100298, #96024, #29530, .T. ) ;
#85320 = DIRECTION ( 'NONE',  ( 0.000000000000000000, 0.9999999999976377785, 2.173523156925979128E-06 ) ) ;
#85321 = CARTESIAN_POINT ( 'NONE',  ( -45.64357623215011728, -24.40133493613049964, 9.663955038902802386 ) ) ;
#85322 = ORIENTED_EDGE ( 'NONE', *, *, #23881, .F. ) ;
#85323 = AXIS2_PLACEMENT_3D ( 'NONE', #13175, #98410, #59882 ) ;
#85324 = ADVANCED_FACE ( 'NONE', ( #54130 ), #95681, .F. ) ;
#85325 = LINE ( 'NONE', #24431, #53483 ) ;
#85326 = CARTESIAN_POINT ( 'NONE',  ( -109.3965479632025080, -25.29012866004314830, 3.940679847089471277 ) ) ;
#85327 = CARTESIAN_POINT ( 'NONE',  ( -58.52287095715006870, -23.96177878511308990, 10.65340807706330217 ) ) ;
#85328 = CARTESIAN_POINT ( 'NONE',  ( -106.5562042904833930, -23.48786465467241769, 11.44779295918252870 ) ) ;
#85329 = CARTESIAN_POINT ( 'NONE',  ( -119.2834313257731935, -25.38352531986205207, 4.245363004327347589 ) ) ;
#85330 = CARTESIAN_POINT ( 'NONE',  ( -83.59183548183668222, -24.15543982623906771, -0.2315651400026649265 ) ) ;
#85331 = AXIS2_PLACEMENT_3D ( 'NONE', #66542, #80737, #26945 ) ;
#85332 = FACE_OUTER_BOUND ( 'NONE', #34095, .T. ) ;
#85333 = EDGE_CURVE ( 'NONE', #43203, #71288, #73048, .T. ) ;
#85335 = VECTOR ( 'NONE', #20974, 1000.000000000000000 ) ;
#85334 = CARTESIAN_POINT ( 'NONE',  ( -40.52287095715007581, -24.82576562948890597, 8.398263436605414967 ) ) ;
#85336 = ORIENTED_EDGE ( 'NONE', *, *, #32290, .T. ) ;
#85337 = VECTOR ( 'NONE', #76884, 1000.000000000000000 ) ;
#85338 = CARTESIAN_POINT ( 'NONE',  ( 11.01437679584920026, 17.03896688766576517, -1.500000000000002220 ) ) ;
#85339 = EDGE_CURVE ( 'NONE', #881, #25949, #65263, .T. ) ;
#85340 = CARTESIAN_POINT ( 'NONE',  ( 29.57907552664497786, 3.519868637853082571, 29.21818156430573765 ) ) ;
#85341 = AXIS2_PLACEMENT_3D ( 'NONE', #33414, #18197, #97319 ) ;
#85342 = DIRECTION ( 'NONE',  ( 0.000000000000000000, 2.173523156925980399E-06, -0.9999999999976378895 ) ) ;
#85343 = EDGE_LOOP ( 'NONE', ( #31683, #75315, #19849, #3050 ) ) ;
#85344 = CARTESIAN_POINT ( 'NONE',  ( -86.52287095715006160, -24.66019654487199375, 8.947790411086119278 ) ) ;
#85345 = CARTESIAN_POINT ( 'NONE',  ( -11.83016301840747175, -16.26703346747452983, -1.500000000000002220 ) ) ;
#85346 = CARTESIAN_POINT ( 'NONE',  ( -16.48755246578841849, -13.11705038010048163, 11.49999999999999645 ) ) ;
#85347 = CARTESIAN_POINT ( 'NONE',  ( -7.320055889550622474, -20.87099576385019972, 11.49999999999998934 ) ) ;
#85349 = CARTESIAN_POINT ( 'NONE',  ( -20.41219973434085944, 2.133827299322149429, -1.500000000000002220 ) ) ;
#85348 = APPROVAL ( #26036, 'UNSPECIFIED' ) ;
#85350 = B_SPLINE_CURVE_WITH_KNOTS ( 'NONE', 3,
 ( #3412, #88635, #90124, #19106, #50077, #27729, #89626, #81018, #27235, #42965, #73901, #45460, #13983, #21590, #60687, #91114, #98724, #67805, #22576 ),
 .UNSPECIFIED., .F., .F.,
 ( 4, 1, 1, 1, 1, 1, 1, 1, 1, 1, 1, 1, 1, 1, 1, 1, 4 ),
 ( 0.000000000000000000, 0.08252970382206505084, 0.1587788549175693509, 0.2277380621151788020, 0.2899456527966750574, 0.3454988386981356352, 0.3938963373401225820, 0.4363737851900879039, 0.4721222744615228839, 0.5363836155048278265, 0.5990779017254967975, 0.6619482340244574603, 0.7263105423531552862, 0.7917711030502098124, 0.8586473037978579192, 0.9273053338076842067, 1.000000000000000000 ),
 .UNSPECIFIED. ) ;
#85351 = CARTESIAN_POINT ( 'NONE',  ( -60.49713738156505372, -24.40034930558990922, 0.3402023900116026289 ) ) ;
#85352 = ORIENTED_EDGE ( 'NONE', *, *, #70852, .F. ) ;
#85353 = DIRECTION ( 'NONE',  ( 1.286817348990133408E-16, 0.000000000000000000, -1.000000000000000000 ) ) ;
#85354 = VERTEX_POINT ( 'NONE', #96186 ) ;
#85355 = CARTESIAN_POINT ( 'NONE',  ( -5.850750514176234596, -6.376774720514411854, 19.74039977944280366 ) ) ;
#85356 = CARTESIAN_POINT ( 'NONE',  ( -102.5228709571500758, -23.47596703998600631, 11.44779298504228215 ) ) ;
#85357 = ORIENTED_EDGE ( 'NONE', *, *, #32238, .T. ) ;
#85358 = ORIENTED_EDGE ( 'NONE', *, *, #5388, .F. ) ;
#85359 = ORIENTED_EDGE ( 'NONE', *, *, #65447, .F. ) ;
#85360 = CARTESIAN_POINT ( 'NONE',  ( -117.2228709571500644, -23.47593901973090524, -1.443836447538996426 ) ) ;
#85361 = CARTESIAN_POINT ( 'NONE',  ( -71.62287095715011276, -23.95044443724992789, 10.65354141964649415 ) ) ;
#85362 = CARTESIAN_POINT ( 'NONE',  ( -68.50125515983249613, -24.35071581493542681, 9.817618358456032368 ) ) ;
#85363 = B_SPLINE_CURVE_WITH_KNOTS ( 'NONE', 3,
 ( #82525, #83518, #50588, #67823, #35371, #36859 ),
 .UNSPECIFIED., .F., .F.,
 ( 4, 2, 4 ),
 ( 0.000000000000000000, 0.001380764517854764966, 0.002761529035709529931 ),
 .UNSPECIFIED. ) ;
#85364 = CARTESIAN_POINT ( 'NONE',  ( -20.24099117049231467, 3.958469829285517161, -1.500000000000002220 ) ) ;
#85365 = CARTESIAN_POINT ( 'NONE',  ( 19.98343133220876666, -8.209121646405339590, 11.49999999999999645 ) ) ;
#85366 = ORIENTED_EDGE ( 'NONE', *, *, #33751, .T. ) ;
#85367 = CARTESIAN_POINT ( 'NONE',  ( -81.58953762381672448, -24.66019654487199020, 8.947790411086137041 ) ) ;
#85368 = CIRCLE ( 'NONE', #7592, 84.48086791635432746 ) ;
#85369 = CARTESIAN_POINT ( 'NONE',  ( 5.251006604497604258, 6.376774720514426953, -25.47015536487705489 ) ) ;
#85370 = CARTESIAN_POINT ( 'NONE',  ( 1.438201247614206757, 22.34484416265529916, -1.500000000000002220 ) ) ;
#85371 = LINE ( 'NONE', #15858, #14025 ) ;
#85372 = DIRECTION ( 'NONE',  ( -3.773278334453079030E-23, 0.9999999999976377785, 2.173523156925979128E-06 ) ) ;
#85373 = ORIENTED_EDGE ( 'NONE', *, *, #76901, .F. ) ;
#85374 = CARTESIAN_POINT ( 'NONE',  ( 33.00535138976593430, -3.570691370340898452, -12.97242311383974744 ) ) ;
#85375 = LINE ( 'NONE', #61565, #57229 ) ;
#85376 = VECTOR ( 'NONE', #37248, 1000.000000000000000 ) ;
#85377 = CARTESIAN_POINT ( 'NONE',  ( -12.66259425867894350, -16.64798919286708667, 11.49999999999998934 ) ) ;
#85378 = ORIENTED_EDGE ( 'NONE', *, *, #34893, .T. ) ;
#85379 = PLANE ( 'NONE',  #32835 ) ;
#85380 = B_SPLINE_CURVE_WITH_KNOTS ( 'NONE', 3,
 ( #12738, #13239, #16251, #45210, #8644, #39589, #77133, #99964, #45705, #78129, #69547, #47210, #525, #30474, #8146, #61440 ),
 .UNSPECIFIED., .F., .F.,
 ( 4, 2, 2, 2, 2, 2, 2, 4 ),
 ( 8.673617379884035472E-19, 0.0002961782169017380213, 0.0005923564338034751752, 0.0008885346507052124376, 0.001184712867606949483, 0.001777069301410424008, 0.002073247518312160836, 0.002369425735213897665 ),
 .UNSPECIFIED. ) ;
#85381 = VERTEX_POINT ( 'NONE', #79447 ) ;
#85382 = PLANE ( 'NONE',  #43889 ) ;
#85383 = CARTESIAN_POINT ( 'NONE',  ( -19.98373207111551508, 7.008865001458166155, -1.500000000000002220 ) ) ;
#85384 = VERTEX_POINT ( 'NONE', #11440 ) ;
#85385 = CARTESIAN_POINT ( 'NONE',  ( -50.57926364954687415, -24.83618233451450408, 1.606449574219538601 ) ) ;
#85386 = CARTESIAN_POINT ( 'NONE',  ( 9.495391690522565042, 19.61495305411445500, -1.500000000000002220 ) ) ;
#85387 = CARTESIAN_POINT ( 'NONE',  ( -60.62287095715004881, -23.47596703998600631, 11.44779298504227505 ) ) ;
#85388 = CARTESIAN_POINT ( 'NONE',  ( -76.56415518045969293, -23.48786465467240703, 11.44779295918254647 ) ) ;
#85389 = CARTESIAN_POINT ( 'NONE',  ( -90.62287095715004170, -29.50249982740957577, 7.747779886224967605 ) ) ;
#85390 = CARTESIAN_POINT ( 'NONE',  ( -1.743439162979827595, 21.76861016152796324, -1.500000000000002220 ) ) ;
#85391 = CARTESIAN_POINT ( 'NONE',  ( 6.403846153846157740, -5.876774720514425177, 21.48076923076922995 ) ) ;
#85392 = ADVANCED_FACE ( 'NONE', ( #57632 ), #64766, .T. ) ;
#85393 = EDGE_LOOP ( 'NONE', ( #34595, #1401, #43300, #97075 ) ) ;
#85394 = CARTESIAN_POINT ( 'NONE',  ( 7.234974673537251100, -5.876774720514416295, 19.99114326857715795 ) ) ;
#85395 = DIRECTION ( 'NONE',  ( -0.000000000000000000, -1.000000000000000000, -0.000000000000000000 ) ) ;
#85396 = ORIENTED_EDGE ( 'NONE', *, *, #20181, .F. ) ;
#85397 = AXIS2_PLACEMENT_3D ( 'NONE', #76569, #34138, #46225 ) ;
#85398 = B_SPLINE_CURVE_WITH_KNOTS ( 'NONE', 3,
 ( #71466, #41011, #79563, #38998, #1954, #942 ),
 .UNSPECIFIED., .F., .F.,
 ( 4, 2, 4 ),
 ( 0.000000000000000000, 0.001380901958385379220, 0.002761803916770758441 ),
 .UNSPECIFIED. ) ;
#85399 = ORIENTED_EDGE ( 'NONE', *, *, #3878, .T. ) ;
#85400 = VERTEX_POINT ( 'NONE', #42419 ) ;
#85401 = EDGE_CURVE ( 'NONE', #13466, #61820, #77859, .T. ) ;
#85402 = CARTESIAN_POINT ( 'NONE',  ( -96.52287095715006160, -24.64965694238575011, 8.947790433994194714 ) ) ;
#85403 = DIRECTION ( 'NONE',  ( -0.000000000000000000, 1.000000000000000000, -0.000000000000000000 ) ) ;
#85404 = CARTESIAN_POINT ( 'NONE',  ( -19.96038302963917488, -7.207760892512529161, -1.500000000000002220 ) ) ;
#85405 = CARTESIAN_POINT ( 'NONE',  ( -94.58862134658387788, -24.34968618360933945, 0.1864209137778861103 ) ) ;
#85406 = EDGE_CURVE ( 'NONE', #94215, #45125, #26165, .T. ) ;
#85407 = CARTESIAN_POINT ( 'NONE',  ( -79.61785653407703478, -25.27791918801320037, 7.314036244604475989 ) ) ;
#85408 = PLANE ( 'NONE',  #80998 ) ;
#85409 = VECTOR ( 'NONE', #94834, 1000.000000000000114 ) ;
#85410 = CARTESIAN_POINT ( 'NONE',  ( -39.04303308397305727, -25.29008967749855685, 4.215216926603018166 ) ) ;
#85411 = CARTESIAN_POINT ( 'NONE',  ( 12.26431755764203047, -15.03328313062362298, 11.49999999999998934 ) ) ;
#85412 = CARTESIAN_POINT ( 'NONE',  ( -51.90526032677228585, -25.28214432996132999, 5.906427834405539201 ) ) ;
#85413 = ORIENTED_EDGE ( 'NONE', *, *, #24203, .T. ) ;
#85414 = CARTESIAN_POINT ( 'NONE',  ( 13.61561175257155298, 13.87280521877887018, 11.49999999999999645 ) ) ;
#85415 = CARTESIAN_POINT ( 'NONE',  ( -26.33488822642538452, -24.89212854592702584, 6.524121854850513991 ) ) ;
#85416 = VECTOR ( 'NONE', #34638, 1000.000000000000000 ) ;
#85417 = CARTESIAN_POINT ( 'NONE',  ( -68.52287095715011844, -24.33832256527049154, 0.1851278514138628983 ) ) ;
#85418 = EDGE_CURVE ( 'NONE', #75788, #77715, #71350, .T. ) ;
#85419 = ORIENTED_EDGE ( 'NONE', *, *, #65393, .F. ) ;
#85420 = CARTESIAN_POINT ( 'NONE',  ( 3.325015365150250535, -5.876774720514403860, 18.26971317031913955 ) ) ;
#85421 = LINE ( 'NONE', #70207, #90319 ) ;
#85422 = CARTESIAN_POINT ( 'NONE',  ( -40.45829750704997707, -25.19502912051678223, 3.293943094755625633 ) ) ;
#85423 = CARTESIAN_POINT ( 'NONE',  ( -93.62357236836618313, -24.66019654487200441, 8.947790411086105067 ) ) ;
#85424 = CARTESIAN_POINT ( 'NONE',  ( -3.719764837209879271, -19.30396570740023421, 11.49999999999998934 ) ) ;
#85425 = DIRECTION ( 'NONE',  ( 0.000000000000000000, -0.000000000000000000, -1.000000000000000000 ) ) ;
#85426 = EDGE_LOOP ( 'NONE', ( #57171, #66829, #39448, #38306 ) ) ;
#85427 = CARTESIAN_POINT ( 'NONE',  ( -21.50746323947805649, 1.722430922125298247, -1.500000000000002220 ) ) ;
#85428 = CARTESIAN_POINT ( 'NONE',  ( -40.59317738058160074, -24.40034930558990922, 0.3402023900116037392 ) ) ;
#85429 = FACE_OUTER_BOUND ( 'NONE', #64537, .T. ) ;
#85430 = CARTESIAN_POINT ( 'NONE',  ( -21.58539018223340022, -8.019882488244659768, -1.500000000000002220 ) ) ;
#85431 = APPROVAL_ROLE ( '' ) ;
#85432 = CARTESIAN_POINT ( 'NONE',  ( -93.58624035233277993, -24.51314013834316086, 0.6176544820404149538 ) ) ;
#85433 = CARTESIAN_POINT ( 'NONE',  ( -90.52287095715009002, -24.14406661686762234, 10.28769366194075019 ) ) ;
#85434 = CARTESIAN_POINT ( 'NONE',  ( -40.01839366089613748, -25.30501058306510487, 5.509688048021296858 ) ) ;
#85435 = DIRECTION ( 'NONE',  ( 0.000000000000000000, 0.000000000000000000, -1.000000000000000000 ) ) ;
#85436 = B_SPLINE_CURVE_WITH_KNOTS ( 'NONE', 3,
 ( #11541, #17157, #71963, #41504, #34389, #88679, #48123, #79052, #1949, #2444, #49131, #80058, #81564, #98764, #66357, #67844, #27279, #74922, #83035 ),
 .UNSPECIFIED., .F., .F.,
 ( 4, 1, 1, 1, 1, 1, 1, 1, 1, 1, 1, 1, 1, 1, 1, 1, 4 ),
 ( 0.000000000000000000, 0.08252970382206502309, 0.1587788549175692676, 0.2277380621151786910, 0.2899456527966748909, 0.3454988386981381332, 0.3938963373401223600, 0.4363737851900878484, 0.4721222744615228284, 0.5363836155048271603, 0.5990779017254961314, 0.6619482340244576823, 0.7263105423531555083, 0.7917711030502102565, 0.8586473037978576972, 0.9273053338076845398, 1.000000000000000000 ),
 .UNSPECIFIED. ) ;
#85437 = CARTESIAN_POINT ( 'NONE',  ( -111.3477393431454487, -25.10921465371560402, 3.253010550120815303 ) ) ;
#85438 = CARTESIAN_POINT ( 'NONE',  ( -98.52287095715004739, -24.50216790748203977, 0.6166512839542589441 ) ) ;
#85439 = CARTESIAN_POINT ( 'NONE',  ( -49.62287095715005592, -23.47593901973091235, -1.443836447539009749 ) ) ;
#85440 = CARTESIAN_POINT ( 'NONE',  ( 19.87125486832220744, 0.9792442318621276121, 11.49999999999998934 ) ) ;
#85441 = DIRECTION ( 'NONE',  ( -1.000000000000000000, -0.000000000000000000, -0.000000000000000000 ) ) ;
#85442 = CARTESIAN_POINT ( 'NONE',  ( 6.388261542594571019, -18.74682169789839392, -1.500000000000002220 ) ) ;
#85443 = VECTOR ( 'NONE', #659, 1000.000000000000000 ) ;
#85444 = FACE_OUTER_BOUND ( 'NONE', #9044, .T. ) ;
#85445 = EDGE_CURVE ( 'NONE', #38147, #79658, #79950, .T. ) ;
#85446 = CARTESIAN_POINT ( 'NONE',  ( -40.43756433397305727, -25.10925592397025241, 2.832404819646103800 ) ) ;
#85447 = CARTESIAN_POINT ( 'NONE',  ( 5.271800844967073907, -3.316774720514426456, -28.56638892015272191 ) ) ;
#85448 = CARTESIAN_POINT ( 'NONE',  ( 1.212613378922696050, -20.72488358683818888, 11.49999999999999645 ) ) ;
#85449 = AXIS2_PLACEMENT_3D ( 'NONE', #6798, #53993, #1203 ) ;
#85450 = CARTESIAN_POINT ( 'NONE',  ( -106.6248962070219335, -24.51314013834316796, 0.6176544820404221703 ) ) ;
#85452 = EDGE_CURVE ( 'NONE', #5224, #94221, #61000, .T. ) ;
#85451 = CARTESIAN_POINT ( 'NONE',  ( 6.015242202445381992, 21.98585358372262633, 11.49999999999999645 ) ) ;
#85453 = ORIENTED_EDGE ( 'NONE', *, *, #11523, .T. ) ;
#85454 = B_SPLINE_SURFACE_WITH_KNOTS ( 'NONE', 3, 3, ( 
 ( #69194, #83920, #14398, #30126 ),
 ( #76294, #61100, #22500, #100112 ),
 ( #1697, #10801, #40748, #86419 ),
 ( #87927, #2204, #18411, #86917 ),
 ( #25524, #78789, #48371, #33133 ),
 ( #64621, #41766, #80814, #17410 ),
 ( #9287, #79300, #64112, #49379 ),
 ( #41256, #9796, #72710, #63608 ),
 ( #95033, #2698, #80311, #56496 ),
 ( #3207, #32630, #34149, #65116 ) ),
 .UNSPECIFIED., .F., .F., .F.,
 ( 4, 3, 3, 4 ),
 ( 4, 4 ),
 ( 0.0004766839783810062465, 0.1491231665100168913, 0.2234464077758348266, 0.2977696490416527619 ),
 ( 0.8495966106698408238, 0.8511156054176940433 ),
 .UNSPECIFIED. ) ;
#85455 = CARTESIAN_POINT ( 'NONE',  ( -69.50161766294181120, -24.34968618360934300, 0.1864209137778826408 ) ) ;
#85456 = CARTESIAN_POINT ( 'NONE',  ( -74.62287095715005592, -24.51387760970724372, 9.387446482453425389 ) ) ;
#85457 = ORIENTED_EDGE ( 'NONE', *, *, #93050, .T. ) ;
#85458 = CARTESIAN_POINT ( 'NONE',  ( -18.82377384687745447, 7.257840063761761051, -1.500000000000002220 ) ) ;
#85459 = CARTESIAN_POINT ( 'NONE',  ( -118.5228709571500758, -29.50250243563736774, 8.947779886222134493 ) ) ;
#85460 = CYLINDRICAL_SURFACE ( 'NONE', #2662, 2.249999999999998668 ) ;
#85461 = EDGE_LOOP ( 'NONE', ( #89863, #57234, #55352, #43346 ) ) ;
#85462 = AXIS2_PLACEMENT_3D ( 'NONE', #47137, #16668, #85182 ) ;
#85463 = ORIENTED_EDGE ( 'NONE', *, *, #60245, .T. ) ;
#85464 = DIRECTION ( 'NONE',  ( -0.000000000000000000, -1.000000000000000000, 0.000000000000000000 ) ) ;
#85465 = CARTESIAN_POINT ( 'NONE',  ( -9.150087108448493822, 20.98025145036519845, -1.500000000000002220 ) ) ;
#85466 = CARTESIAN_POINT ( 'NONE',  ( 13.91401389203221406, 3.316774720514426456, 28.26920385068457264 ) ) ;
#85467 = CARTESIAN_POINT ( 'NONE',  ( 21.64940796807912449, -0.2623997510114038922, -1.500000000000002220 ) ) ;
#85468 = CARTESIAN_POINT ( 'NONE',  ( -36.62287095715004170, -23.47596703998600276, 11.44779298504227505 ) ) ;
#85469 = CARTESIAN_POINT ( 'NONE',  ( -11.44352472427880052, 17.46665840655709090, 11.49999999999999645 ) ) ;
#85470 = EDGE_LOOP ( 'NONE', ( #67914, #45809, #94430, #55731 ) ) ;
#85471 = B_SPLINE_CURVE_WITH_KNOTS ( 'NONE', 3,
 ( #50933, #52425, #73757, #59542 ),
 .UNSPECIFIED., .F., .F.,
 ( 4, 4 ),
 ( 0.000000000000000000, 9.999999999998897304E-05 ),
 .UNSPECIFIED. ) ;
#85472 = CARTESIAN_POINT ( 'NONE',  ( -124.5569027081732827, -23.48783264082477373, -1.443836473390086139 ) ) ;
#85473 = CARTESIAN_POINT ( 'NONE',  ( -12.30081598482267680, 18.28176383447183895, 11.49999999999998934 ) ) ;
#85474 = EDGE_CURVE ( 'NONE', #15615, #82652, #88829, .T. ) ;
#85475 = VECTOR ( 'NONE', #13603, 1000.000000000000000 ) ;
#85476 = PLANE ( 'NONE',  #12251 ) ;
#85477 = CARTESIAN_POINT ( 'NONE',  ( -65.62287095715005592, -24.51254535404254042, 9.355368623467647637 ) ) ;
#85478 = ORIENTED_EDGE ( 'NONE', *, *, #82988, .T. ) ;
#85479 = CARTESIAN_POINT ( 'NONE',  ( -49.56515190845122021, -25.27344855749837294, 3.736414773304981285 ) ) ;
#85480 = DIRECTION ( 'NONE',  ( 1.000000000000000000, -0.000000000000000000, -0.000000000000000000 ) ) ;
#85481 = ORIENTED_EDGE ( 'NONE', *, *, #33075, .T. ) ;
#85482 = LINE ( 'NONE', #6868, #11235 ) ;
#85483 = ORIENTED_EDGE ( 'NONE', *, *, #83955, .T. ) ;
#85484 = VECTOR ( 'NONE', #95529, 1000.000000000000114 ) ;
#85485 = ORIENTED_EDGE ( 'NONE', *, *, #79555, .T. ) ;
#85486 = CARTESIAN_POINT ( 'NONE',  ( 32.50838937279095120, 1.682774720514426114, -10.74666623472941218 ) ) ;
#85487 = CARTESIAN_POINT ( 'NONE',  ( -101.7667076177128678, -25.27404871335912517, 3.940951707345587973 ) ) ;
#85488 = CARTESIAN_POINT ( 'NONE',  ( -4.440151687742864617, -6.376774720514411854, 19.67013632031035897 ) ) ;
#85489 = CARTESIAN_POINT ( 'NONE',  ( -7.951223608505463503, 18.87544906973805325, -1.500000000000002220 ) ) ;
#85490 = ORIENTED_EDGE ( 'NONE', *, *, #66977, .T. ) ;
#85491 = CARTESIAN_POINT ( 'NONE',  ( -27.96875734969026084, -6.143225279485573509, 0.7300228001186309656 ) ) ;
#85492 = EDGE_CURVE ( 'NONE', #10968, #34973, #25664, .T. ) ;
#85493 = CARTESIAN_POINT ( 'NONE',  ( 29.77147767949874435, 4.540774720514427543, 26.15915692125050995 ) ) ;
#85494 = CARTESIAN_POINT ( 'NONE',  ( -45.52287095715006160, -24.99156044556202616, 7.747789690856173195 ) ) ;
#85495 = CARTESIAN_POINT ( 'NONE',  ( -13.27262489239681997, 17.90159134968837051, -1.500000000000002220 ) ) ;
#85496 = EDGE_CURVE ( 'NONE', #17186, #65082, #10946, .T. ) ;
#85497 = CARTESIAN_POINT ( 'NONE',  ( -81.62287095715002749, -23.94994826722515668, -0.6494450866351701990 ) ) ;
#85498 = DIRECTION ( 'NONE',  ( -1.000000000000000000, 0.000000000000000000, 0.000000000000000000 ) ) ;
#85499 = ORIENTED_EDGE ( 'NONE', *, *, #77646, .F. ) ;
#85500 = CARTESIAN_POINT ( 'NONE',  ( 1.000208336950358934, 0.000000000000000000, 2.349999999999999645 ) ) ;
#85501 = DIRECTION ( 'NONE',  ( 0.000000000000000000, 0.000000000000000000, 1.000000000000000000 ) ) ;
#85502 = EDGE_CURVE ( 'NONE', #81363, #18101, #18573, .T. ) ;
#85503 = CARTESIAN_POINT ( 'NONE',  ( -20.82185584224439978, -0.2524610531272265534, 11.49999999999998934 ) ) ;
#85504 = ORIENTED_EDGE ( 'NONE', *, *, #73979, .F. ) ;
#85506 = ORIENTED_EDGE ( 'NONE', *, *, #7163, .F. ) ;
#85505 = CARTESIAN_POINT ( 'NONE',  ( 4.127614219445591814, -6.376774720514408301, 18.60403502951120558 ) ) ;
#85507 = VERTEX_POINT ( 'NONE', #87567 ) ;
#85508 = CARTESIAN_POINT ( 'NONE',  ( -50.85935151307011637, -25.25854555849183924, 7.039179658095172876 ) ) ;
#85509 = CARTESIAN_POINT ( 'NONE',  ( -9.893913718187896222, 18.50344063021147889, -1.500000000000002220 ) ) ;
#85510 = ORIENTED_EDGE ( 'NONE', *, *, #25512, .F. ) ;
#85511 = CARTESIAN_POINT ( 'NONE',  ( -118.5228709571500616, -24.50321055353805377, 9.387540953477511607 ) ) ;
#85512 = DIRECTION ( 'NONE',  ( 0.000000000000000000, 0.9999999999976377785, 2.173523156925979128E-06 ) ) ;
#85513 = CARTESIAN_POINT ( 'NONE',  ( 4.784292611721462585, -5.356774720514426491, -25.54547254883130947 ) ) ;
#85514 = LINE ( 'NONE', #92130, #17770 ) ;
#85515 = CARTESIAN_POINT ( 'NONE',  ( -92.54655063383911795, -24.51419770103157347, 9.386484678747171628 ) ) ;
#85516 = CARTESIAN_POINT ( 'NONE',  ( -63.52287095715006160, -24.64898659630367561, 1.056161002820822592 ) ) ;
#85517 = EDGE_CURVE ( 'NONE', #93507, #40340, #65755, .T. ) ;
#85519 = ORIENTED_EDGE ( 'NONE', *, *, #24937, .F. ) ;
#85518 = CARTESIAN_POINT ( 'NONE',  ( -17.21897301287555848, -14.04741862099043104, 11.49999999999999645 ) ) ;
#85520 = DIRECTION ( 'NONE',  ( -0.000000000000000000, -0.000000000000000000, -1.000000000000000000 ) ) ;
#85521 = CARTESIAN_POINT ( 'NONE',  ( -49.52287095715006160, -29.50250243563736774, 8.947779886222146928 ) ) ;
#85522 = ORIENTED_EDGE ( 'NONE', *, *, #43289, .T. ) ;
#85523 = CARTESIAN_POINT ( 'NONE',  ( -14.80616194778269623, -17.16973004002414882, 11.49999999999998934 ) ) ;
#85524 = VECTOR ( 'NONE', #11148, 1000.000000000000000 ) ;
#85526 = ORIENTED_EDGE ( 'NONE', *, *, #21846, .F. ) ;
#85525 = CARTESIAN_POINT ( 'NONE',  ( -28.60150425279314490, -24.94570498609691001, 7.235193128133280638 ) ) ;
#85527 = VERTEX_POINT ( 'NONE', #10436 ) ;
#85528 = DIRECTION ( 'NONE',  ( 0.000000000000000000, -2.173523156925980399E-06, 0.9999999999976378895 ) ) ;
#85529 = ADVANCED_FACE ( 'NONE', ( #72352 ), #100073, .F. ) ;
#85530 = CARTESIAN_POINT ( 'NONE',  ( 14.76687977769557847, -13.71354340032049457, 11.49999999999998934 ) ) ;
#85531 = EDGE_CURVE ( 'NONE', #42999, #3225, #48519, .T. ) ;
#85532 = CARTESIAN_POINT ( 'NONE',  ( -66.62287095715005592, -24.66019654487199020, 8.947790411086131712 ) ) ;
#85533 = ORIENTED_EDGE ( 'NONE', *, *, #26355, .T. ) ;
#85534 = LINE ( 'NONE', #16018, #19559 ) ;
#85535 = CARTESIAN_POINT ( 'NONE',  ( -18.48265707593502327, -12.51853143457666562, -1.500000000000002220 ) ) ;
#85536 = ADVANCED_FACE ( 'NONE', ( #81949 ), #4340, .T. ) ;
#85537 = ORIENTED_EDGE ( 'NONE', *, *, #24691, .F. ) ;
#85538 = VERTEX_POINT ( 'NONE', #51510 ) ;
#85539 = CARTESIAN_POINT ( 'NONE',  ( -35.52287095715006870, -23.47593901973090169, -1.443836447538997092 ) ) ;
#85540 = CARTESIAN_POINT ( 'NONE',  ( -94.51006116474896146, -24.35071581493543036, 9.817618358456030592 ) ) ;
#85541 = CARTESIAN_POINT ( 'NONE',  ( -54.62287095715004170, -23.47596703998600631, 11.44779298504227505 ) ) ;
#85542 = PLANE ( 'NONE',  #4435 ) ;
#85543 = VECTOR ( 'NONE', #96673, 1000.000000000000114 ) ;
#85544 = EDGE_CURVE ( 'NONE', #25617, #91623, #6321, .T. ) ;
#85545 = CARTESIAN_POINT ( 'NONE',  ( -63.95380932530888884, -23.47593901973090169, -1.443836447538997758 ) ) ;
#85546 = CARTESIAN_POINT ( 'NONE',  ( 17.64699390344983598, -8.409456921668478913, 11.49999999999998934 ) ) ;
#85547 = CARTESIAN_POINT ( 'NONE',  ( 8.500000000000000000, -0.9000000000000000222, -3.750000000000000000 ) ) ;
#85548 = CARTESIAN_POINT ( 'NONE',  ( -0.7226137440361984909, -21.50112622129444162, -1.500000000000002220 ) ) ;
#85549 = CARTESIAN_POINT ( 'NONE',  ( -128.6240058187065927, -23.96119346886882084, -0.6495511937831803806 ) ) ;
#85550 = CARTESIAN_POINT ( 'NONE',  ( 32.25183987940364005, 0.3587747205144265483, 2.026414261721653176 ) ) ;
#85551 = DIRECTION ( 'NONE',  ( -3.773278334453079030E-23, 0.9999999999976377785, 2.173523156925979128E-06 ) ) ;
#85552 = CARTESIAN_POINT ( 'NONE',  ( -80.62287095715004170, -24.62285846362213348, 9.038163152653524435 ) ) ;
#85553 = CARTESIAN_POINT ( 'NONE',  ( 9.452765381649220089, 20.79790602042944414, -1.500000000000002220 ) ) ;
#85554 = VECTOR ( 'NONE', #53941, 1000.000000000000227 ) ;
#85555 = B_SPLINE_CURVE_WITH_KNOTS ( 'NONE', 3,
 ( #94005, #8779, #39217, #23991, #64093, #40232 ),
 .UNSPECIFIED., .F., .F.,
 ( 4, 2, 4 ),
 ( 1.570755371633875854E-05, 0.001396183895866087753, 0.002776660238015836446 ),
 .UNSPECIFIED. ) ;
#85556 = PERSON_AND_ORGANIZATION_ROLE ( 'creator' ) ;
#85557 = CYLINDRICAL_SURFACE ( 'NONE', #80709, 28.45799999999999486 ) ;
#85558 = CARTESIAN_POINT ( 'NONE',  ( -53.55343082792221310, -23.96119346886879953, -0.6495511937832126881 ) ) ;
#85559 = CARTESIAN_POINT ( 'NONE',  ( -16.84340083857899018, -10.81494551495373457, 11.49999999999999645 ) ) ;
#85560 = CARTESIAN_POINT ( 'NONE',  ( -79.24831702480813078, -25.31594428705783528, 5.024332805295591342 ) ) ;
#85561 = DIRECTION ( 'NONE',  ( -0.000000000000000000, -1.000000000000000000, -0.000000000000000000 ) ) ;
#85562 = VECTOR ( 'NONE', #57907, 1000.000000000000000 ) ;
#85563 = CARTESIAN_POINT ( 'NONE',  ( 4.959895098850171102, -5.876774720514411854, 19.67755022954121813 ) ) ;
#85564 = LINE ( 'NONE', #40898, #18096 ) ;
#85565 = ORIENTED_EDGE ( 'NONE', *, *, #40780, .F. ) ;
#85566 = CARTESIAN_POINT ( 'NONE',  ( -79.34687923781922336, -25.27781941911278807, 5.960409260969139922 ) ) ;
#85567 = CARTESIAN_POINT ( 'NONE',  ( 19.96715809174937561, -8.635335823514383335, -1.500000000000002220 ) ) ;
#85568 = PLANE ( 'NONE',  #78716 ) ;
#85569 = CARTESIAN_POINT ( 'NONE',  ( -19.67010641940559168, 0.002901314006966619011, -1.500000000000002220 ) ) ;
#85570 = DIRECTION ( 'NONE',  ( -3.773278334453079030E-23, 0.9999999999976377785, 2.173523156925978705E-06 ) ) ;
#85571 = ADVANCED_FACE ( 'NONE', ( #97179 ), #66165, .F. ) ;
#85572 = CARTESIAN_POINT ( 'NONE',  ( -41.41142090293942601, -25.25399135992076083, 3.882215004696675908 ) ) ;
#85573 = COORDINATED_UNIVERSAL_TIME_OFFSET ( 0, 0, .AHEAD. ) ;
#85574 = CARTESIAN_POINT ( 'NONE',  ( -38.62287095715005592, -23.47596703998600276, 11.44779298504227505 ) ) ;
#85575 = CARTESIAN_POINT ( 'NONE',  ( -92.52287095715006160, -29.50250786944525672, 11.44777988621623344 ) ) ;
#85576 = CARTESIAN_POINT ( 'NONE',  ( 11.93631617611541351, -16.73449621718459923, 11.49999999999999645 ) ) ;
#85577 = CARTESIAN_POINT ( 'NONE',  ( -94.52287095715000476, -23.94994826722564341, -0.6494450866342716955 ) ) ;
#85578 = CARTESIAN_POINT ( 'NONE',  ( -120.5196240066739648, -24.15503026093913874, -0.2815557561904507011 ) ) ;
#85580 = EDGE_CURVE ( 'NONE', #82409, #47215, #74339, .T. ) ;
#85579 = CARTESIAN_POINT ( 'NONE',  ( -22.55165446212525993, 1.111233042438415808, 11.49999999999999645 ) ) ;
#85581 = ORIENTED_EDGE ( 'NONE', *, *, #41367, .T. ) ;
#85582 = CARTESIAN_POINT ( 'NONE',  ( -100.2051565992114632, -25.31296438552667993, 4.680112719389787124 ) ) ;
#85583 = LINE ( 'NONE', #33296, #745 ) ;
#85584 = CARTESIAN_POINT ( 'NONE',  ( -125.5202163252652525, -24.52399227489127043, 9.353111116836528183 ) ) ;
#85585 = CARTESIAN_POINT ( 'NONE',  ( 14.99708669145757511, -3.499965418336752343, -27.33093470766933564 ) ) ;
#85586 = CARTESIAN_POINT ( 'NONE',  ( -25.63919700385670453, -24.61459675201335173, 6.233790649395326788 ) ) ;
#85587 = DIRECTION ( 'NONE',  ( -1.413818403454611288E-16, 1.000000000000000000, 0.000000000000000000 ) ) ;
#85588 = VERTEX_POINT ( 'NONE', #36778 ) ;
#85589 = CARTESIAN_POINT ( 'NONE',  ( -3.381418692465893105, -22.81955385325859709, 11.49999999999999645 ) ) ;
#85590 = CARTESIAN_POINT ( 'NONE',  ( 20.42703387425654427, 10.12935691860780985, 11.49999999999998934 ) ) ;
#85591 = CARTESIAN_POINT ( 'NONE',  ( -74.54989380979742464, -24.15543982623906771, -0.2315651400026650653 ) ) ;
#85592 = B_SPLINE_SURFACE_WITH_KNOTS ( 'NONE', 3, 3, ( 
 ( #44656, #7583, #82707, #29416 ),
 ( #69490, #92811, #98925, #29918 ),
 ( #53774, #60885, #13184, #100407 ),
 ( #91319, #21791, #22289, #53270 ),
 ( #67998, #28922, #84200, #36531 ),
 ( #52767, #6584, #99424, #46155 ),
 ( #13686, #98420, #59893, #91814 ) ),
 .UNSPECIFIED., .F., .F., .F.,
 ( 4, 3, 4 ),
 ( 4, 4 ),
 ( 0.7945040050992243641, 0.8970133687736501216, 0.9995227324480757680 ),
 ( 0.2795650385958281525, 0.2807068289243159764 ),
 .UNSPECIFIED. ) ;
#85593 = CARTESIAN_POINT ( 'NONE',  ( -5.205649524681222218, -6.376774720514406525, 19.16400979764067714 ) ) ;
#85594 = CARTESIAN_POINT ( 'NONE',  ( -89.52287095715006160, -23.47596703998600631, 11.44779298504228393 ) ) ;
#85595 = CARTESIAN_POINT ( 'NONE',  ( -16.84940295534276800, 14.81145437567392698, 11.49999999999999645 ) ) ;
#85596 = ORIENTED_EDGE ( 'NONE', *, *, #75642, .F. ) ;
#85597 = CARTESIAN_POINT ( 'NONE',  ( -40.01839366089613748, -29.50249496284529727, 5.509678924691796098 ) ) ;
#85598 = LINE ( 'NONE', #40441, #44873 ) ;
#85599 = CARTESIAN_POINT ( 'NONE',  ( -21.49438740719132923, 4.340694165963498996, 11.49999999999998934 ) ) ;
#85600 = CARTESIAN_POINT ( 'NONE',  ( -54.62287095715004881, -23.48783264082478084, -1.443836473390070596 ) ) ;
#85601 = EDGE_CURVE ( 'NONE', #42735, #4321, #89567, .T. ) ;
#85602 = CARTESIAN_POINT ( 'NONE',  ( -34.53824809528569517, -24.35071581493542681, 9.817618358456032368 ) ) ;
#85603 = DIRECTION ( 'NONE',  ( -1.000000000000000000, 0.000000000000000000, 0.000000000000000000 ) ) ;
#85604 = EDGE_LOOP ( 'NONE', ( #66992, #46452, #41066, #70547 ) ) ;
#85605 = CARTESIAN_POINT ( 'NONE',  ( -48.93000761175007796, -25.20616604562876617, 6.556111049017001591 ) ) ;
#85606 = DIRECTION ( 'NONE',  ( -3.773278334453079030E-23, 0.9999999999976377785, 2.173523156925979128E-06 ) ) ;
#85607 = VERTEX_POINT ( 'NONE', #59625 ) ;
#85608 = CARTESIAN_POINT ( 'NONE',  ( 12.80116962295325322, 15.99954467330607244, 11.49999999999998934 ) ) ;
#85609 = EDGE_LOOP ( 'NONE', ( #33962, #95659, #82245, #54814 ) ) ;
#85610 = EDGE_LOOP ( 'NONE', ( #35731, #75442, #58355, #60077 ) ) ;
#85611 = VERTEX_POINT ( 'NONE', #27673 ) ;
#85612 = EDGE_LOOP ( 'NONE', ( #77028, #35476, #17856, #90608 ) ) ;
#85613 = CARTESIAN_POINT ( 'NONE',  ( -20.32320236877023589, 10.94715076914730290, -1.500000000000002220 ) ) ;
#85614 = CARTESIAN_POINT ( 'NONE',  ( -49.37922875195936001, -25.19117186706260014, 3.263664075997171121 ) ) ;
#85615 = CARTESIAN_POINT ( 'NONE',  ( -15.70679263237263434, -12.88635299011707502, -1.500000000000002220 ) ) ;
#85616 = ORIENTED_EDGE ( 'NONE', *, *, #69641, .F. ) ;
#85617 = ADVANCED_FACE ( 'NONE', ( #4831 ), #56391, .T. ) ;
#85618 = CARTESIAN_POINT ( 'NONE',  ( -27.13414387080440093, -5.965225279485594001, -10.21530720150730254 ) ) ;
#85619 = ADVANCED_FACE ( 'NONE', ( #90557 ), #66754, .F. ) ;
#85620 = AXIS2_PLACEMENT_3D ( 'NONE', #5459, #22164, #83573 ) ;
#85621 = CARTESIAN_POINT ( 'NONE',  ( -92.63387814436620715, -23.96119346886881374, -0.6495511937831873750 ) ) ;
#85622 = EDGE_CURVE ( 'NONE', #40572, #69058, #82936, .T. ) ;
#85623 = B_SPLINE_CURVE_WITH_KNOTS ( 'NONE', 3,
 ( #28176, #83443, #14430, #21044, #38268, #67749 ),
 .UNSPECIFIED., .F., .F.,
 ( 4, 2, 4 ),
 ( 6.391158118972359742E-06, 0.001387004593080793302, 0.002767618028042614139 ),
 .UNSPECIFIED. ) ;
#85624 = DIRECTION ( 'NONE',  ( -0.000000000000000000, -1.000000000000000000, 0.000000000000000000 ) ) ;
#85625 = CARTESIAN_POINT ( 'NONE',  ( -70.62368311109368335, -25.00158670708910691, 2.256160236439221034 ) ) ;
#85627 = ORIENTED_EDGE ( 'NONE', *, *, #70392, .F. ) ;
#85626 = CARTESIAN_POINT ( 'NONE',  ( -19.93307770644097232, -8.117153041090405807, 11.49999999999999645 ) ) ;
#85628 = CARTESIAN_POINT ( 'NONE',  ( -125.5895376238167245, -24.99132157543083821, 2.256160258750496528 ) ) ;
#85629 = CARTESIAN_POINT ( 'NONE',  ( 15.99960863614631101, 3.577630190450212577, -27.91116951066581819 ) ) ;
#85630 = EDGE_CURVE ( 'NONE', #57287, #40266, #5820, .T. ) ;
#85631 = ORIENTED_EDGE ( 'NONE', *, *, #63941, .T. ) ;
#85632 = CARTESIAN_POINT ( 'NONE',  ( -2.856624844580134770, 20.53689577262001364, 11.49999999999998934 ) ) ;
#85633 = ORIENTED_EDGE ( 'NONE', *, *, #91231, .T. ) ;
#85635 = VERTEX_POINT ( 'NONE', #20051 ) ;
#85634 = DIRECTION ( 'NONE',  ( 0.000000000000000000, 0.000000000000000000, 1.000000000000000000 ) ) ;
#85636 = CARTESIAN_POINT ( 'NONE',  ( -111.6321636762771448, -23.48786465467241769, 11.44779295918254114 ) ) ;
#85637 = CARTESIAN_POINT ( 'NONE',  ( -43.62287095715004881, -29.50250243563736774, 8.947779886222148704 ) ) ;
#85638 = ORIENTED_EDGE ( 'NONE', *, *, #76585, .F. ) ;
#85639 = VERTEX_POINT ( 'NONE', #21529 ) ;
#85640 = LINE ( 'NONE', #31864, #46179 ) ;
#85641 = B_SPLINE_CURVE_WITH_KNOTS ( 'NONE', 3,
 ( #73752, #97091, #67655, #4251, #43316, #13834 ),
 .UNSPECIFIED., .F., .F.,
 ( 4, 2, 4 ),
 ( 0.004212217532641997220, 0.005885052055372064564, 0.007557886578102131908 ),
 .UNSPECIFIED. ) ;
#85642 = AXIS2_PLACEMENT_3D ( 'NONE', #35922, #60772, #14069 ) ;
#85643 = B_SPLINE_CURVE_WITH_KNOTS ( 'NONE', 3,
 ( #63822, #94233, #88139, #55197 ),
 .UNSPECIFIED., .F., .F.,
 ( 4, 4 ),
 ( 0.000000000000000000, 9.999999999998897304E-05 ),
 .UNSPECIFIED. ) ;
#85644 = CARTESIAN_POINT ( 'NONE',  ( -117.5228709571500758, -23.47596703998600631, 11.44779298504227860 ) ) ;
#85645 = B_SPLINE_CURVE_WITH_KNOTS ( 'NONE', 3,
 ( #89970, #20445, #37180, #45301, #68136, #15827 ),
 .UNSPECIFIED., .F., .F.,
 ( 4, 2, 4 ),
 ( 1.570755371633836552E-05, 0.001396183895866087753, 0.002776660238015836880 ),
 .UNSPECIFIED. ) ;
#85647 = EDGE_CURVE ( 'NONE', #22875, #29959, #30430, .T. ) ;
#85646 = CARTESIAN_POINT ( 'NONE',  ( -76.52287095715007581, -24.66019654487199730, 8.947790411086124607 ) ) ;
#85648 = EDGE_CURVE ( 'NONE', #71695, #47216, #13924, .T. ) ;
#85649 = CARTESIAN_POINT ( 'NONE',  ( 13.08019894233326319, 17.74467248152726384, 11.49999999999999645 ) ) ;
#85650 = DIRECTION ( 'NONE',  ( 1.000000000000000000, 0.000000000000000000, 0.000000000000000000 ) ) ;
#85651 = CARTESIAN_POINT ( 'NONE',  ( 21.27769986149581172, 7.469961712261545372, 11.49999999999998934 ) ) ;
#85652 = CARTESIAN_POINT ( 'NONE',  ( 20.99820426035194032, -0.1900765340283884497, 11.49999999999998934 ) ) ;
#85653 = CARTESIAN_POINT ( 'NONE',  ( 27.53860345374808105, 4.772774720514425972, -6.982392034746241372 ) ) ;
#85655 = EDGE_CURVE ( 'NONE', #51201, #10079, #19641, .T. ) ;
#85654 = ORIENTED_EDGE ( 'NONE', *, *, #69583, .T. ) ;
#85656 = VECTOR ( 'NONE', #12320, 1000.000000000000000 ) ;
#85657 = ORIENTED_EDGE ( 'NONE', *, *, #93238, .F. ) ;
#85658 = CARTESIAN_POINT ( 'NONE',  ( -80.62287095715004170, -24.91544648472620338, 1.928969306349224810 ) ) ;
#85659 = ADVANCED_FACE ( 'NONE', ( #98659 ), #52506, .T. ) ;
#85660 = DIRECTION ( 'NONE',  ( 1.000000000000000000, 0.000000000000000000, 0.000000000000000000 ) ) ;
#85661 = ORIENTED_EDGE ( 'NONE', *, *, #91967, .F. ) ;
#85662 = CARTESIAN_POINT ( 'NONE',  ( 19.19679251752027227, 8.867671107084703408, 11.49999999999998934 ) ) ;
#85663 = DIRECTION ( 'NONE',  ( 0.000000000000000000, 0.000000000000000000, -1.000000000000000000 ) ) ;
#85664 = CARTESIAN_POINT ( 'NONE',  ( -51.83680534327738343, -25.26040924062689896, 6.675008265709720057 ) ) ;
#85665 = CARTESIAN_POINT ( 'NONE',  ( -88.62287095715004170, -23.47596703998600631, 11.44779298504227860 ) ) ;
#85666 = DIRECTION ( 'NONE',  ( -3.773278334453079030E-23, 0.9999999999976377785, 2.173523156925979128E-06 ) ) ;
#85667 = DIRECTION ( 'NONE',  ( -0.1593164160933057683, 0.000000000000000000, 0.9872275723272647685 ) ) ;
#85668 = CARTESIAN_POINT ( 'NONE',  ( -10.56713949322891999, -19.48831581008217384, -1.500000000000002220 ) ) ;
#85669 = CARTESIAN_POINT ( 'NONE',  ( -71.54135322174539624, -24.51314013834315730, 0.6176544820404130665 ) ) ;
#85670 = EDGE_CURVE ( 'NONE', #80003, #396, #19546, .T. ) ;
#85671 = ORIENTED_EDGE ( 'NONE', *, *, #63082, .T. ) ;
#85672 = CARTESIAN_POINT ( 'NONE',  ( -51.77186309286971522, -25.24860127752034700, 5.562993739656123537 ) ) ;
#85673 = CARTESIAN_POINT ( 'NONE',  ( -37.52201680321181243, -23.48783264082477729, -1.443836473390075703 ) ) ;
#85674 = CARTESIAN_POINT ( 'NONE',  ( -126.5547695978490310, -24.65952944569306027, 1.056160979905708786 ) ) ;
#85675 = EDGE_CURVE ( 'NONE', #80353, #8894, #66255, .T. ) ;
#85676 = CARTESIAN_POINT ( 'NONE',  ( 13.91401389203221406, -6.376774720514426953, 158.0376437107427137 ) ) ;
#85677 = CARTESIAN_POINT ( 'NONE',  ( 15.92621150404962016, 6.475225279485573360, -27.29681269571041824 ) ) ;
#85678 = B_SPLINE_CURVE_WITH_KNOTS ( 'NONE', 3,
 ( #97447, #59900, #82713, #45169 ),
 .UNSPECIFIED., .F., .F.,
 ( 4, 4 ),
 ( 0.000000000000000000, 1.000000000000000000 ),
 .UNSPECIFIED. ) ;
#85679 = EDGE_CURVE ( 'NONE', #75373, #60109, #83953, .T. ) ;
#85680 = CARTESIAN_POINT ( 'NONE',  ( 15.33136405852079243, -11.96835230219363311, -1.500000000000002220 ) ) ;
#85681 = CARTESIAN_POINT ( 'NONE',  ( -17.32345979880200204, -12.59856583755568415, 11.49999999999998934 ) ) ;
#85682 = CARTESIAN_POINT ( 'NONE',  ( -62.62751418018152094, -24.51314013834316441, 0.6176544820404141767 ) ) ;
#85683 = CARTESIAN_POINT ( 'NONE',  ( 9.478389368232452483, 2.682774720514426559, -23.17485683983816003 ) ) ;
#85684 = DIRECTION ( 'NONE',  ( -0.000000000000000000, -1.000000000000000000, -0.000000000000000000 ) ) ;
#85685 = CARTESIAN_POINT ( 'NONE',  ( -101.3603016561062589, -25.27360118438346248, 3.955748476195026342 ) ) ;
#85686 = CARTESIAN_POINT ( 'NONE',  ( -17.38503614929206265, -14.63273120789127013, -1.500000000000002220 ) ) ;
#85687 = B_SPLINE_SURFACE_WITH_KNOTS ( 'NONE', 3, 3, ( 
 ( #57914, #3622, #88858, #49806 ),
 ( #26946, #34066, #56418, #87337 ),
 ( #50295, #73130, #80738, #19323 ),
 ( #87850, #34569, #81232, #11710 ),
 ( #73624, #48802, #4116, #35065 ),
 ( #80232, #96955, #56917, #64041 ),
 ( #94956, #79724, #72635, #41178 ) ),
 .UNSPECIFIED., .F., .F., .F.,
 ( 4, 3, 4 ),
 ( 4, 4 ),
 ( 0.0004766839783816872339, 0.1029713700210893590, 0.2054660560637970312 ),
 ( 0.5696389036532559791, 0.5709144585527624605 ),
 .UNSPECIFIED. ) ;
#85688 = CARTESIAN_POINT ( 'NONE',  ( -98.51627647636760798, -23.96119346886880663, -0.6495511937832080251 ) ) ;
#85689 = CARTESIAN_POINT ( 'NONE',  ( -58.52287095715006160, -29.50250243563736774, 8.947779886222145151 ) ) ;
#85690 = CARTESIAN_POINT ( 'NONE',  ( 11.24879072547334324, 16.40116332625411033, 11.49999999999999645 ) ) ;
#85691 = CARTESIAN_POINT ( 'NONE',  ( -123.5563712641698118, -23.73791477778912196, 11.05961554403169878 ) ) ;
#85692 = VECTOR ( 'NONE', #85222, 1000.000000000000114 ) ;
#85693 = AXIS2_PLACEMENT_3D ( 'NONE', #59220, #65860, #96778 ) ;
#85694 = CARTESIAN_POINT ( 'NONE',  ( -3.826923076923074429, -6.376774720514427841, 21.75000000000000355 ) ) ;
#85695 = ORIENTED_EDGE ( 'NONE', *, *, #17185, .T. ) ;
#85696 = CARTESIAN_POINT ( 'NONE',  ( -49.53207283835729413, -25.17696084702891568, 6.767063398092357573 ) ) ;
#85697 = CARTESIAN_POINT ( 'NONE',  ( -5.988734693054777125, -6.376774720514415407, 19.95737465391042065 ) ) ;
#85698 = B_SPLINE_CURVE_WITH_KNOTS ( 'NONE', 3,
 ( #70347, #25160, #55132, #830 ),
 .UNSPECIFIED., .F., .F.,
 ( 4, 4 ),
 ( 0.000000000000000000, 9.999999999998897304E-05 ),
 .UNSPECIFIED. ) ;
#85699 = CARTESIAN_POINT ( 'NONE',  ( -51.66021737866784491, -25.10935945577014294, 3.699308914517982938 ) ) ;
#85700 = CARTESIAN_POINT ( 'NONE',  ( -20.56447267657262401, 6.860157381912782348, 11.49999999999998934 ) ) ;
#85701 = CARTESIAN_POINT ( 'NONE',  ( -66.55620429048339304, -24.65952944569304606, 1.056160979905697905 ) ) ;
#85702 = VECTOR ( 'NONE', #85001, 1000.000000000000000 ) ;
#85703 = CARTESIAN_POINT ( 'NONE',  ( 1.793504005174451077, 19.40006364325761012, -1.500000000000002220 ) ) ;
#85704 = LINE ( 'NONE', #54267, #70120 ) ;
#85705 = ORIENTED_EDGE ( 'NONE', *, *, #15639, .F. ) ;
#85706 = VECTOR ( 'NONE', #44425, 1000.000000000000000 ) ;
#85707 = CARTESIAN_POINT ( 'NONE',  ( -19.47531982339030776, -5.969937916086089480, 11.49999999999999645 ) ) ;
#85708 = DIRECTION ( 'NONE',  ( -0.000000000000000000, 1.000000000000000000, -0.000000000000000000 ) ) ;
#85709 = DIRECTION ( 'NONE',  ( -3.773278334453079030E-23, 0.9999999999976377785, 2.173523156925979128E-06 ) ) ;
#85710 = ORIENTED_EDGE ( 'NONE', *, *, #13678, .F. ) ;
#85711 = CARTESIAN_POINT ( 'NONE',  ( -40.58336788261102157, -25.19566465339486783, 3.298403319262286360 ) ) ;
#85712 = CARTESIAN_POINT ( 'NONE',  ( -92.52287095715006160, -23.47593901973090169, -1.443836447538996426 ) ) ;
#85713 = CARTESIAN_POINT ( 'NONE',  ( -59.80072539166535250, -25.14083923594767001, 2.947789366383931853 ) ) ;
#85714 = AXIS2_PLACEMENT_3D ( 'NONE', #49192, #57309, #97342 ) ;
#85715 = CARTESIAN_POINT ( 'NONE',  ( -128.6228709571500701, -24.51283580621365843, 0.6167428607019860287 ) ) ;
#85716 = CARTESIAN_POINT ( 'NONE',  ( -0.9078848932494473223, -6.376774720514411854, 19.67454710845354171 ) ) ;
#85717 = CARTESIAN_POINT ( 'NONE',  ( -0.3114230556345199963, -20.10660241673355486, -1.500000000000002220 ) ) ;
#85718 = CARTESIAN_POINT ( 'NONE',  ( -57.55620429048340725, -23.47593901973091235, -1.443836447539007972 ) ) ;
#85719 = ORIENTED_EDGE ( 'NONE', *, *, #20805, .T. ) ;
#85720 = CARTESIAN_POINT ( 'NONE',  ( -91.62287095715004170, -23.96177878511308634, 10.65340807706329507 ) ) ;
#85721 = CARTESIAN_POINT ( 'NONE',  ( 22.59171682324826236, -3.780823453261925593, 11.49999999999999645 ) ) ;
#85722 = CARTESIAN_POINT ( 'NONE',  ( -17.38503614929206265, -14.63273120789127013, 11.49999999999998934 ) ) ;
#85723 = ORIENTED_EDGE ( 'NONE', *, *, #98689, .F. ) ;
#85724 = CARTESIAN_POINT ( 'NONE',  ( -45.52287095715006870, -24.63287334234177450, 0.9662140553045317493 ) ) ;
#85725 = CARTESIAN_POINT ( 'NONE',  ( 10.46399479596396453, 2.682774720514426559, -27.03001098546561920 ) ) ;
#85726 = CARTESIAN_POINT ( 'NONE',  ( -24.97666371003640506, -0.3587747205143964613, -15.72894043976419454 ) ) ;
#85727 = CARTESIAN_POINT ( 'NONE',  ( -30.57287095715005520, -24.67790239037960021, 8.895694439986561619 ) ) ;
#85728 = CARTESIAN_POINT ( 'NONE',  ( 6.660000000000001030, 0.000000000000000000, 2.399999999999999911 ) ) ;
#85729 = AXIS2_PLACEMENT_3D ( 'NONE', #57636, #88578, #50510 ) ;
#85730 = CARTESIAN_POINT ( 'NONE',  ( -98.89303308397303738, -25.31200744192977581, 6.110950052045652114 ) ) ;
#85731 = VERTEX_POINT ( 'NONE', #53012 ) ;
#85732 = ADVANCED_FACE ( 'NONE', ( #46887 ), #62617, .T. ) ;
#85733 = CARTESIAN_POINT ( 'NONE',  ( 18.38310620586021571, 8.829655622120887060, 11.49999999999998934 ) ) ;
#85735 = EDGE_CURVE ( 'NONE', #7838, #44949, #66938, .T. ) ;
#85734 = ORIENTED_EDGE ( 'NONE', *, *, #3762, .F. ) ;
#85736 = CARTESIAN_POINT ( 'NONE',  ( 4.903590608199674072, 22.46510890469962263, 11.49999999999998934 ) ) ;
#85737 = CARTESIAN_POINT ( 'NONE',  ( -69.22287095715007865, -23.47596703998600276, 11.44779298504227860 ) ) ;
#85738 = EDGE_CURVE ( 'NONE', #3935, #27247, #2771, .T. ) ;
#85739 = EDGE_LOOP ( 'NONE', ( #61046, #23441, #49708, #81757 ) ) ;
#85740 = CARTESIAN_POINT ( 'NONE',  ( -114.5228709571501184, -24.35013146730204525, 9.818937971375092388 ) ) ;
#85741 = EDGE_CURVE ( 'NONE', #10167, #42367, #40321, .T. ) ;
#85743 = EDGE_CURVE ( 'NONE', #36332, #18512, #23970, .T. ) ;
#85742 = CARTESIAN_POINT ( 'NONE',  ( -84.62287095715002749, -23.96127896941631619, -0.6493128931037801532 ) ) ;
#85744 = CARTESIAN_POINT ( 'NONE',  ( -89.58953762381671027, -24.65952944569304961, 1.056160979905700126 ) ) ;
#85746 = VERTEX_POINT ( 'NONE', #61627 ) ;
#85745 = CARTESIAN_POINT ( 'NONE',  ( -16.05942832139214360, -14.02155611864158402, 11.49999999999999645 ) ) ;
#85747 = EDGE_LOOP ( 'NONE', ( #29849, #21434 ) ) ;
#85748 = CARTESIAN_POINT ( 'NONE',  ( -2.516727866726558460, 22.04588476715296963, 11.49999999999998934 ) ) ;
#85749 = CARTESIAN_POINT ( 'NONE',  ( -3.285303218690974525, -20.39892020120133154, -1.500000000000002220 ) ) ;
#85750 = ORIENTED_EDGE ( 'NONE', *, *, #89531, .T. ) ;
#85751 = EDGE_LOOP ( 'NONE', ( #28149, #50000, #7648, #5493 ) ) ;
#85752 = CARTESIAN_POINT ( 'NONE',  ( -4.886549725601808447, -5.876774720514410077, 19.15251819062245175 ) ) ;
#85753 = CARTESIAN_POINT ( 'NONE',  ( -95.64416487886954599, -23.48786465467241058, 11.44779295918254469 ) ) ;
#85754 = VERTEX_POINT ( 'NONE', #84936 ) ;
#85755 = CARTESIAN_POINT ( 'NONE',  ( -91.50436023160280286, -24.65952944569304606, 1.056160979905703234 ) ) ;
#85756 = VECTOR ( 'NONE', #35321, 1000.000000000000114 ) ;
#85757 = VERTEX_POINT ( 'NONE', #22521 ) ;
#85758 = CARTESIAN_POINT ( 'NONE',  ( -58.54813711902425410, -24.15620529776628089, 10.23563542870660470 ) ) ;
#85759 = DIRECTION ( 'NONE',  ( -3.773278334453079618E-23, 0.9999999999976377785, 2.173523156925978705E-06 ) ) ;
#85760 = CARTESIAN_POINT ( 'NONE',  ( 5.579783289733251550, -20.15082174716252794, -1.500000000000002220 ) ) ;
#85761 = EDGE_CURVE ( 'NONE', #54721, #97694, #76808, .T. ) ;
#85762 = CARTESIAN_POINT ( 'NONE',  ( 21.83686239284238084, -0.8075297431944471471, 11.49999999999999645 ) ) ;
#85763 = CARTESIAN_POINT ( 'NONE',  ( -27.61674701359889639, -24.77993797186285008, 7.602796574010316277 ) ) ;
#85764 = CARTESIAN_POINT ( 'NONE',  ( -78.50858408022973833, -24.15620529776628445, 10.23563542870660292 ) ) ;
#85765 = CARTESIAN_POINT ( 'NONE',  ( 11.54466316424315231, -19.26756404802103972, -1.500000000000002220 ) ) ;
#85766 = VECTOR ( 'NONE', #81773, 999.9999999999998863 ) ;
#85767 = CARTESIAN_POINT ( 'NONE',  ( -38.56988824117014758, -23.48783264082477729, -1.443836473390076591 ) ) ;
#85768 = CARTESIAN_POINT ( 'NONE',  ( -87.55620429048337883, -23.48783264082478084, -1.443836473390063269 ) ) ;
#85769 = CARTESIAN_POINT ( 'NONE',  ( 3.797776442307698286, -5.876774720514427841, 21.83974358974358410 ) ) ;
#85770 = ADVANCED_FACE ( 'NONE', ( #15421 ), #77314, .F. ) ;
#85771 = AXIS2_PLACEMENT_3D ( 'NONE', #8366, #29213, #69775 ) ;
#85772 = VERTEX_POINT ( 'NONE', #39261 ) ;
#85773 = CIRCLE ( 'NONE', #72829, 252.4458649670781085 ) ;
#85774 = ORIENTED_EDGE ( 'NONE', *, *, #20550, .T. ) ;
#85775 = B_SPLINE_CURVE_WITH_KNOTS ( 'NONE', 3,
 ( #53899, #15314, #85328, #24434 ),
 .UNSPECIFIED., .F., .F.,
 ( 4, 4 ),
 ( 0.000000000000000000, 0.0001000000000000028644 ),
 .UNSPECIFIED. ) ;
#85776 = EDGE_LOOP ( 'NONE', ( #85565, #58181, #24784, #38063 ) ) ;
#85777 = B_SPLINE_CURVE_WITH_KNOTS ( 'NONE', 3,
 ( #76494, #84621, #82621, #75999 ),
 .UNSPECIFIED., .F., .F.,
 ( 4, 4 ),
 ( 1.387778780781445676E-17, 0.0001000000000000028508 ),
 .UNSPECIFIED. ) ;
#85778 = VECTOR ( 'NONE', #30229, 1000.000000000000000 ) ;
#85779 = CARTESIAN_POINT ( 'NONE',  ( -20.51402961445061734, 6.013860829077147585, -1.500000000000002220 ) ) ;
#85780 = CARTESIAN_POINT ( 'NONE',  ( 15.07672925556244969, 16.42598562245719407, 11.49999999999999645 ) ) ;
#85781 = ORIENTED_EDGE ( 'NONE', *, *, #24326, .F. ) ;
#85782 = CARTESIAN_POINT ( 'NONE',  ( -21.07084664159375009, 0.3847054351051909515, -1.500000000000002220 ) ) ;
#85783 = CARTESIAN_POINT ( 'NONE',  ( -30.42979910109433916, -24.56868136509832112, 0.8299800598022502029 ) ) ;
#85784 = CARTESIAN_POINT ( 'NONE',  ( -12.66726347749767179, -15.43046242340049545, -1.500000000000002220 ) ) ;
#85785 = CARTESIAN_POINT ( 'NONE',  ( -50.53276790146632891, -24.73531770709094602, 8.716586749053508498 ) ) ;
#85786 = CARTESIAN_POINT ( 'NONE',  ( -49.36964668519517829, -25.11052413561256813, 7.227227948084789411 ) ) ;
#85787 = CARTESIAN_POINT ( 'NONE',  ( 1.410849576418898632, -21.91845101833037290, -1.500000000000002220 ) ) ;
#85788 = CARTESIAN_POINT ( 'NONE',  ( -76.58953762381673869, -24.65952944569304606, 1.056160979905704123 ) ) ;
#85789 = ORIENTED_EDGE ( 'NONE', *, *, #11656, .T. ) ;
#85790 = LINE ( 'NONE', #62969, #51655 ) ;
#85791 = LINE ( 'NONE', #31495, #23831 ) ;
#85792 = CARTESIAN_POINT ( 'NONE',  ( 16.20321855003292555, -13.12800272717607619, 11.49999999999999645 ) ) ;
#85793 = ADVANCED_FACE ( 'NONE', ( #78315 ), #37198, .T. ) ;
#85794 = CARTESIAN_POINT ( 'NONE',  ( 29.61860529676591369, -5.187414344753652706, 28.58826086137218780 ) ) ;
#85795 = B_SPLINE_CURVE_WITH_KNOTS ( 'NONE', 3,
 ( #94043, #24528, #20287, #81209 ),
 .UNSPECIFIED., .F., .F.,
 ( 4, 4 ),
 ( 0.000000000000000000, 9.999999999997510880E-05 ),
 .UNSPECIFIED. ) ;
#85796 = CARTESIAN_POINT ( 'NONE',  ( -125.5228709571501184, -24.51254535375844057, 9.355368624242190734 ) ) ;
#85797 = CARTESIAN_POINT ( 'NONE',  ( -28.47875734969025885, -6.475225279485573360, -0.08597719988137300651 ) ) ;
#85798 = CARTESIAN_POINT ( 'NONE',  ( -21.20786952941880443, -2.223526401999901925, -1.500000000000002220 ) ) ;
#85799 = CARTESIAN_POINT ( 'NONE',  ( -98.55771473076809741, -23.73791477778912196, 11.05961554403170588 ) ) ;
#85800 = DIRECTION ( 'NONE',  ( -3.773278334453080206E-23, 0.9999999999976377785, 2.173523156925979975E-06 ) ) ;
#85801 = ADVANCED_FACE ( 'NONE', ( #65135 ), #48387, .T. ) ;
#85802 = CARTESIAN_POINT ( 'NONE',  ( -110.9353407762807251, -25.06732983082694943, 7.447789526168955732 ) ) ;
#85803 = CARTESIAN_POINT ( 'NONE',  ( 22.02124265030973760, -6.143225279485574397, 16.20402280011862217 ) ) ;
#85804 = CARTESIAN_POINT ( 'NONE',  ( 5.133194422563156500, 21.89913303424002677, -1.500000000000002220 ) ) ;
#85805 = DIRECTION ( 'NONE',  ( 0.000000000000000000, 0.9999999999976377785, 2.173523156925979975E-06 ) ) ;
#85806 = ORIENTED_EDGE ( 'NONE', *, *, #34831, .T. ) ;
#85807 = CARTESIAN_POINT ( 'NONE',  ( -79.88859889895181254, -25.29802671295835026, 4.572338242537191455 ) ) ;
#85808 = CARTESIAN_POINT ( 'NONE',  ( -31.48872353745126773, -24.35071581493542325, 9.817618358456039473 ) ) ;
#85809 = CARTESIAN_POINT ( 'NONE',  ( -16.89733858281218204, -10.06102416988892934, 11.49999999999999645 ) ) ;
#85810 = CARTESIAN_POINT ( 'NONE',  ( 32.98733314340959311, 5.965225279485572685, 2.074222136288530027 ) ) ;
#85811 = CARTESIAN_POINT ( 'NONE',  ( 14.75122623597949101, -4.701663563191170070, -27.79036425924725151 ) ) ;
#85812 = ORIENTED_EDGE ( 'NONE', *, *, #69351, .F. ) ;
#85813 = CARTESIAN_POINT ( 'NONE',  ( -99.56067757241656579, -23.48783264082478439, -1.443836473390063047 ) ) ;
#85814 = CARTESIAN_POINT ( 'NONE',  ( 31.64143112576189765, 5.965225279485572685, 14.03360796525321774 ) ) ;
#85815 = CARTESIAN_POINT ( 'NONE',  ( -124.5888231589337209, -24.66019654487200441, 8.947790411086108620 ) ) ;
#85816 = DIRECTION ( 'NONE',  ( 0.000000000000000000, 0.000000000000000000, 1.000000000000000000 ) ) ;
#85817 = CARTESIAN_POINT ( 'NONE',  ( -0.6023826358649750912, 19.72334862104828090, 11.49999999999998934 ) ) ;
#85818 = ORIENTED_EDGE ( 'NONE', *, *, #65393, .T. ) ;
#85819 = CARTESIAN_POINT ( 'NONE',  ( 9.146648804574669001, 3.316774720514593433, -28.07004961703220758 ) ) ;
#85820 = CIRCLE ( 'NONE', #95596, 15.00000000000000178 ) ;
#85821 = DATE_TIME_ROLE ( 'creation_date' ) ;
#85822 = ORIENTED_EDGE ( 'NONE', *, *, #17875, .F. ) ;
#85823 = DIRECTION ( 'NONE',  ( 0.000000000000000000, 0.9999999999976377785, 2.173523156925979128E-06 ) ) ;
#85824 = DIRECTION ( 'NONE',  ( 3.773278334444167608E-23, -1.000000000000000000, 0.000000000000000000 ) ) ;
#85825 = CARTESIAN_POINT ( 'NONE',  ( -4.568292318365942073, -0.3587747205144265483, 30.06720597538392425 ) ) ;
#85826 = CARTESIAN_POINT ( 'NONE',  ( 32.29806486058159010, -4.575840390334028562, -4.131869215359018632 ) ) ;
#85827 = CARTESIAN_POINT ( 'NONE',  ( 6.371704462700114924, -6.376774720514427841, 21.83798798526824214 ) ) ;
#85828 = CIRCLE ( 'NONE', #8035, 2.000000000000001776 ) ;
#85829 = CARTESIAN_POINT ( 'NONE',  ( -41.55620429048340014, -24.66019654487199020, 8.947790411086135265 ) ) ;
#85830 = CARTESIAN_POINT ( 'NONE',  ( -40.49165087243459737, -25.30353303947430987, 5.543942858925161588 ) ) ;
#85831 = CARTESIAN_POINT ( 'NONE',  ( -7.547287378330592489, -18.53391252851691462, -1.500000000000002220 ) ) ;
#85832 = PLANE ( 'NONE',  #15943 ) ;
#85833 = CARTESIAN_POINT ( 'NONE',  ( 31.55507366846311967, -4.132774720514426292, -2.076992067079099336 ) ) ;
#85834 = ORIENTED_EDGE ( 'NONE', *, *, #18627, .F. ) ;
#85835 = AXIS2_PLACEMENT_3D ( 'NONE', #1801, #21734, #32738 ) ;
#85836 = VECTOR ( 'NONE', #31861, 1000.000000000000114 ) ;
#85837 = CARTESIAN_POINT ( 'NONE',  ( -79.52213156321093379, -23.48786465467241058, 11.44779295918254824 ) ) ;
#85838 = CARTESIAN_POINT ( 'NONE',  ( -109.3584176993576591, -25.18430352096120473, 4.206202733454734499 ) ) ;
#85839 = CARTESIAN_POINT ( 'NONE',  ( -35.65502281178025612, -24.15503026093914940, -0.2815557561904327155 ) ) ;
#85840 = CARTESIAN_POINT ( 'NONE',  ( -100.5228709571500332, -24.15516710230296482, 10.28746687063728160 ) ) ;
#85841 = VECTOR ( 'NONE', #73266, 1000.000000000000000 ) ;
#85842 = DIRECTION ( 'NONE',  ( -0.000000000000000000, -1.000000000000000000, -0.000000000000000000 ) ) ;
#85843 = PLANE ( 'NONE',  #79363 ) ;
#85844 = AXIS2_PLACEMENT_3D ( 'NONE', #71183, #64092, #25501 ) ;
#85845 = CARTESIAN_POINT ( 'NONE',  ( -63.62287095715004881, -23.96177878511307568, 10.65340807706329862 ) ) ;
#85846 = CARTESIAN_POINT ( 'NONE',  ( -44.62287095715004881, -29.50250786944525672, 11.44777988621624232 ) ) ;
#85847 = EDGE_LOOP ( 'NONE', ( #67192, #85734, #53459, #44582 ) ) ;
#85848 = CARTESIAN_POINT ( 'NONE',  ( -18.37190169643047355, -11.86832528159398237, -1.500000000000002220 ) ) ;
#85849 = EDGE_CURVE ( 'NONE', #94640, #42958, #78944, .T. ) ;
#85850 = CARTESIAN_POINT ( 'NONE',  ( 18.82434097252966154, -7.598309640217090433, -1.500000000000002220 ) ) ;
#85851 = PLANE ( 'NONE',  #40435 ) ;
#85852 = ADVANCED_FACE ( 'NONE', ( #10819 ), #76085, .T. ) ;
#85853 = CARTESIAN_POINT ( 'NONE',  ( -52.62287095715005592, -29.50247984919015209, -1.443849546365058689 ) ) ;
#85854 = EDGE_CURVE ( 'NONE', #45470, #100015, #48894, .T. ) ;
#85855 = ORIENTED_EDGE ( 'NONE', *, *, #84368, .F. ) ;
#85856 = LINE ( 'NONE', #62523, #29110 ) ;
#85857 = CARTESIAN_POINT ( 'NONE',  ( 9.931738293602487389, -17.53800358597336384, -1.500000000000002220 ) ) ;
#85858 = B_SPLINE_CURVE_WITH_KNOTS ( 'NONE', 3,
 ( #842, #39901, #7949, #24172 ),
 .UNSPECIFIED., .F., .F.,
 ( 4, 4 ),
 ( 0.000000000000000000, 9.999999999998897304E-05 ),
 .UNSPECIFIED. ) ;
#85859 = ADVANCED_FACE ( 'NONE', ( #80835 ), #88450, .F. ) ;
#85860 = CARTESIAN_POINT ( 'NONE',  ( -21.09505027744838657, -1.104435277493458045, 11.49999999999999645 ) ) ;
#85861 = CARTESIAN_POINT ( 'NONE',  ( 16.06085343747454175, -15.19291221174989204, -1.500000000000002220 ) ) ;
#85862 = EDGE_CURVE ( 'NONE', #55233, #81363, #83796, .T. ) ;
#85863 = CARTESIAN_POINT ( 'NONE',  ( -6.092534927433182368, -19.63929903328317295, -1.500000000000002220 ) ) ;
#85864 = CARTESIAN_POINT ( 'NONE',  ( -60.63671166649558586, -24.52300882791528380, 0.6510814631126233820 ) ) ;
#85865 = ORIENTED_EDGE ( 'NONE', *, *, #45430, .T. ) ;
#85866 = CYLINDRICAL_SURFACE ( 'NONE', #81686, 10.11363636363636331 ) ;
#85867 = EDGE_LOOP ( 'NONE', ( #40967, #46346, #75216, #3599 ) ) ;
#85868 = DIRECTION ( 'NONE',  ( 1.000000000000000000, 3.773278334444166432E-23, 8.201307841325785021E-29 ) ) ;
#85869 = CARTESIAN_POINT ( 'NONE',  ( -109.5228709571500332, -24.50321055353806088, 9.387540953477524042 ) ) ;
#85870 = EDGE_LOOP ( 'NONE', ( #3553, #66726, #92349, #68166 ) ) ;
#85871 = ORIENTED_EDGE ( 'NONE', *, *, #43964, .T. ) ;
#85872 = EDGE_LOOP ( 'NONE', ( #74794, #22939, #69560, #29093 ) ) ;
#85873 = CARTESIAN_POINT ( 'NONE',  ( -100.5228709571500474, -24.91544648472620693, 1.928969306349232582 ) ) ;
#85874 = DIRECTION ( 'NONE',  ( 0.000000000000000000, 2.173523156925980399E-06, -0.9999999999976378895 ) ) ;
#85875 = DIRECTION ( 'NONE',  ( -1.000000000000000000, 0.000000000000000000, 0.000000000000000000 ) ) ;
#85876 = CARTESIAN_POINT ( 'NONE',  ( -19.40337959798338119, 7.141409694766009508, -1.500000000000002220 ) ) ;
#85877 = CARTESIAN_POINT ( 'NONE',  ( 7.679218611123722837, 20.28660689097963399, 11.49999999999999645 ) ) ;
#85878 = EDGE_LOOP ( 'NONE', ( #11703, #22941, #36831, #46069, #100101, #53573, #19129 ) ) ;
#85879 = DIRECTION ( 'NONE',  ( 1.000000000000000000, 3.773278334444166432E-23, 8.201307841325785021E-29 ) ) ;
#85880 = FACE_OUTER_BOUND ( 'NONE', #7888, .T. ) ;
#85881 = CARTESIAN_POINT ( 'NONE',  ( -13.11617634606977489, 18.14055439154125438, -1.500000000000002220 ) ) ;
#85882 = CARTESIAN_POINT ( 'NONE',  ( -79.39179774623507058, -25.27874917451760695, 6.303983963574001592 ) ) ;
#85883 = CARTESIAN_POINT ( 'NONE',  ( -120.6228709571500559, -24.91570333823100825, 8.075032458375558164 ) ) ;
#85884 = ORIENTED_EDGE ( 'NONE', *, *, #20439, .T. ) ;
#85885 = CARTESIAN_POINT ( 'NONE',  ( 32.18888049830260911, -5.126885235861809775, -11.87322522691203908 ) ) ;
#85886 = CARTESIAN_POINT ( 'NONE',  ( -35.54979913294904037, -24.15602025860895452, 10.28564288303536856 ) ) ;
#85887 = ORIENTED_EDGE ( 'NONE', *, *, #22624, .T. ) ;
#85888 = VECTOR ( 'NONE', #66806, 1000.000000000000000 ) ;
#85889 = LINE ( 'NONE', #79268, #3649 ) ;
#85890 = EDGE_LOOP ( 'NONE', ( #98870, #84984, #36810, #33024, #76004, #9031, #74248, #34645, #63007, #23149, #32093, #51100, #49212, #67613, #22093, #50223, #68171, #6236, #45026, #2915, #66985, #28026, #62522, #51289, #64303 ) ) ;
#85891 = DIRECTION ( 'NONE',  ( -0.000000000000000000, -1.000000000000000000, 0.000000000000000000 ) ) ;
#85892 = CARTESIAN_POINT ( 'NONE',  ( 18.68757921870947669, -9.911485057863893999, -1.500000000000002220 ) ) ;
#85893 = ORIENTED_EDGE ( 'NONE', *, *, #11576, .F. ) ;
#85894 = CARTESIAN_POINT ( 'NONE',  ( -50.62375377019235145, -25.00158670708910691, 2.256160236439223254 ) ) ;
#85895 = CARTESIAN_POINT ( 'NONE',  ( 18.38516380405726736, -11.72527425286322611, 11.49999999999998934 ) ) ;
#85896 = CARTESIAN_POINT ( 'NONE',  ( -60.52287095715006160, -23.47596703998600631, 11.44779298504228926 ) ) ;
#85897 = AXIS2_PLACEMENT_3D ( 'NONE', #91362, #99465, #52814 ) ;
#85898 = DIRECTION ( 'NONE',  ( -3.773278334453079618E-23, 0.9999999999976377785, 2.173523156925979975E-06 ) ) ;
#85899 = CARTESIAN_POINT ( 'NONE',  ( -75.58953762381673869, -25.00158670708909625, 2.256160236439167299 ) ) ;
#85900 = CARTESIAN_POINT ( 'NONE',  ( 21.36706796925463792, 4.321743776461201669, -1.500000000000002220 ) ) ;
#85901 = CARTESIAN_POINT ( 'NONE',  ( -30.57287095715005520, -25.29575059580470153, 5.560322743885222074 ) ) ;
#85902 = ORIENTED_EDGE ( 'NONE', *, *, #8060, .F. ) ;
#85903 = DIRECTION ( 'NONE',  ( 0.000000000000000000, 0.000000000000000000, 1.000000000000000000 ) ) ;
#85904 = LINE ( 'NONE', #62578, #92948 ) ;
#85905 = ORIENTED_EDGE ( 'NONE', *, *, #25265, .F. ) ;
#85906 = VECTOR ( 'NONE', #30993, 1000.000000000000000 ) ;
#85907 = ORIENTED_EDGE ( 'NONE', *, *, #64285, .F. ) ;
#85908 = VECTOR ( 'NONE', #60353, 1000.000000000000000 ) ;
#85909 = ORIENTED_EDGE ( 'NONE', *, *, #57924, .T. ) ;
#85910 = B_SPLINE_CURVE_WITH_KNOTS ( 'NONE', 3,
 ( #28195, #41938, #35318, #72881 ),
 .UNSPECIFIED., .F., .F.,
 ( 4, 4 ),
 ( 0.000000000000000000, 9.999999999998897304E-05 ),
 .UNSPECIFIED. ) ;
#85911 = CARTESIAN_POINT ( 'NONE',  ( -47.62287095715004881, -29.50247984919015209, -1.443849546365058689 ) ) ;
#85912 = AXIS2_PLACEMENT_3D ( 'NONE', #96584, #98065, #4744 ) ;
#85913 = CARTESIAN_POINT ( 'NONE',  ( -124.6228709571500701, -24.66019654487200086, 8.947790411086121054 ) ) ;
#85914 = CARTESIAN_POINT ( 'NONE',  ( 12.26186175617451113, -17.30295086655154080, 11.49999999999998934 ) ) ;
#85915 = CARTESIAN_POINT ( 'NONE',  ( 8.160000000000000142, -9.652339641703484574, -1.621096496867199033 ) ) ;
#85916 = CARTESIAN_POINT ( 'NONE',  ( -130.5728709571500588, -23.56000036390797092, -1.497999999999531040 ) ) ;
#85917 = EDGE_CURVE ( 'NONE', #60317, #80103, #55964, .T. ) ;
#85918 = CARTESIAN_POINT ( 'NONE',  ( 16.15056352287345121, -3.622774720514426949, -27.77856273171767398 ) ) ;
#85919 = CARTESIAN_POINT ( 'NONE',  ( -128.6228709571500417, -23.47593901973091235, -1.443836447538995760 ) ) ;
#85920 = AXIS2_PLACEMENT_3D ( 'NONE', #4689, #66612, #97522 ) ;
#85921 = CARTESIAN_POINT ( 'NONE',  ( 16.99290379607386114, -9.356058476803225332, 11.49999999999998934 ) ) ;
#85922 = EDGE_CURVE ( 'NONE', #75526, #41954, #30495, .T. ) ;
#85923 = CARTESIAN_POINT ( 'NONE',  ( -69.34449053119547557, -25.26190598939342280, 6.145922818284793365 ) ) ;
#85924 = ORIENTED_EDGE ( 'NONE', *, *, #87524, .T. ) ;
#85925 = AXIS2_PLACEMENT_3D ( 'NONE', #81079, #51127, #96303 ) ;
#85926 = CARTESIAN_POINT ( 'NONE',  ( -18.91883139384513157, -4.797682538509264738, 11.49999999999999645 ) ) ;
#85927 = CARTESIAN_POINT ( 'NONE',  ( -42.52287095715005449, -24.64965694238575011, 8.947790433994205372 ) ) ;
#85928 = CYLINDRICAL_SURFACE ( 'NONE', #34956, 84.48086791635432746 ) ;
#85929 = ORIENTED_EDGE ( 'NONE', *, *, #7730, .F. ) ;
#85930 = CARTESIAN_POINT ( 'NONE',  ( -58.62287095715004881, -24.64965695001468404, 8.947790433994185832 ) ) ;
#85931 = CARTESIAN_POINT ( 'NONE',  ( -59.52287095715004739, -24.66019654487199375, 8.947790411086128159 ) ) ;
#85932 = CARTESIAN_POINT ( 'NONE',  ( -57.62287095715004881, -29.50250243563736774, 8.947779886222145151 ) ) ;
#85933 = PLANE ( 'NONE',  #60719 ) ;
#85934 = CARTESIAN_POINT ( 'NONE',  ( 2.289404864003111051, -19.52285375609543294, -1.500000000000002220 ) ) ;
#85935 = CARTESIAN_POINT ( 'NONE',  ( -41.23075053442405391, -25.31583700235511714, 4.755616837286789966 ) ) ;
#85936 = ORIENTED_EDGE ( 'NONE', *, *, #37768, .F. ) ;
#85937 = CARTESIAN_POINT ( 'NONE',  ( 20.07693369621832602, 7.961103810760662647, -1.500000000000002220 ) ) ;
#85938 = DIRECTION ( 'NONE',  ( 0.000000000000000000, 1.020425574104004246E-16, -1.000000000000000000 ) ) ;
#85939 = CARTESIAN_POINT ( 'NONE',  ( -77.92287095715005307, -23.47593901973090169, -1.443836447538997536 ) ) ;
#85940 = CARTESIAN_POINT ( 'NONE',  ( -46.62287095715004881, -23.47593901973091235, -1.443836447539009749 ) ) ;
#85941 = PRODUCT_RELATED_PRODUCT_CATEGORY ( 'detail', '', ( #27178 ) ) ;
#85942 = B_SPLINE_CURVE_WITH_KNOTS ( 'NONE', 3,
 ( #39989, #1940, #70949, #1437 ),
 .UNSPECIFIED., .F., .F.,
 ( 4, 4 ),
 ( 0.000000000000000000, 1.000000000000000000 ),
 .UNSPECIFIED. ) ;
#85943 = COORDINATED_UNIVERSAL_TIME_OFFSET ( 0, 0, .AHEAD. ) ;
#85944 = CARTESIAN_POINT ( 'NONE',  ( -126.9228709571500247, -23.47593901973090524, -1.443836447538996204 ) ) ;
#85945 = CARTESIAN_POINT ( 'NONE',  ( 3.787259615384621192, -6.376774720514426065, 21.48076923076922640 ) ) ;
#85946 = CARTESIAN_POINT ( 'NONE',  ( -126.5895376238166961, -23.48783264082479505, -1.443836473390057051 ) ) ;
#85947 = CARTESIAN_POINT ( 'NONE',  ( -101.3308234756344035, -25.09314650408467173, 7.321823265739929809 ) ) ;
#85948 = CARTESIAN_POINT ( 'NONE',  ( -109.3646363756176783, -25.27084415602777767, 4.082054875553674300 ) ) ;
#85949 = CARTESIAN_POINT ( 'NONE',  ( -129.5218490263226272, -24.51314013834316796, 0.6176544820404223923 ) ) ;
#85950 = CARTESIAN_POINT ( 'NONE',  ( -114.5158143349167403, -24.51419770103158768, 9.386484678747160970 ) ) ;
#85951 = CARTESIAN_POINT ( 'NONE',  ( -13.91458393394894166, 14.26456941660895339, -1.500000000000002220 ) ) ;
#85952 = DIRECTION ( 'NONE',  ( 0.000000000000000000, 0.000000000000000000, 1.000000000000000000 ) ) ;
#85953 = CARTESIAN_POINT ( 'NONE',  ( -17.91562471463183570, -8.470225615102204841, -1.500000000000002220 ) ) ;
#85954 = CARTESIAN_POINT ( 'NONE',  ( 0.3376760108279234784, -5.876774720514417183, 20.09898898868105732 ) ) ;
#85955 = CARTESIAN_POINT ( 'NONE',  ( -51.62287095715005592, -24.66019654487199020, 8.947790411086135265 ) ) ;
#85956 = CARTESIAN_POINT ( 'NONE',  ( -35.62287095715007723, -24.62285846362215125, 9.038163152653519106 ) ) ;
#85957 = CARTESIAN_POINT ( 'NONE',  ( 19.63682106917175929, 6.691539877478525966, 11.49999999999999645 ) ) ;
#85958 = DIRECTION ( 'NONE',  ( -3.773278334453080206E-23, 0.9999999999976377785, 2.173523156925979975E-06 ) ) ;
#85959 = B_SPLINE_CURVE_WITH_KNOTS ( 'NONE', 3,
 ( #37150, #99529, #58511, #50893, #74705, #54889, #77691, #61997, #24424, #14799, #100020, #62497, #92925, #85827, #55389 ),
 .UNSPECIFIED., .F., .F.,
 ( 4, 1, 1, 1, 1, 1, 1, 1, 1, 1, 1, 1, 4 ),
 ( 0.000000000000000000, 0.08594794314412859682, 0.1691252118806910454, 0.2503991071860492412, 0.3322897361388358339, 0.4133642879158805905, 0.4941722833711898466, 0.5760217353866382561, 0.6607569692540066209, 0.7457831259137440716, 0.8300435929752246755, 0.9140275458206831294, 1.000000000000000000 ),
 .UNSPECIFIED. ) ;
#85960 = VECTOR ( 'NONE', #52081, 1000.000000000000114 ) ;
#85961 = CARTESIAN_POINT ( 'NONE',  ( -106.5861045487569356, -24.65952944569304250, 1.056160979905701902 ) ) ;
#85962 = CARTESIAN_POINT ( 'NONE',  ( 22.46337926046256328, 3.617889471270266277, 11.49999999999999645 ) ) ;
#85963 = VERTEX_POINT ( 'NONE', #88946 ) ;
#85964 = DIRECTION ( 'NONE',  ( 1.251281512149627050E-16, 0.000000000000000000, -1.000000000000000000 ) ) ;
#85965 = CARTESIAN_POINT ( 'NONE',  ( 27.86270917940689174, 5.965225279485572685, 29.49402280011862487 ) ) ;
#85966 = EDGE_LOOP ( 'NONE', ( #36683, #44165, #7853, #49476 ) ) ;
#85967 = CARTESIAN_POINT ( 'NONE',  ( -16.64171244834553676, 11.49637152377623828, -1.500000000000002220 ) ) ;
#85968 = DIRECTION ( 'NONE',  ( -3.773278334453079618E-23, 0.9999999999976377785, 2.173523156925979975E-06 ) ) ;
#85969 = LINE ( 'NONE', #16955, #48000 ) ;
#85970 = ORIENTED_EDGE ( 'NONE', *, *, #78573, .T. ) ;
#85971 = ORIENTED_EDGE ( 'NONE', *, *, #51542, .T. ) ;
#85972 = CARTESIAN_POINT ( 'NONE',  ( -109.5228709571500616, -29.50250243563736774, 8.947779886222136270 ) ) ;
#85973 = CARTESIAN_POINT ( 'NONE',  ( -4.681240387505234857, -22.43558246840685300, 11.49999999999998934 ) ) ;
#85974 = DIRECTION ( 'NONE',  ( 0.000000000000000000, -2.173523156925980399E-06, 0.9999999999976378895 ) ) ;
#85975 = AXIS2_PLACEMENT_3D ( 'NONE', #62478, #54367, #39125 ) ;
#85976 = CARTESIAN_POINT ( 'NONE',  ( -2.642555958445479192, -21.45212208726272607, -1.500000000000002220 ) ) ;
#85977 = EDGE_CURVE ( 'NONE', #44036, #20176, #42783, .T. ) ;
#85978 = CARTESIAN_POINT ( 'NONE',  ( -9.893913718187896222, 18.50344063021147889, 11.49999999999999645 ) ) ;
#85979 = ORIENTED_EDGE ( 'NONE', *, *, #68919, .F. ) ;
#85980 = PLANE ( 'NONE',  #12965 ) ;
#85981 = CARTESIAN_POINT ( 'NONE',  ( -124.6234875072562289, -24.65952944569305316, 1.056160979905708563 ) ) ;
#85982 = CARTESIAN_POINT ( 'NONE',  ( 2.156995527713877259, 21.93451973775924557, -1.500000000000002220 ) ) ;
#85983 = EDGE_CURVE ( 'NONE', #90358, #67210, #4210, .T. ) ;
#85985 = CARTESIAN_POINT ( 'NONE',  ( -102.5228709571500900, -23.47593901973090524, -1.443836447538996648 ) ) ;
#85984 = AXIS2_PLACEMENT_3D ( 'NONE', #89186, #57748, #50128 ) ;
#85986 = ORIENTED_EDGE ( 'NONE', *, *, #62047, .F. ) ;
#85987 = DIRECTION ( 'NONE',  ( 0.000000000000000000, 0.000000000000000000, -1.000000000000000000 ) ) ;
#85988 = CARTESIAN_POINT ( 'NONE',  ( 0.000000000000000000, -1.530000000000000027, -0.3850000000000000089 ) ) ;
#85989 = ORIENTED_EDGE ( 'NONE', *, *, #4984, .F. ) ;
#85990 = CARTESIAN_POINT ( 'NONE',  ( -123.6228709571500133, -24.33927499327853994, 9.819080762295818943 ) ) ;
#85991 = ORIENTED_EDGE ( 'NONE', *, *, #31131, .T. ) ;
#85992 = ORIENTED_EDGE ( 'NONE', *, *, #93981, .T. ) ;
#85993 = CARTESIAN_POINT ( 'NONE',  ( 10.86264265030973952, -5.965225279485574461, -28.64597719988137570 ) ) ;
#85994 = CARTESIAN_POINT ( 'NONE',  ( -83.52287095715009002, -23.95044443724993144, 10.65354141964648882 ) ) ;
#85996 = EDGE_CURVE ( 'NONE', #36722, #47188, #62071, .T. ) ;
#85995 = CARTESIAN_POINT ( 'NONE',  ( -36.49756682744079228, -24.15543982623906771, -0.2315651400026672579 ) ) ;
#85997 = CARTESIAN_POINT ( 'NONE',  ( 17.04084431845542369, 11.38269047019995206, -1.500000000000002220 ) ) ;
#85998 = ORIENTED_EDGE ( 'NONE', *, *, #13019, .T. ) ;
#85999 = CARTESIAN_POINT ( 'NONE',  ( -61.52287095715006160, -23.47596703998600631, 11.44779298504228926 ) ) ;
#86000 = CARTESIAN_POINT ( 'NONE',  ( -10.25272501932627378, 4.561466182953243909, 29.07579354015162210 ) ) ;
#86001 = CARTESIAN_POINT ( 'NONE',  ( -32.07722060962682775, -25.12026506542016335, 2.831122744435439209 ) ) ;
#86002 = CARTESIAN_POINT ( 'NONE',  ( 18.42719714020066846, 12.55551944762973626, 11.49999999999998934 ) ) ;
#86003 = CARTESIAN_POINT ( 'NONE',  ( -81.62287095715002749, -24.33832256526968862, 0.1851278514119888696 ) ) ;
#86004 = CARTESIAN_POINT ( 'NONE',  ( -90.52287095715006160, -24.99156044556202616, 7.747789690856173195 ) ) ;
#86005 = VERTEX_POINT ( 'NONE', #73715 ) ;
#86006 = CARTESIAN_POINT ( 'NONE',  ( -1.877194073982709988, 8.794404527355018431, 9.000000000000000000 ) ) ;
#86007 = CARTESIAN_POINT ( 'NONE',  ( -3.108974358974355923, -6.376774720514427841, 21.75000000000001066 ) ) ;
#86008 = CARTESIAN_POINT ( 'NONE',  ( -14.03827505669662479, 15.38897104800697591, 11.49999999999998934 ) ) ;
#86009 = EDGE_LOOP ( 'NONE', ( #75027, #80529, #18455, #80022 ) ) ;
#86011 = ORIENTED_EDGE ( 'NONE', *, *, #13538, .T. ) ;
#86010 = CARTESIAN_POINT ( 'NONE',  ( -52.52287095715006160, -24.34917612407042142, 0.1852690917480152855 ) ) ;
#86012 = VERTEX_POINT ( 'NONE', #58507 ) ;
#86013 = CARTESIAN_POINT ( 'NONE',  ( -51.38881019666819583, -25.25854471556175795, 6.651362266542584223 ) ) ;
#86014 = CARTESIAN_POINT ( 'NONE',  ( 5.724939850241691275, 20.19279902153374096, -1.500000000000002220 ) ) ;
#86015 = ORIENTED_EDGE ( 'NONE', *, *, #94194, .F. ) ;
#86016 = CARTESIAN_POINT ( 'NONE',  ( 22.81105451610979173, -1.682774720514426114, -18.46691820600746681 ) ) ;
#86017 = CARTESIAN_POINT ( 'NONE',  ( -37.52287095715006870, -24.64965694238406613, 8.947790433994205372 ) ) ;
#86018 = CARTESIAN_POINT ( 'NONE',  ( 10.22011794243639038, -5.356774720516090937, -27.02313658038265132 ) ) ;
#86019 = B_SPLINE_CURVE_WITH_KNOTS ( 'NONE', 3,
 ( #88903, #65585, #88399, #10774, #57466, #65089 ),
 .UNSPECIFIED., .F., .F.,
 ( 4, 2, 4 ),
 ( 0.000000000000000000, 0.001380764517853255106, 0.002761529035706510211 ),
 .UNSPECIFIED. ) ;
#86020 = CARTESIAN_POINT ( 'NONE',  ( -119.6228709571500559, -23.47596703998600631, 11.44779298504227860 ) ) ;
#86021 = CARTESIAN_POINT ( 'NONE',  ( -59.63756427278922700, -24.15543982623906416, -0.2315651400026668416 ) ) ;
#86022 = CARTESIAN_POINT ( 'NONE',  ( -65.62287095715008434, -24.92604778743017846, 8.074972756849355449 ) ) ;
#86024 = VERTEX_POINT ( 'NONE', #81828 ) ;
#86023 = CARTESIAN_POINT ( 'NONE',  ( 21.93305185196877360, -3.456643806985262302, 11.49999999999999645 ) ) ;
#86025 = CARTESIAN_POINT ( 'NONE',  ( -99.16166289166532977, -25.31166538673566180, 5.311370725864150266 ) ) ;
#86026 = DIRECTION ( 'NONE',  ( 0.000000000000000000, 0.000000000000000000, -1.000000000000000000 ) ) ;
#86027 = VERTEX_POINT ( 'NONE', #19920 ) ;
#86028 = CARTESIAN_POINT ( 'NONE',  ( -21.16080155796574047, 8.166215375980355518, 11.49999999999998934 ) ) ;
#86030 = EDGE_LOOP ( 'NONE', ( #84656, #23709, #20432, #57221 ) ) ;
#86029 = LINE ( 'NONE', #79413, #52252 ) ;
#86031 = ADVANCED_FACE ( 'NONE', ( #50889 ), #29078, .F. ) ;
#86032 = ORIENTED_EDGE ( 'NONE', *, *, #6420, .T. ) ;
#86033 = CARTESIAN_POINT ( 'NONE',  ( -24.90875734969025501, 6.475225279485573360, 30.00402280011862288 ) ) ;
#86034 = TOROIDAL_SURFACE ( 'NONE', #90883, 1.020000000000000018, 2.040000000000000036 ) ;
#86035 = EDGE_CURVE ( 'NONE', #90963, #82927, #37798, .T. ) ;
#86036 = CARTESIAN_POINT ( 'NONE',  ( -7.946508460909448956, -18.53024980520100939, -1.500000000000002220 ) ) ;
#86037 = CARTESIAN_POINT ( 'NONE',  ( -88.55620429048340725, -23.48783264082478794, -1.443836473390064157 ) ) ;
#86038 = ORIENTED_EDGE ( 'NONE', *, *, #171, .F. ) ;
#86039 = CARTESIAN_POINT ( 'NONE',  ( 32.45853543194704116, 5.965225279485572685, 9.169203677920338080 ) ) ;
#86040 = CARTESIAN_POINT ( 'NONE',  ( -7.019573500991415749, 21.25910006591672996, -1.500000000000002220 ) ) ;
#86041 = B_SPLINE_CURVE_WITH_KNOTS ( 'NONE', 3,
 ( #75973, #15085, #6482, #85593, #61778, #98818, #67895, #37927, #77964, #23186, #45552, #37433, #53167, #92205, #68383 ),
 .UNSPECIFIED., .F., .F.,
 ( 4, 1, 1, 1, 1, 1, 1, 1, 1, 1, 1, 1, 4 ),
 ( 0.000000000000000000, 0.08415201884431650070, 0.1665323202984589912, 0.2488363311465309202, 0.3312461454872611122, 0.4129571090216161422, 0.4904942776695665474, 0.5661557919819242279, 0.6399873346864671797, 0.7167654882718511589, 0.8021439047100994424, 0.8958332007101933447, 1.000000000000000000 ),
 .UNSPECIFIED. ) ;
#86042 = VERTEX_POINT ( 'NONE', #20911 ) ;
#86043 = VERTEX_POINT ( 'NONE', #5199 ) ;
#86044 = CARTESIAN_POINT ( 'NONE',  ( -101.5363578631102541, -25.25341111464364019, 6.270899391521124855 ) ) ;
#86045 = CARTESIAN_POINT ( 'NONE',  ( -119.6228709571500559, -23.47596703998600631, 11.44779298504227860 ) ) ;
#86046 = CARTESIAN_POINT ( 'NONE',  ( -73.62287095715005592, -24.65952944569304606, 1.056160979905698794 ) ) ;
#86047 = CARTESIAN_POINT ( 'NONE',  ( -116.5228709571500616, -23.72773821059537269, 11.05748984161097503 ) ) ;
#86048 = FACE_BOUND ( 'NONE', #20209, .T. ) ;
#86049 = VECTOR ( 'NONE', #26669, 1000.000000000000227 ) ;
#86050 = CARTESIAN_POINT ( 'NONE',  ( -18.73025074496528219, 5.678645368852136777, 11.49999999999998934 ) ) ;
#86051 = CARTESIAN_POINT ( 'NONE',  ( -5.530932042872791499, -5.876774720514408301, 19.30497968945844534 ) ) ;
#86052 = ORIENTED_EDGE ( 'NONE', *, *, #21035, .T. ) ;
#86053 = CARTESIAN_POINT ( 'NONE',  ( 20.53733210929814845, -6.371126427052321795, -1.500000000000002220 ) ) ;
#86054 = CARTESIAN_POINT ( 'NONE',  ( -19.77875734969026311, -6.143225279485574397, 27.31649921512899937 ) ) ;
#86056 = CYLINDRICAL_SURFACE ( 'NONE', #40000, 91.74549126261079834 ) ;
#86055 = B_SPLINE_CURVE_WITH_KNOTS ( 'NONE', 3,
 ( #41853, #72793, #81398, #11879, #2288, #33218 ),
 .UNSPECIFIED., .F., .F.,
 ( 4, 2, 4 ),
 ( 1.570755371633954459E-05, 0.001396183895866085585, 0.002776660238015831676 ),
 .UNSPECIFIED. ) ;
#86057 = CARTESIAN_POINT ( 'NONE',  ( -113.5228709571500616, -23.48786465467242479, 11.44779295918253936 ) ) ;
#86058 = CARTESIAN_POINT ( 'NONE',  ( -30.57287095715006231, -29.50247984919009170, -1.443849575687677245 ) ) ;
#86059 = CARTESIAN_POINT ( 'NONE',  ( -13.69284064830502423, 18.33895024417757469, -1.500000000000002220 ) ) ;
#86060 = CC_DESIGN_PERSON_AND_ORGANIZATION_ASSIGNMENT ( #65754, #50020, ( #57026 ) ) ;
#86061 = APPROVAL_DATE_TIME ( #92168, #45738 ) ;
#86062 = CARTESIAN_POINT ( 'NONE',  ( -124.5895376238167103, -24.64965694238408034, 8.947790433994649462 ) ) ;
#86063 = CARTESIAN_POINT ( 'NONE',  ( -2.702089344534958304, -5.876774720514413630, 19.72789237585158162 ) ) ;
#86064 = CARTESIAN_POINT ( 'NONE',  ( 15.05167116458888010, 13.23127732593390959, 11.49999999999999645 ) ) ;
#86065 = CARTESIAN_POINT ( 'NONE',  ( -79.55512035851637620, -25.26612423904884608, 4.736590108043814418 ) ) ;
#86066 = CYLINDRICAL_SURFACE ( 'NONE', #50110, 20.00000000000000355 ) ;
#86067 = DIRECTION ( 'NONE',  ( -0.000000000000000000, -1.000000000000000000, -0.000000000000000000 ) ) ;
#86068 = CARTESIAN_POINT ( 'NONE',  ( -38.58953762381672448, -24.64965694238406613, 8.947790433994660120 ) ) ;
#86069 = ORIENTED_EDGE ( 'NONE', *, *, #75680, .T. ) ;
#86070 = CARTESIAN_POINT ( 'NONE',  ( -6.499999999999992895, 1.999999999999999112, 0.000000000000000000 ) ) ;
#86071 = CARTESIAN_POINT ( 'NONE',  ( -21.74948284930419717, -1.071797830193938372, -1.500000000000002220 ) ) ;
#86072 = EDGE_CURVE ( 'NONE', #51831, #55337, #46241, .T. ) ;
#86073 = CARTESIAN_POINT ( 'NONE',  ( -45.52287095715006160, -23.48786465467240347, 11.44779295918255002 ) ) ;
#86074 = CARTESIAN_POINT ( 'NONE',  ( -13.08164486973500118, 14.69858247433046650, -1.500000000000002220 ) ) ;
#86075 = FACE_OUTER_BOUND ( 'NONE', #26006, .T. ) ;
#86076 = DIRECTION ( 'NONE',  ( -3.773278334444166432E-23, 1.000000000000000000, 0.000000000000000000 ) ) ;
#86077 = DIRECTION ( 'NONE',  ( -1.000000000000000000, -0.000000000000000000, -0.000000000000000000 ) ) ;
#86078 = CARTESIAN_POINT ( 'NONE',  ( -73.62287095715005592, -23.48786465467241058, 11.44779295918254469 ) ) ;
#86079 = CARTESIAN_POINT ( 'NONE',  ( -14.18348626307465743, -14.89297910716571849, 11.49999999999999645 ) ) ;
#86080 = CARTESIAN_POINT ( 'NONE',  ( 3.902919446070569176, -6.376774720514427841, 21.47497695444087284 ) ) ;
#86081 = CARTESIAN_POINT ( 'NONE',  ( 9.071512145086499501, 0.000000000000000000, 3.687490859131163923 ) ) ;
#86082 = CARTESIAN_POINT ( 'NONE',  ( 21.37280783159109276, 7.349196219051140844, 11.49999999999999645 ) ) ;
#86083 = VERTEX_POINT ( 'NONE', #75204 ) ;
#86084 =( NAMED_UNIT ( * ) PLANE_ANGLE_UNIT ( ) SI_UNIT ( $, .RADIAN. ) );
#86085 = DIRECTION ( 'NONE',  ( -3.773278334453080206E-23, 0.9999999999976377785, 2.173523156925979975E-06 ) ) ;
#86086 = CARTESIAN_POINT ( 'NONE',  ( -26.45415226839903866, -24.86235341855187286, 6.807275991248984859 ) ) ;
#86087 = CARTESIAN_POINT ( 'NONE',  ( -108.5895376238167387, -23.48783264082478794, -1.443836473390060604 ) ) ;
#86088 = FACE_OUTER_BOUND ( 'NONE', #61797, .T. ) ;
#86089 = EDGE_CURVE ( 'NONE', #27656, #64559, #5696, .T. ) ;
#86090 = B_SPLINE_CURVE_WITH_KNOTS ( 'NONE', 3,
 ( #37002, #67967, #90291, #84167, #91289, #45622 ),
 .UNSPECIFIED., .F., .F.,
 ( 4, 2, 4 ),
 ( 0.000000000000000000, 0.001380901958385389412, 0.002761803916770778824 ),
 .UNSPECIFIED. ) ;
#86091 = DIRECTION ( 'NONE',  ( 1.000000000000000000, 3.773278334444166432E-23, 8.201307841325785021E-29 ) ) ;
#86092 = DIRECTION ( 'NONE',  ( 2.168404344971008868E-16, 0.000000000000000000, 1.000000000000000000 ) ) ;
#86093 = B_SPLINE_CURVE_WITH_KNOTS ( 'NONE', 3,
 ( #28115, #4778, #3791, #58569 ),
 .UNSPECIFIED., .F., .F.,
 ( 4, 4 ),
 ( 0.000000000000000000, 9.999999999998897304E-05 ),
 .UNSPECIFIED. ) ;
#86094 = ORIENTED_EDGE ( 'NONE', *, *, #88092, .F. ) ;
#86095 = CARTESIAN_POINT ( 'NONE',  ( 22.94779996701378266, 2.684060219229261968, 11.49999999999999645 ) ) ;
#86096 = CARTESIAN_POINT ( 'NONE',  ( 20.43669262517703800, -10.12641136740851699, -1.500000000000002220 ) ) ;
#86097 = CARTESIAN_POINT ( 'NONE',  ( -74.58444882624816330, -24.51314013834315375, 0.6176544820404124003 ) ) ;
#86098 = DIRECTION ( 'NONE',  ( 0.000000000000000000, -1.000000000000000000, 0.000000000000000000 ) ) ;
#86099 = CARTESIAN_POINT ( 'NONE',  ( -71.62287095715005592, -29.50247984919015209, -1.443849546365055359 ) ) ;
#86100 = CARTESIAN_POINT ( 'NONE',  ( 18.93296920960566965, -11.98514031388154599, 11.49999999999999645 ) ) ;
#86101 = VERTEX_POINT ( 'NONE', #11322 ) ;
#86102 = DIRECTION ( 'NONE',  ( 0.000000000000000000, 0.9961946980917453232, -0.08715574274766167695 ) ) ;
#86103 = AXIS2_PLACEMENT_3D ( 'NONE', #13547, #44516, #99285 ) ;
#86104 = CARTESIAN_POINT ( 'NONE',  ( 18.54397492014093984, 11.73900455106235086, -1.500000000000002220 ) ) ;
#86105 = EDGE_CURVE ( 'NONE', #50455, #69616, #42299, .T. ) ;
#86106 = DIRECTION ( 'NONE',  ( 1.000000000000000000, 3.773278334444167020E-23, 8.201307838832447938E-29 ) ) ;
#86107 = CARTESIAN_POINT ( 'NONE',  ( -34.56115400525960979, -23.73791477778911485, 11.05961554403171299 ) ) ;
#86108 = FACE_OUTER_BOUND ( 'NONE', #87746, .T. ) ;
#86109 = ORIENTED_EDGE ( 'NONE', *, *, #25925, .T. ) ;
#86110 = CARTESIAN_POINT ( 'NONE',  ( -48.48461591879575394, -24.66019654487199730, 8.947790411086119278 ) ) ;
#86111 = PLANE ( 'NONE',  #43009 ) ;
#86112 = ORIENTED_EDGE ( 'NONE', *, *, #47191, .T. ) ;
#86113 = CARTESIAN_POINT ( 'NONE',  ( -8.751980504941329286, -18.49744413911281882, -1.500000000000002220 ) ) ;
#86114 =( BOUNDED_SURFACE ( )  B_SPLINE_SURFACE ( 3, 2, ( 
 ( #93820, #48161, #49172 ),
 ( #41045, #47661, #94315 ),
 ( #31929, #18200, #26316 ),
 ( #79086, #1487, #24801 ),
 ( #55781, #9588, #40548 ),
 ( #80097, #10582, #25306 ),
 ( #41547, #71500, #1987 ),
 ( #32929, #63906, #94819 ),
 ( #56285, #87208, #17699 ),
 ( #66398, #73001, #67381 ) ),
 .UNSPECIFIED., .F., .F., .F. ) 
 B_SPLINE_SURFACE_WITH_KNOTS ( ( 4, 2, 2, 2, 4 ),
 ( 3, 3 ),
 ( -1.454863790203986262E-16, 9.770668801556799598E-05, 0.0001954133760312814648, 0.0002931200640469949336, 0.0003908267520627084295 ),
 ( 0.000000000000000000, 1.000000000000000000 ),
 .UNSPECIFIED. ) 
 GEOMETRIC_REPRESENTATION_ITEM ( )  RATIONAL_B_SPLINE_SURFACE ( (
 ( 1.000000000000000000, 0.8096947957034197341, 1.000000000000000000),
 ( 1.000000000000000000, 0.8369431042627567541, 1.000000000000000000),
 ( 1.000000000000000000, 0.8633772427686626783, 1.000000000000000000),
 ( 1.000000000000000000, 0.9107640641016462313, 1.000000000000000000),
 ( 1.000000000000000000, 0.9319105126974177589, 1.000000000000000000),
 ( 1.000000000000000000, 0.9655776140384774164, 1.000000000000000000),
 ( 1.000000000000000000, 0.9783528158684996479, 1.000000000000000000),
 ( 1.000000000000000000, 0.9955824377509593370, 1.000000000000000000),
 ( 1.000000000000000000, 1.000024029240739631, 1.000000000000000000),
 ( 1.000000000000000000, 1.000000000000000000, 1.000000000000000000) ) ) 
 REPRESENTATION_ITEM ( '' )  SURFACE ( )  );
#86115 = ORIENTED_EDGE ( 'NONE', *, *, #3322, .F. ) ;
#86116 = EDGE_LOOP ( 'NONE', ( #76641, #47339, #50572, #78505 ) ) ;
#86117 = ORIENTED_EDGE ( 'NONE', *, *, #62652, .T. ) ;
#86118 = ORIENTED_EDGE ( 'NONE', *, *, #67137, .F. ) ;
#86119 = CARTESIAN_POINT ( 'NONE',  ( -10.12245940999746985, -20.73198382670940987, -1.500000000000002220 ) ) ;
#86121 = ADVANCED_FACE ( 'NONE', ( #34663 ), #27047, .T. ) ;
#86120 = CARTESIAN_POINT ( 'NONE',  ( -40.11625432859197815, -25.26871255744266875, 3.880430150159563940 ) ) ;
#86122 = CARTESIAN_POINT ( 'NONE',  ( 20.23811035156253979, -1.552196809741442696, -1.500000000000002220 ) ) ;
#86123 = EDGE_LOOP ( 'NONE', ( #39837, #59217, #24109, #77062 ) ) ;
#86124 = LINE ( 'NONE', #38945, #5612 ) ;
#86125 = LINE ( 'NONE', #87124, #90341 ) ;
#86127 = CARTESIAN_POINT ( 'NONE',  ( -93.62287095715008434, -24.50321055353803601, 9.387540953477522265 ) ) ;
#86126 = VECTOR ( 'NONE', #42052, 1000.000000000000114 ) ;
#86128 = CARTESIAN_POINT ( 'NONE',  ( 4.518205171808153509, -6.376774720514406525, 19.05004583296150500 ) ) ;
#86130 = VERTEX_POINT ( 'NONE', #60994 ) ;
#86129 = CARTESIAN_POINT ( 'NONE',  ( 18.54456287915894563, -10.88813254144886322, 11.49999999999999645 ) ) ;
#86131 = CARTESIAN_POINT ( 'NONE',  ( -89.62287095715004170, -24.64965695001468404, 8.947790433994180503 ) ) ;
#86132 = PLANE ( 'NONE',  #476 ) ;
#86133 = CC_DESIGN_APPROVAL ( #32096, ( #79677 ) ) ;
#86134 = ORIENTED_EDGE ( 'NONE', *, *, #28593, .F. ) ;
#86135 = CARTESIAN_POINT ( 'NONE',  ( 20.64725891757762355, 2.036748910689437864, 11.49999999999998934 ) ) ;
#86136 = ORIENTED_EDGE ( 'NONE', *, *, #60229, .T. ) ;
#86138 = ORIENTED_EDGE ( 'NONE', *, *, #74542, .T. ) ;
#86137 = CARTESIAN_POINT ( 'NONE',  ( -125.6251159883579902, -24.15503026093915295, -0.2815557561904348804 ) ) ;
#86139 = CARTESIAN_POINT ( 'NONE',  ( -41.50559876260985703, -23.96169478059712787, 10.65365249895718591 ) ) ;
#86140 = LINE ( 'NONE', #32352, #34060 ) ;
#86141 = ORIENTED_EDGE ( 'NONE', *, *, #76602, .F. ) ;
#86142 = VERTEX_POINT ( 'NONE', #60507 ) ;
#86143 = CARTESIAN_POINT ( 'NONE',  ( -49.21454750704995007, -25.12863070112381791, 7.069183623698430452 ) ) ;
#86144 = LINE ( 'NONE', #1422, #22176 ) ;
#86145 = CARTESIAN_POINT ( 'NONE',  ( -43.52945059456417454, -24.66019654487199375, 8.947790411086122830 ) ) ;
#86146 = CARTESIAN_POINT ( 'NONE',  ( 16.78392297789021015, 14.29496084597832883, 11.49999999999999645 ) ) ;
#86147 = B_SPLINE_CURVE_WITH_KNOTS ( 'NONE', 3,
 ( #32143, #7304, #45888, #23516 ),
 .UNSPECIFIED., .F., .F.,
 ( 4, 4 ),
 ( 0.000000000000000000, 9.999999999998897304E-05 ),
 .UNSPECIFIED. ) ;
#86148 = CARTESIAN_POINT ( 'NONE',  ( -89.63827055049355863, -23.73791477778911840, 11.05961554403170233 ) ) ;
#86149 = CARTESIAN_POINT ( 'NONE',  ( 2.010693963185784749, 22.50221635003889276, -1.500000000000002220 ) ) ;
#86150 = CARTESIAN_POINT ( 'NONE',  ( -11.62490142266122639, -17.50836435561060256, -1.500000000000002220 ) ) ;
#86151 = CARTESIAN_POINT ( 'NONE',  ( -100.6814946224345988, -25.30604030395771531, 4.890060448994407061 ) ) ;
#86153 = EDGE_LOOP ( 'NONE', ( #25298, #55338, #9914, #9612 ) ) ;
#86152 = DIRECTION ( 'NONE',  ( 1.000000000000000000, 3.491481338843133355E-15, 2.352173255807796056E-16 ) ) ;
#86154 = VERTEX_POINT ( 'NONE', #23915 ) ;
#86155 = CARTESIAN_POINT ( 'NONE',  ( 26.73860345374794178, 1.477225279485574028, 19.84760796525321425 ) ) ;
#86156 = EDGE_CURVE ( 'NONE', #13329, #1499, #12682, .T. ) ;
#86157 = AXIS2_PLACEMENT_3D ( 'NONE', #65972, #95890, #96892 ) ;
#86158 = DIRECTION ( 'NONE',  ( -0.000000000000000000, 1.000000000000000000, -0.000000000000000000 ) ) ;
#86159 = ORIENTED_EDGE ( 'NONE', *, *, #11527, .F. ) ;
#86160 = CARTESIAN_POINT ( 'NONE',  ( 6.139388171429570384, 20.22809724653347985, -1.500000000000002220 ) ) ;
#86161 = CARTESIAN_POINT ( 'NONE',  ( -66.62287095715005592, -23.47596703998600276, 11.44779298504227683 ) ) ;
#86162 = FACE_OUTER_BOUND ( 'NONE', #99138, .T. ) ;
#86163 = CARTESIAN_POINT ( 'NONE',  ( -121.6267039608711400, -23.73766607897670156, -1.055555164236450905 ) ) ;
#86164 = CARTESIAN_POINT ( 'NONE',  ( -109.5562042904833788, -24.66019654487200086, 8.947790411086124607 ) ) ;
#86165 = DIRECTION ( 'NONE',  ( 0.000000000000000000, -1.000000000000000000, 0.000000000000000000 ) ) ;
#86166 = CARTESIAN_POINT ( 'NONE',  ( 12.24756355222007898, 18.56953561607567238, -1.500000000000002220 ) ) ;
#86167 = CARTESIAN_POINT ( 'NONE',  ( -49.32147450118114307, -25.13941415244942945, 7.186702086172223503 ) ) ;
#86168 = ORIENTED_EDGE ( 'NONE', *, *, #97665, .T. ) ;
#86169 = LINE ( 'NONE', #61351, #69182 ) ;
#86170 = CARTESIAN_POINT ( 'NONE',  ( -37.64193424478225580, -24.15543982623907127, -0.2315651400026566831 ) ) ;
#86171 = CARTESIAN_POINT ( 'NONE',  ( -126.5566007190337956, -23.48783264082477018, -1.443836473390087249 ) ) ;
#86172 = CYLINDRICAL_SURFACE ( 'NONE', #2590, 129.7684398600581517 ) ;
#86173 = CARTESIAN_POINT ( 'NONE',  ( -39.52287095715006870, -24.64965694238406613, 8.947790433994205372 ) ) ;
#86174 = B_SPLINE_CURVE_WITH_KNOTS ( 'NONE', 3,
 ( #70194, #39237, #40746, #85919 ),
 .UNSPECIFIED., .F., .F.,
 ( 4, 4 ),
 ( 0.000000000000000000, 1.000000000000000000 ),
 .UNSPECIFIED. ) ;
#86175 = CARTESIAN_POINT ( 'NONE',  ( 12.63578256557813795, 14.83599306707809085, -1.500000000000002220 ) ) ;
#86176 = B_SPLINE_CURVE_WITH_KNOTS ( 'NONE', 3,
 ( #37583, #30965, #77127, #22 ),
 .UNSPECIFIED., .F., .F.,
 ( 4, 4 ),
 ( 0.9094323928107194144, 0.9104331398514848850 ),
 .UNSPECIFIED. ) ;
#86177 = CARTESIAN_POINT ( 'NONE',  ( -21.38522110535750542, 1.317000383210971792, 11.49999999999998934 ) ) ;
#86178 = DIRECTION ( 'NONE',  ( 0.000000000000000000, 1.000000000000000000, 0.000000000000000000 ) ) ;
#86179 = CARTESIAN_POINT ( 'NONE',  ( -60.52841940773001284, -25.00182538069856619, 7.747789668514392325 ) ) ;
#86180 = VECTOR ( 'NONE', #98929, 1000.000000000000114 ) ;
#86181 = CARTESIAN_POINT ( 'NONE',  ( -100.6228709571500843, -24.92604778743017846, 8.074972756849359001 ) ) ;
#86182 = FACE_OUTER_BOUND ( 'NONE', #81407, .T. ) ;
#86183 = CARTESIAN_POINT ( 'NONE',  ( 22.03932947713327906, 5.445304565557160359, -1.500000000000002220 ) ) ;
#86184 = ADVANCED_FACE ( 'NONE', ( #46767 ), #23396, .F. ) ;
#86185 = EDGE_CURVE ( 'NONE', #33250, #32160, #53384, .T. ) ;
#86186 = DIRECTION ( 'NONE',  ( -0.000000000000000000, -1.000000000000000000, -0.000000000000000000 ) ) ;
#86187 = CARTESIAN_POINT ( 'NONE',  ( -72.62287095715005592, -23.47593901973091235, -1.443836447539006196 ) ) ;
#86188 = CARTESIAN_POINT ( 'NONE',  ( -9.044204435542846809, 17.70297415775587169, 11.49999999999999645 ) ) ;
#86189 = CARTESIAN_POINT ( 'NONE',  ( -118.6228709571500701, -23.47596703998600631, 11.44779298504227683 ) ) ;
#86190 = CARTESIAN_POINT ( 'NONE',  ( -89.81226385320381667, -25.18330262851202050, 6.757888827294434186 ) ) ;
#86191 = DIRECTION ( 'NONE',  ( 0.5709972981045763341, 1.784358049357977499E-06, -0.8209519386383650197 ) ) ;
#86192 = ORIENTED_EDGE ( 'NONE', *, *, #85300, .F. ) ;
#86193 = DIRECTION ( 'NONE',  ( -1.000000000000000000, 0.000000000000000000, 0.000000000000000000 ) ) ;
#86194 = CARTESIAN_POINT ( 'NONE',  ( -58.52287095715009713, -24.66019654487199730, 8.947790411086121054 ) ) ;
#86195 = CARTESIAN_POINT ( 'NONE',  ( -51.69439593370608321, -25.27412447326236489, 3.842802143524250091 ) ) ;
#86196 = CARTESIAN_POINT ( 'NONE',  ( -2.787017431591729988, -21.48445716988565835, 11.49999999999998934 ) ) ;
#86197 = EDGE_CURVE ( 'NONE', #10968, #57696, #92425, .T. ) ;
#86198 = CARTESIAN_POINT ( 'NONE',  ( -56.54231419305688888, -24.35071581493543391, 9.817618358456030592 ) ) ;
#86199 = CARTESIAN_POINT ( 'NONE',  ( -18.70048401425367501, 5.426029767813830063, -1.500000000000002220 ) ) ;
#86200 = EDGE_CURVE ( 'NONE', #27315, #95233, #83819, .T. ) ;
#86201 = CARTESIAN_POINT ( 'NONE',  ( -55.62855437941350090, -24.83644354573578283, 8.397322867130093016 ) ) ;
#86202 = VECTOR ( 'NONE', #36617, 1000.000000000000000 ) ;
#86203 = ORIENTED_EDGE ( 'NONE', *, *, #71358, .T. ) ;
#86205 = ADVANCED_FACE ( 'NONE', ( #45269 ), #61993, .T. ) ;
#86204 = APPROVAL_PERSON_ORGANIZATION ( #66254, #100233, #84437 ) ;
#86206 = CARTESIAN_POINT ( 'NONE',  ( -2.495337616714382367, -20.20711602426958819, 11.49999999999999645 ) ) ;
#86207 = FACE_OUTER_BOUND ( 'NONE', #87933, .T. ) ;
#86208 = CARTESIAN_POINT ( 'NONE',  ( 5.184553252003285984, 6.475225279485573360, -28.06387035751381731 ) ) ;
#86209 = ORIENTED_EDGE ( 'NONE', *, *, #33286, .F. ) ;
#86210 = CARTESIAN_POINT ( 'NONE',  ( -0.1182468871973336583, -21.51920112203868740, 11.01174216661999949 ) ) ;
#86211 = CARTESIAN_POINT ( 'NONE',  ( -95.52287095715006160, -23.47596703998600631, 11.44779298504228215 ) ) ;
#86212 = CARTESIAN_POINT ( 'NONE',  ( -96.62287095715007013, -23.95044443724992433, 10.65354141964649592 ) ) ;
#86213 = CARTESIAN_POINT ( 'NONE',  ( 10.54059822343757880, -5.876774720514426953, 23.12308057603841149 ) ) ;
#86214 = CARTESIAN_POINT ( 'NONE',  ( -89.81226385320383088, -29.50249591506787894, 5.947779886229223045 ) ) ;
#86215 = CARTESIAN_POINT ( 'NONE',  ( 17.77915467781788195, 9.360003092772107181, 11.49999999999998934 ) ) ;
#86216 = EDGE_CURVE ( 'NONE', #17029, #83268, #87395, .T. ) ;
#86217 = LINE ( 'NONE', #61894, #71095 ) ;
#86218 = ORIENTED_EDGE ( 'NONE', *, *, #71690, .T. ) ;
#86219 = CARTESIAN_POINT ( 'NONE',  ( -28.32169924589829080, -5.965225279485592225, -8.244178532169447848 ) ) ;
#86220 = CARTESIAN_POINT ( 'NONE',  ( -19.87571804785047647, -11.42512898079034400, 11.49999999999999645 ) ) ;
#86221 = CARTESIAN_POINT ( 'NONE',  ( 9.518656604726816184, -20.62229310799655124, -1.500000000000002220 ) ) ;
#86222 = ORIENTED_EDGE ( 'NONE', *, *, #5388, .T. ) ;
#86223 = CARTESIAN_POINT ( 'NONE',  ( -30.47287095715006444, -25.24888046561066091, 6.123886400242147587 ) ) ;
#86224 = DIRECTION ( 'NONE',  ( 0.000000000000000000, 0.000000000000000000, 1.000000000000000000 ) ) ;
#86225 = FACE_OUTER_BOUND ( 'NONE', #16385, .T. ) ;
#86226 = CARTESIAN_POINT ( 'NONE',  ( -30.57287095715006231, -25.11786545954479877, 2.750328999548155462 ) ) ;
#86227 = EDGE_CURVE ( 'NONE', #58432, #60030, #69243, .T. ) ;
#86228 = CARTESIAN_POINT ( 'NONE',  ( -84.52287095715006160, -23.48786465467241769, 11.44779295918254469 ) ) ;
#86229 = VECTOR ( 'NONE', #419, 1000.000000000000114 ) ;
#86230 = EDGE_CURVE ( 'NONE', #95068, #47734, #43548, .T. ) ;
#86231 = CARTESIAN_POINT ( 'NONE',  ( -33.52287095715006160, -23.47596703998600631, 11.44779298504229459 ) ) ;
#86232 = CARTESIAN_POINT ( 'NONE',  ( -99.09705801370142808, -25.25460571337453075, 5.399822423257166548 ) ) ;
#86233 = ORIENTED_EDGE ( 'NONE', *, *, #28886, .T. ) ;
#86234 = CARTESIAN_POINT ( 'NONE',  ( 20.11976772532220181, -3.360927329567881205, -1.500000000000002220 ) ) ;
#86235 = EDGE_LOOP ( 'NONE', ( #61676, #21965, #73341, #15613 ) ) ;
#86236 = CARTESIAN_POINT ( 'NONE',  ( 9.898807498884217182, 20.75630955806377287, 11.49999999999998934 ) ) ;
#86238 = EDGE_CURVE ( 'NONE', #15126, #64588, #71776, .T. ) ;
#86237 = CARTESIAN_POINT ( 'NONE',  ( -1.438454482798693146, -5.876774720514409189, 19.55848054040323092 ) ) ;
#86239 = ORIENTED_EDGE ( 'NONE', *, *, #17580, .F. ) ;
#86240 = CARTESIAN_POINT ( 'NONE',  ( -108.5552593049708889, -23.96169478059714564, 10.65365249895716993 ) ) ;
#86241 = EDGE_CURVE ( 'NONE', #64814, #96161, #20893, .T. ) ;
#86242 = EDGE_CURVE ( 'NONE', #24998, #23703, #21899, .T. ) ;
#86243 = DIRECTION ( 'NONE',  ( 1.000000000000000000, 0.000000000000000000, 0.000000000000000000 ) ) ;
#86245 = ORIENTED_EDGE ( 'NONE', *, *, #99840, .F. ) ;
#86244 = CARTESIAN_POINT ( 'NONE',  ( -12.43717309395686499, -17.31322327496724611, 11.49999999999999645 ) ) ;
#86246 = AXIS2_PLACEMENT_3D ( 'NONE', #73967, #48653, #65881 ) ;
#86247 = ORIENTED_EDGE ( 'NONE', *, *, #4256, .T. ) ;
#86248 = CARTESIAN_POINT ( 'NONE',  ( 2.725811458822067657, 22.07344620009914138, 11.49999999999998934 ) ) ;
#86249 = VECTOR ( 'NONE', #48675, 1000.000000000000000 ) ;
#86250 = CARTESIAN_POINT ( 'NONE',  ( 17.27521350410721368, -11.31798593588896829, 11.49999999999998934 ) ) ;
#86251 = B_SPLINE_CURVE_WITH_KNOTS ( 'NONE', 3,
 ( #24004, #54972, #10794, #2194, #34140, #55985, #10290, #1687 ),
 .UNSPECIFIED., .F., .F.,
 ( 4, 2, 2, 4 ),
 ( 3.992453237073820429E-05, 0.003307229636718544714, 0.004940882188892447430, 0.006574534741066350579 ),
 .UNSPECIFIED. ) ;
#86252 = B_SPLINE_CURVE_WITH_KNOTS ( 'NONE', 3,
 ( #37848, #76393, #52579, #6895, #68802, #61207, #7385, #23601, #79400, #48969 ),
 .UNSPECIFIED., .F., .F.,
 ( 4, 2, 2, 2, 4 ),
 ( 0.000000000000000000, 0.0003937058646109520060, 0.0007874117292219040120, 0.001181117593832857644, 0.001574823458443811493 ),
 .UNSPECIFIED. ) ;
#86253 = ORIENTED_EDGE ( 'NONE', *, *, #59173, .T. ) ;
#86254 = CARTESIAN_POINT ( 'NONE',  ( -5.023036858974361252, -5.876774720514410077, 19.14743589743590846 ) ) ;
#86255 = CARTESIAN_POINT ( 'NONE',  ( -69.85540018123268169, -25.31392322340849432, 5.203679841770401104 ) ) ;
#86256 = ORIENTED_EDGE ( 'NONE', *, *, #88764, .F. ) ;
#86257 = CARTESIAN_POINT ( 'NONE',  ( -112.5228709571500616, -23.47593901973090524, -1.443836447538996426 ) ) ;
#86258 = EDGE_LOOP ( 'NONE', ( #6514, #33490, #38283, #1267, #78605, #89753, #16700, #3885 ) ) ;
#86259 = CARTESIAN_POINT ( 'NONE',  ( -58.64947410562866281, -23.73791477778911840, 11.05961554403170766 ) ) ;
#86260 = CARTESIAN_POINT ( 'NONE',  ( -11.44352472427880052, 17.46665840655709090, -1.500000000000002220 ) ) ;
#86261 = CARTESIAN_POINT ( 'NONE',  ( 19.95399986947220583, -8.914707708046476498, 11.49999999999999645 ) ) ;
#86262 = CARTESIAN_POINT ( 'NONE',  ( 25.03841014571435508, -5.082747618816810586, -9.367571460246121973 ) ) ;
#86263 = CARTESIAN_POINT ( 'NONE',  ( 33.00535138976592719, 3.570691370340881576, -12.97242311383975988 ) ) ;
#86264 = CARTESIAN_POINT ( 'NONE',  ( 17.87336509531889561, -13.68139028912531785, -1.500000000000002220 ) ) ;
#86265 = CARTESIAN_POINT ( 'NONE',  ( -44.62287095715004881, -24.64898659630528854, 1.056161002820819261 ) ) ;
#86266 = CARTESIAN_POINT ( 'NONE',  ( 30.32108885906865936, -4.540774720514427543, 3.274824222184972822 ) ) ;
#86267 = AXIS2_PLACEMENT_3D ( 'NONE', #10191, #54873, #72105 ) ;
#86268 = CARTESIAN_POINT ( 'NONE',  ( 4.332134589405623792, -5.876774720514426953, 21.69242924468134959 ) ) ;
#86269 = ORIENTED_EDGE ( 'NONE', *, *, #13084, .T. ) ;
#86270 = LOCAL_TIME ( 0, 54, 15.00000000000000000, #30021 ) ;
#86271 = ORIENTED_EDGE ( 'NONE', *, *, #28014, .T. ) ;
#86272 = ORIENTED_EDGE ( 'NONE', *, *, #31566, .F. ) ;
#86273 = ORIENTED_EDGE ( 'NONE', *, *, #24907, .T. ) ;
#86274 = CARTESIAN_POINT ( 'NONE',  ( -19.34459864454321831, 9.218434461607088792, -1.500000000000002220 ) ) ;
#86275 = CARTESIAN_POINT ( 'NONE',  ( -21.90463088927077706, -4.570550247397807908, 11.49999999999999645 ) ) ;
#86276 = ORIENTED_EDGE ( 'NONE', *, *, #91461, .F. ) ;
#86277 = CARTESIAN_POINT ( 'NONE',  ( 0.4554788648648982474, -21.05657754196055009, 11.49999999999998934 ) ) ;
#86278 = CARTESIAN_POINT ( 'NONE',  ( -30.48114189052184031, -24.75335575484455219, 8.640462295247351321 ) ) ;
#86279 = CARTESIAN_POINT ( 'NONE',  ( -18.20579941527595480, -8.200869797747142087, -1.500000000000002220 ) ) ;
#86280 = PLANE ( 'NONE',  #24204 ) ;
#86281 = CARTESIAN_POINT ( 'NONE',  ( -43.52287095715005449, -24.51387760970724017, 9.387446482453409402 ) ) ;
#86282 = CARTESIAN_POINT ( 'NONE',  ( -2.093881351098874521, -21.91542971883435698, -1.500000000000002220 ) ) ;
#86283 = FACE_OUTER_BOUND ( 'NONE', #85739, .T. ) ;
#86284 = AXIS2_PLACEMENT_3D ( 'NONE', #48846, #47334, #79771 ) ;
#86285 = ORIENTED_EDGE ( 'NONE', *, *, #40262, .T. ) ;
#86286 = CARTESIAN_POINT ( 'NONE',  ( -72.52287095715007581, -29.50250243563736774, 8.947779886222143375 ) ) ;
#86287 = LINE ( 'NONE', #71075, #4448 ) ;
#86288 = CARTESIAN_POINT ( 'NONE',  ( 15.94631523246878579, 13.42178585792578360, 11.49999999999999645 ) ) ;
#86289 = FACE_OUTER_BOUND ( 'NONE', #95502, .T. ) ;
#86290 = DIRECTION ( 'NONE',  ( 0.000000000000000000, 1.084202172485504434E-16, -1.000000000000000000 ) ) ;
#86291 = DIRECTION ( 'NONE',  ( -1.000000000000000000, 8.503546450866701308E-16, 0.000000000000000000 ) ) ;
#86292 = CARTESIAN_POINT ( 'NONE',  ( -19.99249555334884221, 7.427959064407942513, 11.49999999999998934 ) ) ;
#86293 = DIRECTION ( 'NONE',  ( -3.773278334444166432E-23, 1.000000000000000000, 0.000000000000000000 ) ) ;
#86294 = CARTESIAN_POINT ( 'NONE',  ( 30.53060340732262645, 5.330559497946674163, 2.122526108692961877 ) ) ;
#86295 = CARTESIAN_POINT ( 'NONE',  ( -109.9161100070499515, -25.06732983082694588, 7.447789526168954843 ) ) ;
#86296 = CARTESIAN_POINT ( 'NONE',  ( -5.568927889719891944, -5.876774720514417183, 20.14881673916291760 ) ) ;
#86297 = CARTESIAN_POINT ( 'NONE',  ( 5.070899574700155732, -21.93562493352797915, -1.500000000000002220 ) ) ;
#86298 = VECTOR ( 'NONE', #46996, 1000.000000000000114 ) ;
#86299 = ADVANCED_FACE ( 'NONE', ( #14297 ), #76195, .T. ) ;
#86300 = DIRECTION ( 'NONE',  ( 1.000000000000000000, 0.000000000000000000, -2.504262461560503878E-15 ) ) ;
#86301 = ORIENTED_EDGE ( 'NONE', *, *, #96714, .F. ) ;
#86302 = EDGE_CURVE ( 'NONE', #94426, #32090, #31028, .T. ) ;
#86303 = CYLINDRICAL_SURFACE ( 'NONE', #70939, 1.000000000000000000 ) ;
#86304 = CARTESIAN_POINT ( 'NONE',  ( 2.905472630834636139, -6.376774720514415407, 19.87563926270137671 ) ) ;
#86305 = CARTESIAN_POINT ( 'NONE',  ( -2.223759785643201869, -19.53228827767608777, 11.49999999999999645 ) ) ;
#86306 = CARTESIAN_POINT ( 'NONE',  ( -49.52287095715004028, -23.94994826722564696, -0.6494450866342753592 ) ) ;
#86307 = CARTESIAN_POINT ( 'NONE',  ( -32.52287095715004028, -24.35013146730201683, 9.818937971375111928 ) ) ;
#86308 = VERTEX_POINT ( 'NONE', #14795 ) ;
#86309 = ADVANCED_FACE ( 'NONE', ( #85311 ), #15802, .T. ) ;
#86310 = CARTESIAN_POINT ( 'NONE',  ( -99.51176673733515088, -24.34968618360934300, 0.1864209137778966852 ) ) ;
#86311 = CARTESIAN_POINT ( 'NONE',  ( -55.62287095715004170, -24.99132157543083821, 2.256160258750667502 ) ) ;
#86312 = CARTESIAN_POINT ( 'NONE',  ( -124.5211384108013846, -23.96169478059714564, 10.65365249895717170 ) ) ;
#86313 = EDGE_CURVE ( 'NONE', #29681, #4993, #57768, .T. ) ;
#86314 = EDGE_CURVE ( 'NONE', #89470, #62448, #48790, .T. ) ;
#86315 = DIRECTION ( 'NONE',  ( -0.000000000000000000, 0.000000000000000000, -1.000000000000000000 ) ) ;
#86316 = CARTESIAN_POINT ( 'NONE',  ( 3.912202881759007767, 19.34271161525698091, 11.49999999999998934 ) ) ;
#86317 = ORIENTED_EDGE ( 'NONE', *, *, #33171, .T. ) ;
#86318 = VECTOR ( 'NONE', #14796, 1000.000000000000114 ) ;
#86319 = EDGE_CURVE ( 'NONE', #31094, #87031, #229, .T. ) ;
#86320 = CARTESIAN_POINT ( 'NONE',  ( 12.43249465596513126, -15.92577207200969092, 11.49999999999999645 ) ) ;
#86321 = CARTESIAN_POINT ( 'NONE',  ( 8.817327481845893544, 6.376774720514678307, -28.08864864928871086 ) ) ;
#86322 = B_SPLINE_CURVE_WITH_KNOTS ( 'NONE', 3,
 ( #66333, #19125, #65346, #64848, #42496, #57712 ),
 .UNSPECIFIED., .F., .F.,
 ( 4, 2, 4 ),
 ( 1.570887131794795405E-05, 0.001396322306279762808, 0.002776935741241577573 ),
 .UNSPECIFIED. ) ;
#86323 = PERSON_AND_ORGANIZATION ( #70597, #27821 ) ;
#86324 = ORIENTED_EDGE ( 'NONE', *, *, #9471, .F. ) ;
#86325 = CARTESIAN_POINT ( 'NONE',  ( -128.5228709571500758, -29.50250243563736774, 8.947779886222132717 ) ) ;
#86326 = LINE ( 'NONE', #39646, #41012 ) ;
#86327 = CARTESIAN_POINT ( 'NONE',  ( -50.92646440412053011, -25.30193528779874512, 5.303687469111972419 ) ) ;
#86328 = CARTESIAN_POINT ( 'NONE',  ( -1.967852706420949005, -5.876774720514409189, 19.18381548539530357 ) ) ;
#86329 = FACE_OUTER_BOUND ( 'NONE', #90435, .T. ) ;
#86330 = PLANE ( 'NONE',  #41370 ) ;
#86331 = CARTESIAN_POINT ( 'NONE',  ( -19.32702923155483177, -5.217993511516596961, -1.500000000000002220 ) ) ;
#86332 = EDGE_CURVE ( 'NONE', #33445, #98946, #27305, .T. ) ;
#86333 = B_SPLINE_CURVE_WITH_KNOTS ( 'NONE', 3,
 ( #89922, #20391, #60489, #20895, #50375, #19404 ),
 .UNSPECIFIED., .F., .F.,
 ( 4, 2, 4 ),
 ( 0.000000000000000000, 0.001380901958385393966, 0.002761803916770787931 ),
 .UNSPECIFIED. ) ;
#86334 = CARTESIAN_POINT ( 'NONE',  ( 2.246611357655419638, -0.1632191352058106892, -0.1632191352058112721 ) ) ;
#86335 = LINE ( 'NONE', #50654, #4729 ) ;
#86336 = VERTEX_POINT ( 'NONE', #18681 ) ;
#86337 = AXIS2_PLACEMENT_3D ( 'NONE', #69349, #64136, #76941 ) ;
#86338 = ADVANCED_FACE ( 'NONE', ( #97316 ), #54885, .F. ) ;
#86340 = CARTESIAN_POINT ( 'NONE',  ( -92.52287095715006160, -24.64965694238407323, 8.947790433994196491 ) ) ;
#86339 = LOCAL_TIME ( 0, 54, 15.00000000000000000, #75954 ) ;
#86341 = CARTESIAN_POINT ( 'NONE',  ( -109.5174377349821953, -25.18430242849744261, 3.703579253892022471 ) ) ;
#86342 = CARTESIAN_POINT ( 'NONE',  ( -20.27875734969026311, -4.543225279485573864, 22.85402280011862430 ) ) ;
#86343 = PLANE ( 'NONE',  #75930 ) ;
#86344 = CARTESIAN_POINT ( 'NONE',  ( -41.26959558397307148, -25.08918874615346439, 7.338714959427068862 ) ) ;
#86345 = DIRECTION ( 'NONE',  ( -1.000000000000000000, 0.000000000000000000, 0.000000000000000000 ) ) ;
#86346 = EDGE_CURVE ( 'NONE', #95277, #8989, #96994, .T. ) ;
#86347 = CARTESIAN_POINT ( 'NONE',  ( -19.80875734969026425, 5.965225279485572685, 30.51402280011862089 ) ) ;
#86348 = AXIS2_PLACEMENT_3D ( 'NONE', #86696, #40540, #54766 ) ;
#86349 = CARTESIAN_POINT ( 'NONE',  ( -99.90552080552691905, -25.31392319263090585, 5.203681702801228326 ) ) ;
#86350 = ORIENTED_EDGE ( 'NONE', *, *, #66405, .T. ) ;
#86351 = CARTESIAN_POINT ( 'NONE',  ( -12.35269427871797987, -16.12754648828645543, -1.500000000000002220 ) ) ;
#86352 = CIRCLE ( 'NONE', #81514, 21.89999999999999858 ) ;
#86353 = CARTESIAN_POINT ( 'NONE',  ( -109.5562042904833646, -23.48783264082478439, -1.443836473390060604 ) ) ;
#86354 = CARTESIAN_POINT ( 'NONE',  ( -100.5228709571500616, -29.50248528299804818, 1.056150453629042030 ) ) ;
#86356 = ORIENTED_EDGE ( 'NONE', *, *, #39227, .T. ) ;
#86355 = ADVANCED_FACE ( 'NONE', ( #19675 ), #56776, .F. ) ;
#86357 = CARTESIAN_POINT ( 'NONE',  ( -94.62287095715005592, -23.47596703998600631, 11.44779298504227860 ) ) ;
#86358 = CARTESIAN_POINT ( 'NONE',  ( -20.08517628505838815, -1.856936949192496300, -1.500000000000002220 ) ) ;
#86359 = CARTESIAN_POINT ( 'NONE',  ( 3.428800225705347149, -20.88102749682517612, 11.49999999999999645 ) ) ;
#86360 = CARTESIAN_POINT ( 'NONE',  ( 19.81268554055766273, 9.900562300003143079, -1.500000000000002220 ) ) ;
#86361 = ADVANCED_FACE ( 'NONE', ( #81091 ), #78194, .T. ) ;
#86362 = CARTESIAN_POINT ( 'NONE',  ( -10.41206725544052780, -17.73373708237225799, 11.49999999999998934 ) ) ;
#86363 = CARTESIAN_POINT ( 'NONE',  ( 7.164812103570541879, -5.876774720514421624, 20.85668272347560404 ) ) ;
#86364 = ORIENTED_EDGE ( 'NONE', *, *, #85269, .F. ) ;
#86365 = CARTESIAN_POINT ( 'NONE',  ( -43.52287095715006870, -24.50216790748204332, 0.6166512839542462876 ) ) ;
#86366 = ORIENTED_EDGE ( 'NONE', *, *, #74322, .T. ) ;
#86367 = CARTESIAN_POINT ( 'NONE',  ( -88.58953762381669605, -24.64965694238575011, 8.947790433994194714 ) ) ;
#86368 = CARTESIAN_POINT ( 'NONE',  ( -23.29179552176161749, 5.965225279485594001, -17.29637630388738501 ) ) ;
#86369 = VERTEX_POINT ( 'NONE', #8707 ) ;
#86370 = VERTEX_POINT ( 'NONE', #33922 ) ;
#86371 = EDGE_LOOP ( 'NONE', ( #91452, #79121, #57467, #77981 ) ) ;
#86372 = FACE_OUTER_BOUND ( 'NONE', #93988, .T. ) ;
#86373 = CARTESIAN_POINT ( 'NONE',  ( 7.165897526731081157, -5.876774720514419847, 20.76279523443833597 ) ) ;
#86374 = FACE_OUTER_BOUND ( 'NONE', #8655, .T. ) ;
#86375 = CARTESIAN_POINT ( 'NONE',  ( -2.856624844580134770, 20.53689577262001364, -1.500000000000002220 ) ) ;
#86376 = CARTESIAN_POINT ( 'NONE',  ( -20.21959982808627032, -7.803091810188320210, 11.49999999999999645 ) ) ;
#86377 = VERTEX_POINT ( 'NONE', #73982 ) ;
#86378 = AXIS2_PLACEMENT_3D ( 'NONE', #19990, #97611, #12371 ) ;
#86379 = CARTESIAN_POINT ( 'NONE',  ( -46.58953762381671737, -24.64965694238406968, 8.947790433994658343 ) ) ;
#86380 = CARTESIAN_POINT ( 'NONE',  ( -111.2237262587288598, -25.16193699626175118, 3.138289488163724439 ) ) ;
#86381 = CARTESIAN_POINT ( 'NONE',  ( -21.90463088927077706, -4.570550247397807908, -1.500000000000002220 ) ) ;
#86382 = CARTESIAN_POINT ( 'NONE',  ( -71.52287095715010423, -23.48783264082477018, -1.443836473390091246 ) ) ;
#86383 = CARTESIAN_POINT ( 'NONE',  ( -84.58539173471375250, -24.51314013834316441, 0.6176544820404183955 ) ) ;
#86384 = ORIENTED_EDGE ( 'NONE', *, *, #66085, .F. ) ;
#86385 = B_SPLINE_CURVE_WITH_KNOTS ( 'NONE', 3,
 ( #19512, #44366, #73315, #67209 ),
 .UNSPECIFIED., .F., .F.,
 ( 4, 4 ),
 ( 0.7002859815557139767, 0.7092924128278295104 ),
 .UNSPECIFIED. ) ;
#86386 = CARTESIAN_POINT ( 'NONE',  ( -119.4728709571500644, -25.40558663563398056, 5.000950440326719537 ) ) ;
#86387 = CARTESIAN_POINT ( 'NONE',  ( -35.64141604588792944, -24.52399227489126687, 9.353111116836519301 ) ) ;
#86388 = VECTOR ( 'NONE', #8834, 1000.000000000000227 ) ;
#86389 = ORIENTED_EDGE ( 'NONE', *, *, #47851, .T. ) ;
#86390 = CARTESIAN_POINT ( 'NONE',  ( -102.5228709571500758, -29.50250243563736774, 8.947779886222138046 ) ) ;
#86391 = EDGE_LOOP ( 'NONE', ( #93465, #4483, #2901, #30090 ) ) ;
#86392 = CARTESIAN_POINT ( 'NONE',  ( -112.6228709571500559, -29.50250243563736774, 8.947779886222136270 ) ) ;
#86393 = CARTESIAN_POINT ( 'NONE',  ( 17.87031378931267867, -11.31994873005049129, -1.500000000000002220 ) ) ;
#86394 = ORIENTED_EDGE ( 'NONE', *, *, #61276, .T. ) ;
#86395 = CARTESIAN_POINT ( 'NONE',  ( -50.62611295517817211, -24.92564183028979130, 1.928384488918255535 ) ) ;
#86396 = CARTESIAN_POINT ( 'NONE',  ( -3.204121956075930200, -21.57847171274271858, -1.500000000000002220 ) ) ;
#86397 = CARTESIAN_POINT ( 'NONE',  ( -90.62287095715004170, -29.50248789122583659, 2.256150453626215580 ) ) ;
#86398 = CARTESIAN_POINT ( 'NONE',  ( -62.62287095715004881, -24.66019654487199020, 8.947790411086131712 ) ) ;
#86399 = PLANE ( 'NONE',  #35193 ) ;
#86400 = CARTESIAN_POINT ( 'NONE',  ( -11.04117723084791614, -18.81814233335528286, -1.500000000000002220 ) ) ;
#86401 = CARTESIAN_POINT ( 'NONE',  ( -30.57287095715007297, -25.09900243522883301, 2.757825582299280764 ) ) ;
#86402 = EDGE_LOOP ( 'NONE', ( #36725, #85971, #21207, #78697 ) ) ;
#86403 = FACE_OUTER_BOUND ( 'NONE', #47673, .T. ) ;
#86404 = CARTESIAN_POINT ( 'NONE',  ( -85.62828315695789172, -24.73531770709095312, 8.716586749053508498 ) ) ;
#86405 = ORIENTED_EDGE ( 'NONE', *, *, #64042, .F. ) ;
#86406 = CARTESIAN_POINT ( 'NONE',  ( -129.5558062447522047, -24.35071581493544102, 9.817618358456021710 ) ) ;
#86407 = VERTEX_POINT ( 'NONE', #4479 ) ;
#86408 = CIRCLE ( 'NONE', #2119, 0.8160000000000007248 ) ;
#86409 = EDGE_LOOP ( 'NONE', ( #86985, #63781, #71962, #28031 ) ) ;
#86410 = CARTESIAN_POINT ( 'NONE',  ( -29.23542772204989859, -25.18830698421514924, 4.359319682132476004 ) ) ;
#86411 = CARTESIAN_POINT ( 'NONE',  ( -82.55857439284859822, -23.73766607897671577, -1.055555164236435362 ) ) ;
#86412 = CARTESIAN_POINT ( 'NONE',  ( 18.67678363807796416, 10.12720680154768971, 11.49999999999998934 ) ) ;
#86413 = CARTESIAN_POINT ( 'NONE',  ( -125.5895376238167245, -23.47593901973091235, -1.443836447538995760 ) ) ;
#86414 = CARTESIAN_POINT ( 'NONE',  ( -41.58953762381673158, -24.65952944569304250, 1.056160979905689024 ) ) ;
#86415 = DIRECTION ( 'NONE',  ( -3.445208383210904608E-15, 0.9940716917543757081, -0.1087265912856350686 ) ) ;
#86416 = DIRECTION ( 'NONE',  ( -0.000000000000000000, -1.000000000000000000, -0.000000000000000000 ) ) ;
#86418 = CARTESIAN_POINT ( 'NONE',  ( 14.52268490272241408, 12.84546865777419455, -1.500000000000002220 ) ) ;
#86417 = AXIS2_PLACEMENT_3D ( 'NONE', #13028, #90169, #61232 ) ;
#86419 = CARTESIAN_POINT ( 'NONE',  ( -45.49986917282443244, -24.15503026093915651, -0.2815557561904415418 ) ) ;
#86420 = ORIENTED_EDGE ( 'NONE', *, *, #36592, .F. ) ;
#86421 = EDGE_CURVE ( 'NONE', #55779, #20587, #82351, .T. ) ;
#86422 = CARTESIAN_POINT ( 'NONE',  ( -8.292788067677484776, 17.68049324621676632, 11.49999999999999645 ) ) ;
#86423 = PLANE ( 'NONE',  #64938 ) ;
#86424 = ADVANCED_FACE ( 'NONE', ( #34421 ), #64401, .T. ) ;
#86425 = DIRECTION ( 'NONE',  ( -1.000000000000000000, 0.000000000000000000, -0.000000000000000000 ) ) ;
#86426 = ORIENTED_EDGE ( 'NONE', *, *, #85622, .F. ) ;
#86427 = ADVANCED_FACE ( 'NONE', ( #72993 ), #72491, .F. ) ;
#86428 = CARTESIAN_POINT ( 'NONE',  ( -98.52287095715009002, -24.66019654487200441, 8.947790411086119278 ) ) ;
#86429 = CARTESIAN_POINT ( 'NONE',  ( -75.62287095715004170, -24.15431212366389957, -0.2830839119429070516 ) ) ;
#86430 = EDGE_CURVE ( 'NONE', #81257, #54341, #57283, .T. ) ;
#86431 = FACE_OUTER_BOUND ( 'NONE', #42294, .T. ) ;
#86432 = PLANE ( 'NONE',  #76902 ) ;
#86433 = CARTESIAN_POINT ( 'NONE',  ( -19.15055961920884542, -4.482958728538418924, -1.500000000000002220 ) ) ;
#86434 = B_SPLINE_SURFACE_WITH_KNOTS ( 'NONE', 3, 3, ( 
 ( #44113, #37492, #67452, #52722 ),
 ( #22245, #98377, #28881, #75536 ),
 ( #30373, #22745, #83659, #59845 ),
 ( #29875, #38493, #98883, #21252 ),
 ( #13640, #69443, #51726, #29374 ),
 ( #100361, #61843, #60351, #84156 ),
 ( #84660, #76532, #44610, #20754 ) ),
 .UNSPECIFIED., .F., .F., .F.,
 ( 4, 3, 4 ),
 ( 4, 4 ),
 ( 0.7945040050992245861, 0.8970133687736503436, 0.9995227324480759901 ),
 ( 0.4696133325002398995, 0.4708428617326421151 ),
 .UNSPECIFIED. ) ;
#86435 = ORIENTED_EDGE ( 'NONE', *, *, #76715, .F. ) ;
#86436 = CARTESIAN_POINT ( 'NONE',  ( -18.50814150397365410, 11.09706937414969374, 11.49999999999998934 ) ) ;
#86437 = CARTESIAN_POINT ( 'NONE',  ( -97.58953762381675290, -23.47596703998600631, 11.44779298504227683 ) ) ;
#86438 = CARTESIAN_POINT ( 'NONE',  ( 3.509873074917118085, -5.965225279485572685, 29.15869884040363758 ) ) ;
#86439 = CARTESIAN_POINT ( 'NONE',  ( 16.03631736716203449, -16.64276770305488284, -1.500000000000002220 ) ) ;
#86440 = CALENDAR_DATE ( 2026, 9, 10 ) ;
#86441 = CARTESIAN_POINT ( 'NONE',  ( 3.557932825399831689, -6.376774720514429617, 21.44518044978141091 ) ) ;
#86442 = CARTESIAN_POINT ( 'NONE',  ( -103.6228709571500559, -29.50250243563736774, 8.947779886222138046 ) ) ;
#86443 = CARTESIAN_POINT ( 'NONE',  ( -126.6228709571500275, -23.48783264082479505, -1.443836473390057051 ) ) ;
#86444 = LINE ( 'NONE', #9308, #41855 ) ;
#86445 = CARTESIAN_POINT ( 'NONE',  ( -111.7494854843401555, -25.10921632119354641, 4.020187994209829974 ) ) ;
#86446 = DIRECTION ( 'NONE',  ( 0.000000000000000000, -2.173523156925979552E-06, 0.9999999999976378895 ) ) ;
#86447 = CARTESIAN_POINT ( 'NONE',  ( -114.5904428896033522, -24.15620529776629155, 10.23563542870659404 ) ) ;
#86448 = CARTESIAN_POINT ( 'NONE',  ( -15.73602684802347440, -12.20685706852216867, -1.500000000000002220 ) ) ;
#86449 = AXIS2_PLACEMENT_3D ( 'NONE', #51349, #27012, #66602 ) ;
#86450 = CARTESIAN_POINT ( 'NONE',  ( -75.63150933904543649, -24.63419186844611275, 9.035850630976923981 ) ) ;
#86451 = CARTESIAN_POINT ( 'NONE',  ( 19.75055111929153639, -1.948201398878238066, -1.500000000000002220 ) ) ;
#86452 = ORIENTED_EDGE ( 'NONE', *, *, #95999, .F. ) ;
#86453 = CARTESIAN_POINT ( 'NONE',  ( -0.001774553997815280816, -5.876774720514414518, 19.59623724171353487 ) ) ;
#86454 = VECTOR ( 'NONE', #35335, 1000.000000000000114 ) ;
#86455 = CARTESIAN_POINT ( 'NONE',  ( 8.500000000000000000, -0.9000000000000000222, -3.750000000000000000 ) ) ;
#86456 = LINE ( 'NONE', #93057, #57300 ) ;
#86457 = CARTESIAN_POINT ( 'NONE',  ( -1.843323519027639357, -20.62917239659568835, 11.49999999999999645 ) ) ;
#86458 = CARTESIAN_POINT ( 'NONE',  ( 0.000000000000000000, -4.056774720514426669, 0.000000000000000000 ) ) ;
#86459 = CARTESIAN_POINT ( 'NONE',  ( -106.5500360596543317, -24.51314013834316441, 0.6176544820404206160 ) ) ;
#86460 = CARTESIAN_POINT ( 'NONE',  ( -9.230423729802735622, -20.81519635545753033, 11.49999999999999645 ) ) ;
#86461 = ORIENTED_EDGE ( 'NONE', *, *, #62098, .F. ) ;
#86462 = CARTESIAN_POINT ( 'NONE',  ( -69.51085230579893448, -23.96119346886880663, -0.6495511937832122440 ) ) ;
#86463 = CARTESIAN_POINT ( 'NONE',  ( -100.5562042904834072, -25.00158670708909625, 2.256160236439166411 ) ) ;
#86464 = ORIENTED_EDGE ( 'NONE', *, *, #14244, .T. ) ;
#86465 = CARTESIAN_POINT ( 'NONE',  ( -5.148175472751820081, -19.54457232503198227, 11.49999999999998934 ) ) ;
#86466 = CARTESIAN_POINT ( 'NONE',  ( 9.021150247049412485, -0.9126213611645739299, -3.707288619710387145 ) ) ;
#86467 = B_SPLINE_CURVE_WITH_KNOTS ( 'NONE', 3,
 ( #58176, #58666, #89120, #89614 ),
 .UNSPECIFIED., .F., .F.,
 ( 4, 4 ),
 ( 0.1688795826442255343, 0.1698803296849912270 ),
 .UNSPECIFIED. ) ;
#86468 = DIRECTION ( 'NONE',  ( 0.000000000000000000, -0.9513357669802769978, 0.3081562241202474572 ) ) ;
#86469 = EDGE_CURVE ( 'NONE', #97847, #19743, #50152, .T. ) ;
#86470 = ORIENTED_EDGE ( 'NONE', *, *, #16424, .F. ) ;
#86471 = CARTESIAN_POINT ( 'NONE',  ( -40.62287095715005592, -23.48786465467240347, 11.44779295918255180 ) ) ;
#86472 = CARTESIAN_POINT ( 'NONE',  ( 7.457602374657920308, -21.66695214233757838, 11.49999999999998934 ) ) ;
#86473 = CARTESIAN_POINT ( 'NONE',  ( -13.89275734969026388, -0.3587747205144262708, 30.51402280011862089 ) ) ;
#86474 = CARTESIAN_POINT ( 'NONE',  ( -19.63739455291241498, 3.909132673056371132, -1.500000000000002220 ) ) ;
#86475 = CARTESIAN_POINT ( 'NONE',  ( -36.62287095715005592, -24.50321055353804667, 9.387540953477540029 ) ) ;
#86476 = CARTESIAN_POINT ( 'NONE',  ( 20.89173079421859214, 1.537965369061287557, 11.49999999999999645 ) ) ;
#86477 = CARTESIAN_POINT ( 'NONE',  ( -122.6228709571500417, -23.73934037231758154, 11.05740245334328264 ) ) ;
#86478 = CARTESIAN_POINT ( 'NONE',  ( -124.5548839462270365, -24.34968618360934300, 0.1864209137778899961 ) ) ;
#86479 = CARTESIAN_POINT ( 'NONE',  ( -5.411813039392390223, -21.34095290059367755, -1.500000000000002220 ) ) ;
#86480 = EDGE_CURVE ( 'NONE', #89504, #39568, #75348, .T. ) ;
#86481 = CARTESIAN_POINT ( 'NONE',  ( -0.7395115731254252589, 18.09566585216508727, -9.000000000000000000 ) ) ;
#86482 = AXIS2_PLACEMENT_3D ( 'NONE', #69463, #67980, #53251 ) ;
#86483 = VERTEX_POINT ( 'NONE', #5953 ) ;
#86484 = FACE_OUTER_BOUND ( 'NONE', #76615, .T. ) ;
#86485 = ADVANCED_FACE ( 'NONE', ( #97804 ), #89707, .T. ) ;
#86486 = FACE_BOUND ( 'NONE', #86702, .T. ) ;
#86487 = ORIENTED_EDGE ( 'NONE', *, *, #81067, .T. ) ;
#86488 = CARTESIAN_POINT ( 'NONE',  ( 2.677564053859940341, -6.376774720514406525, 19.16116138973293559 ) ) ;
#86489 = ORIENTED_EDGE ( 'NONE', *, *, #63537, .F. ) ;
#86490 = VECTOR ( 'NONE', #51506, 1000.000000000000114 ) ;
#86491 = VERTEX_POINT ( 'NONE', #27800 ) ;
#86492 = DIRECTION ( 'NONE',  ( 0.9951627101165076983, 0.000000000000000000, 0.09824042138329622254 ) ) ;
#86493 = CARTESIAN_POINT ( 'NONE',  ( -69.52287095715006160, -29.50247984919015209, -1.443849546365055359 ) ) ;
#86494 = CARTESIAN_POINT ( 'NONE',  ( -4.177535645411178500, -5.876774720514415407, 20.17598923696320767 ) ) ;
#86495 = CARTESIAN_POINT ( 'NONE',  ( 13.18781518674367348, -15.76626393773247337, -1.500000000000002220 ) ) ;
#86496 = ORIENTED_EDGE ( 'NONE', *, *, #42707, .T. ) ;
#86497 = DIRECTION ( 'NONE',  ( 0.000000000000000000, 0.000000000000000000, -1.000000000000000000 ) ) ;
#86498 = DIRECTION ( 'NONE',  ( 0.9975640502598241977, -0.06975647374412546897, 0.000000000000000000 ) ) ;
#86499 = PLANE ( 'NONE',  #74204 ) ;
#86500 = CARTESIAN_POINT ( 'NONE',  ( -17.00426676922356606, 14.40147940013276973, 11.49999999999998934 ) ) ;
#86501 = DIRECTION ( 'NONE',  ( -3.773278334453079030E-23, 0.9999999999976377785, 2.173523156925979128E-06 ) ) ;
#86502 = DIRECTION ( 'NONE',  ( 1.000000000000000000, 3.773278334444166432E-23, 8.201307841325785021E-29 ) ) ;
#86503 = ORIENTED_EDGE ( 'NONE', *, *, #26743, .T. ) ;
#86504 = CARTESIAN_POINT ( 'NONE',  ( -96.62287095714999907, -24.51283580621364067, 0.6167428607019872500 ) ) ;
#86505 = CARTESIAN_POINT ( 'NONE',  ( -124.6228709571500275, -23.72747288104469732, -1.053458166803224794 ) ) ;
#86506 = CARTESIAN_POINT ( 'NONE',  ( -14.03827505669662479, 15.38897104800697591, -1.500000000000002220 ) ) ;
#86507 = ORIENTED_EDGE ( 'NONE', *, *, #21233, .T. ) ;
#86509 = ORIENTED_EDGE ( 'NONE', *, *, #58112, .T. ) ;
#86508 = CARTESIAN_POINT ( 'NONE',  ( -3.749999999999999556, 26.59999999999999432, 2.100000000000000089 ) ) ;
#86510 = ORIENTED_EDGE ( 'NONE', *, *, #79972, .T. ) ;
#86511 = B_SPLINE_CURVE_WITH_KNOTS ( 'NONE', 3,
 ( #3836, #95174, #96667, #66247 ),
 .UNSPECIFIED., .F., .F.,
 ( 4, 4 ),
 ( 0.000000000000000000, 9.999999999998897304E-05 ),
 .UNSPECIFIED. ) ;
#86512 = CARTESIAN_POINT ( 'NONE',  ( -103.6228709571500559, -23.47593901973091235, -1.443836447539001089 ) ) ;
#86513 = CARTESIAN_POINT ( 'NONE',  ( -20.39251343623233836, 4.912230638944180328, -1.500000000000002220 ) ) ;
#86514 = EDGE_LOOP ( 'NONE', ( #15310, #44891, #30466, #54872 ) ) ;
#86515 = DIRECTION ( 'NONE',  ( -0.000000000000000000, 1.000000000000000000, -0.000000000000000000 ) ) ;
#86516 = CARTESIAN_POINT ( 'NONE',  ( 5.101312121039179637, -3.305285905532577839, -27.56070534847060571 ) ) ;
#86517 = CARTESIAN_POINT ( 'NONE',  ( 10.77631500667670572, -5.356774720514423827, -24.99100794736120434 ) ) ;
#86518 = PLANE ( 'NONE',  #42054 ) ;
#86519 = CARTESIAN_POINT ( 'NONE',  ( -59.65599814963717051, -23.48783264082476308, -1.443836473390097908 ) ) ;
#86520 = CARTESIAN_POINT ( 'NONE',  ( 8.349999999999972999, 27.69999999999999574, 2.100000000000000089 ) ) ;
#86521 = CARTESIAN_POINT ( 'NONE',  ( -57.52287095715003318, -23.48783264082476663, -1.443836473390093911 ) ) ;
#86523 = ORIENTED_EDGE ( 'NONE', *, *, #17447, .T. ) ;
#86522 = CARTESIAN_POINT ( 'NONE',  ( -18.24902840909259538, -12.68162010772806170, 11.49999999999999645 ) ) ;
#86524 = DIRECTION ( 'NONE',  ( 0.1478094111296165691, -0.9890158633619158257, 0.000000000000000000 ) ) ;
#86525 = CARTESIAN_POINT ( 'NONE',  ( 26.73860345374794178, -1.477225279485574028, 19.84760796525321780 ) ) ;
#86526 = VERTEX_POINT ( 'NONE', #98800 ) ;
#86527 = VECTOR ( 'NONE', #54176, 1000.000000000000114 ) ;
#86528 = CARTESIAN_POINT ( 'NONE',  ( -7.311831771877058905, -21.45741656709679646, 11.49999999999998934 ) ) ;
#86529 = EDGE_CURVE ( 'NONE', #92377, #53767, #17314, .T. ) ;
#86531 = ORIENTED_EDGE ( 'NONE', *, *, #63940, .F. ) ;
#86530 = CARTESIAN_POINT ( 'NONE',  ( 0.3000000000000007661, 0.000000000000000000, 0.000000000000000000 ) ) ;
#86532 = VECTOR ( 'NONE', #60674, 1000.000000000000000 ) ;
#86533 = ORIENTED_EDGE ( 'NONE', *, *, #53326, .T. ) ;
#86534 = CARTESIAN_POINT ( 'NONE',  ( 31.27821779315964790, -4.116118814799345493, -3.972734673865978117 ) ) ;
#86535 = CARTESIAN_POINT ( 'NONE',  ( -6.497366621441947210, -19.08602653180391329, -1.500000000000002220 ) ) ;
#86536 = DIRECTION ( 'NONE',  ( -1.000000000000000000, -3.491481338843133355E-15, -2.352173255807796056E-16 ) ) ;
#86537 = ORIENTED_EDGE ( 'NONE', *, *, #1770, .T. ) ;
#86538 = ADVANCED_FACE ( 'NONE', ( #13061 ), #67373, .T. ) ;
#86539 = CARTESIAN_POINT ( 'NONE',  ( -55.62287095715004170, -29.50248789122583659, 2.256150453626215580 ) ) ;
#86540 = CARTESIAN_POINT ( 'NONE',  ( 17.95543856985664277, -13.40637504462900331, -1.500000000000002220 ) ) ;
#86541 = ORIENTED_EDGE ( 'NONE', *, *, #97089, .T. ) ;
#86542 = ORIENTED_EDGE ( 'NONE', *, *, #46224, .F. ) ;
#86543 = CARTESIAN_POINT ( 'NONE',  ( -112.5150097671653810, -24.51419770103158413, 9.386484678747166299 ) ) ;
#86544 = CARTESIAN_POINT ( 'NONE',  ( -94.55479201150613733, -23.96169478059713143, 10.65365249895717881 ) ) ;
#86545 = EDGE_CURVE ( 'NONE', #66209, #72281, #90197, .T. ) ;
#86546 = DIRECTION ( 'NONE',  ( -1.000000000000000000, 0.000000000000000000, 0.000000000000000000 ) ) ;
#86547 = DIRECTION ( 'NONE',  ( -0.9951627101165076983, -0.09824042138329588947, -3.430045979798635096E-16 ) ) ;
#86548 = EDGE_CURVE ( 'NONE', #46432, #11836, #13560, .T. ) ;
#86549 = CARTESIAN_POINT ( 'NONE',  ( -58.52287095715006160, -23.48786465467241058, 11.44779295918254824 ) ) ;
#86550 = CARTESIAN_POINT ( 'NONE',  ( -19.37596289572233488, 2.755671585415585767, 11.49999999999998934 ) ) ;
#86551 = EDGE_CURVE ( 'NONE', #35049, #50718, #66881, .T. ) ;
#86552 = DIRECTION ( 'NONE',  ( -0.000000000000000000, -1.000000000000000000, -0.000000000000000000 ) ) ;
#86553 = ORIENTED_EDGE ( 'NONE', *, *, #22365, .F. ) ;
#86554 = CARTESIAN_POINT ( 'NONE',  ( 14.19067371521932230, 16.14321034643037578, 11.49999999999998934 ) ) ;
#86555 = B_SPLINE_CURVE_WITH_KNOTS ( 'NONE', 3,
 ( #86968, #25065, #8346, #39294, #95089, #9342 ),
 .UNSPECIFIED., .F., .F.,
 ( 4, 2, 4 ),
 ( 6.384118678619663671E-06, 0.001386860460828381273, 0.002767336802978143193 ),
 .UNSPECIFIED. ) ;
#86556 = CARTESIAN_POINT ( 'NONE',  ( -128.5896665593298849, -24.34968618360935011, 0.1864209137779018477 ) ) ;
#86557 = ADVANCED_FACE ( 'NONE', ( #36908 ), #83360, .T. ) ;
#86558 = CARTESIAN_POINT ( 'NONE',  ( -121.5228709571500332, -24.51283580621365488, 0.6167428607019768139 ) ) ;
#86559 = LINE ( 'NONE', #7427, #68682 ) ;
#86560 = CARTESIAN_POINT ( 'NONE',  ( -70.52287095715007581, -25.00182538069145366, 7.747789668545101094 ) ) ;
#86561 = CARTESIAN_POINT ( 'NONE',  ( -8.048360580058307789, -21.46040670285860230, -1.500000000000002220 ) ) ;
#86562 = DATE_AND_TIME ( #88573, #42408 ) ;
#86563 = CARTESIAN_POINT ( 'NONE',  ( 5.271800844963591359, -3.316774720514426456, -28.56638892015329034 ) ) ;
#86564 = LINE ( 'NONE', #87063, #26434 ) ;
#86565 = CARTESIAN_POINT ( 'NONE',  ( 18.22975119132022215, -8.346483668847822557, 11.49999999999999645 ) ) ;
#86566 = CARTESIAN_POINT ( 'NONE',  ( 15.14080536460164517, -5.152774720514427642, -26.62908960815038384 ) ) ;
#86567 = CARTESIAN_POINT ( 'NONE',  ( -57.55620429048338593, -24.66019654487199020, 8.947790411086131712 ) ) ;
#86568 = CARTESIAN_POINT ( 'NONE',  ( -8.749999999999767297, 18.74999999999999645, 2.100000000000000089 ) ) ;
#86569 = LINE ( 'NONE', #48020, #99048 ) ;
#86570 = ADVANCED_FACE ( 'NONE', ( #35912 ), #37418, .T. ) ;
#86571 = LINE ( 'NONE', #24166, #798 ) ;
#86572 = CARTESIAN_POINT ( 'NONE',  ( 14.05712878599199200, -16.60762996970646199, -1.500000000000002220 ) ) ;
#86573 = CARTESIAN_POINT ( 'NONE',  ( -28.98875734969026396, 0.3587747205144265483, 10.11402280011862587 ) ) ;
#86574 = CARTESIAN_POINT ( 'NONE',  ( 0.6594449095415070294, 19.62168050102039629, -1.500000000000002220 ) ) ;
#86575 = CARTESIAN_POINT ( 'NONE',  ( -85.52287095715006160, -24.63345952396255356, 9.038047939301506517 ) ) ;
#86576 = CARTESIAN_POINT ( 'NONE',  ( -40.76736580419878919, -25.19037098555834575, 3.332599596532740183 ) ) ;
#86577 = DIRECTION ( 'NONE',  ( 0.000000000000000000, 0.000000000000000000, -1.000000000000000000 ) ) ;
#86578 = CARTESIAN_POINT ( 'NONE',  ( 2.627412086454235851, -5.876774720514420736, 20.59155478446653831 ) ) ;
#86579 = CARTESIAN_POINT ( 'NONE',  ( 11.80677006232881254, 16.86875346446678137, 11.49999999999999645 ) ) ;
#86580 = FACE_OUTER_BOUND ( 'NONE', #6106, .T. ) ;
#86581 = VECTOR ( 'NONE', #74480, 1000.000000000000114 ) ;
#86582 = DIRECTION ( 'NONE',  ( -1.000000000000000000, 0.000000000000000000, 0.000000000000000000 ) ) ;
#86583 = CARTESIAN_POINT ( 'NONE',  ( 7.090404290683943067, 21.45231405096426514, 11.49999999999999645 ) ) ;
#86584 = ORIENTED_EDGE ( 'NONE', *, *, #5346, .T. ) ;
#86585 = CARTESIAN_POINT ( 'NONE',  ( -70.29041810236439858, -25.12219144531777459, 7.100646716122134272 ) ) ;
#86586 = CARTESIAN_POINT ( 'NONE',  ( -27.30354941466529439, -24.79259182970212549, 7.548671802243905660 ) ) ;
#86587 = CARTESIAN_POINT ( 'NONE',  ( -125.6234888013038926, -25.00182538069147498, 7.747789668545045139 ) ) ;
#86588 = CARTESIAN_POINT ( 'NONE',  ( 15.13694198098060717, -3.544954394834232581, -27.27417057618865570 ) ) ;
#86589 = EDGE_CURVE ( 'NONE', #24503, #54649, #45532, .T. ) ;
#86590 = LINE ( 'NONE', #46044, #100237 ) ;
#86591 = VECTOR ( 'NONE', #31844, 1000.000000000000114 ) ;
#86592 = LINE ( 'NONE', #95710, #23636 ) ;
#86593 = EDGE_CURVE ( 'NONE', #36415, #25694, #45037, .T. ) ;
#86594 = VERTEX_POINT ( 'NONE', #37909 ) ;
#86595 = CARTESIAN_POINT ( 'NONE',  ( 23.08992502549420323, -0.8469403905869224980, 11.49999999999999645 ) ) ;
#86596 = CARTESIAN_POINT ( 'NONE',  ( 22.28265747778879202, 5.072132558558076099, 11.49999999999998934 ) ) ;
#86597 = CARTESIAN_POINT ( 'NONE',  ( 4.214857194124448370, -5.876774720514402972, 18.65898740197609840 ) ) ;
#86598 = CARTESIAN_POINT ( 'NONE',  ( -96.58459391463640031, -24.65952944569305316, 1.056160979905706121 ) ) ;
#86599 = CARTESIAN_POINT ( 'NONE',  ( -63.57960293449288258, -24.66019654487200086, 8.947790411086121054 ) ) ;
#86600 = CARTESIAN_POINT ( 'NONE',  ( 19.77452139984142221, -10.64395493966388706, 11.49999999999999645 ) ) ;
#86601 = ORIENTED_EDGE ( 'NONE', *, *, #71716, .F. ) ;
#86602 = DIRECTION ( 'NONE',  ( 1.000000000000000000, 3.773278334444166432E-23, 8.201307841325785021E-29 ) ) ;
#86603 = CARTESIAN_POINT ( 'NONE',  ( -21.09739860443290382, 5.981408608369527258, -1.500000000000002220 ) ) ;
#86604 = EDGE_CURVE ( 'NONE', #70027, #15603, #76452, .T. ) ;
#86605 = DIRECTION ( 'NONE',  ( -3.773278334444166432E-23, 1.000000000000000000, 0.000000000000000000 ) ) ;
#86606 = B_SPLINE_CURVE_WITH_KNOTS ( 'NONE', 3,
 ( #90985, #52434, #44825, #75746, #6246, #1142, #84366, #7237, #8753, #55435, #84866, #93470, #93977, #61553, #24469, #8251, #22452, #53437, #7744 ),
 .UNSPECIFIED., .F., .F.,
 ( 4, 1, 1, 1, 1, 1, 1, 1, 1, 1, 1, 1, 1, 1, 1, 1, 4 ),
 ( 0.000000000000000000, 0.06867706841303485021, 0.1368709585090958636, 0.2061143571452989376, 0.2775381819697280150, 0.3497719775548984722, 0.4212508361555684644, 0.4929107569233693309, 0.5670265889927383895, 0.6066141532413351634, 0.6497039535189884640, 0.6973031504846843864, 0.7490856597091365421, 0.8048806474593092064, 0.8654850057023351084, 0.9302371271531362229, 1.000000000000000000 ),
 .UNSPECIFIED. ) ;
#86607 = CARTESIAN_POINT ( 'NONE',  ( -110.6228709571500559, -25.00158670708909625, 2.256160236439165967 ) ) ;
#86608 = CARTESIAN_POINT ( 'NONE',  ( -0.02075734969026423599, -6.475225279485573360, -0.08597719988137648983 ) ) ;
#86609 = ORIENTED_EDGE ( 'NONE', *, *, #84526, .F. ) ;
#86610 = CARTESIAN_POINT ( 'NONE',  ( -48.56040166396459057, -23.73791477778911840, 11.05961554403170766 ) ) ;
#86611 = ADVANCED_FACE ( 'NONE', ( #51646 ), #75252, .T. ) ;
#86612 = DIRECTION ( 'NONE',  ( -1.000000000000000000, -3.773278334444167608E-23, -8.201307833595939069E-29 ) ) ;
#86613 = ORIENTED_EDGE ( 'NONE', *, *, #98007, .F. ) ;
#86614 = CARTESIAN_POINT ( 'NONE',  ( -15.03541999946025243, -13.88573836563254460, -1.500000000000002220 ) ) ;
#86615 = ORIENTED_EDGE ( 'NONE', *, *, #90243, .F. ) ;
#86616 = EDGE_LOOP ( 'NONE', ( #13374, #95852, #58669, #9478 ) ) ;
#86617 = ORIENTED_EDGE ( 'NONE', *, *, #13901, .T. ) ;
#86618 = ORIENTED_EDGE ( 'NONE', *, *, #5340, .F. ) ;
#86619 = CARTESIAN_POINT ( 'NONE',  ( 20.31487730549432413, -11.01532776123576518, -1.500000000000002220 ) ) ;
#86620 = CARTESIAN_POINT ( 'NONE',  ( -77.62287095715005592, -29.50247984919015209, -1.443849546365053582 ) ) ;
#86621 = CARTESIAN_POINT ( 'NONE',  ( 5.347689060783223702, 19.56899250667117229, -1.500000000000002220 ) ) ;
#86622 = EDGE_CURVE ( 'NONE', #90525, #12265, #15064, .T. ) ;
#86623 = ORIENTED_EDGE ( 'NONE', *, *, #98696, .F. ) ;
#86624 = CARTESIAN_POINT ( 'NONE',  ( -6.741682653110981249, 5.965225279485572685, 30.62569541381301619 ) ) ;
#86625 = CARTESIAN_POINT ( 'NONE',  ( -72.52287095715007581, -24.33832256527048798, 0.1851278514138591791 ) ) ;
#86626 = CARTESIAN_POINT ( 'NONE',  ( -101.4434582987268811, -25.22066056363861719, 6.520318706290999522 ) ) ;
#86627 = CARTESIAN_POINT ( 'NONE',  ( -98.22287095715006444, -23.47596703998600276, 11.44779298504227683 ) ) ;
#86629 = ORIENTED_EDGE ( 'NONE', *, *, #40743, .F. ) ;
#86628 = CARTESIAN_POINT ( 'NONE',  ( -8.581294335678165908, -19.67629172487136557, 11.49999999999999645 ) ) ;
#86630 = CARTESIAN_POINT ( 'NONE',  ( -6.660000000000001030, -10.15233964170348457, 0.003711184059992174607 ) ) ;
#86631 = CARTESIAN_POINT ( 'NONE',  ( -49.46456330771200527, -25.26385804535316026, 4.758318182142605934 ) ) ;
#86632 = AXIS2_PLACEMENT_3D ( 'NONE', #54141, #52132, #14046 ) ;
#86633 = EDGE_LOOP ( 'NONE', ( #65567, #22799 ) ) ;
#86634 = CARTESIAN_POINT ( 'NONE',  ( 14.12806351585482112, -15.20395780304818523, -1.500000000000002220 ) ) ;
#86635 = ORIENTED_EDGE ( 'NONE', *, *, #99166, .F. ) ;
#86636 = CC_DESIGN_PERSON_AND_ORGANIZATION_ASSIGNMENT ( #12796, #20403, ( #97564 ) ) ;
#86638 = ORIENTED_EDGE ( 'NONE', *, *, #99760, .T. ) ;
#86637 = LINE ( 'NONE', #71423, #71810 ) ;
#86639 = CARTESIAN_POINT ( 'NONE',  ( -111.6235230997591685, -24.66019654487200441, 8.947790411086105067 ) ) ;
#86640 = CARTESIAN_POINT ( 'NONE',  ( -102.6228709571500559, -23.47596703998600631, 11.44779298504227683 ) ) ;
#86641 = EDGE_LOOP ( 'NONE', ( #45945, #59891, #99817, #51808 ) ) ;
#86642 = ORIENTED_EDGE ( 'NONE', *, *, #40504, .F. ) ;
#86643 = CARTESIAN_POINT ( 'NONE',  ( -28.58953762381671382, -24.50475509704323329, 8.947790423985489738 ) ) ;
#86644 = CARTESIAN_POINT ( 'NONE',  ( -0.02075734969026423599, 3.316774720514426456, -0.08597719988137648983 ) ) ;
#86645 = CARTESIAN_POINT ( 'NONE',  ( -29.78642357706881683, -25.22946142887256826, 4.201050309516873860 ) ) ;
#86647 = ORIENTED_EDGE ( 'NONE', *, *, #88047, .T. ) ;
#86646 = CARTESIAN_POINT ( 'NONE',  ( 3.837975233861466329, 21.70421690940786874, 11.49999999999999645 ) ) ;
#86648 = CARTESIAN_POINT ( 'NONE',  ( -103.5856513585207637, -24.65952944569304606, 1.056160979905703234 ) ) ;
#86649 = CARTESIAN_POINT ( 'NONE',  ( 5.419076944403256491, 21.93356404788375258, 11.49999999999998934 ) ) ;
#86650 = CARTESIAN_POINT ( 'NONE',  ( 14.98681507544721292, -14.71779577663021321, -1.500000000000002220 ) ) ;
#86652 = ORIENTED_EDGE ( 'NONE', *, *, #66400, .T. ) ;
#86651 = CARTESIAN_POINT ( 'NONE',  ( -62.52287095715006160, -23.94994826722564696, -0.6494450866342735829 ) ) ;
#86653 = ORIENTED_EDGE ( 'NONE', *, *, #14157, .F. ) ;
#86654 = LINE ( 'NONE', #11531, #83927 ) ;
#86655 = CIRCLE ( 'NONE', #68842, 2.350000000000000089 ) ;
#86656 = CARTESIAN_POINT ( 'NONE',  ( -90.62287095715001328, -24.51254535404253332, 9.355368623467651190 ) ) ;
#86657 = ORIENTED_EDGE ( 'NONE', *, *, #96654, .F. ) ;
#86658 = CARTESIAN_POINT ( 'NONE',  ( -3.482456173223098528, 20.84670800329844198, 11.49999999999998934 ) ) ;
#86659 = CARTESIAN_POINT ( 'NONE',  ( -0.3244794670026783234, -9.612687562450236811, 9.000000000000000000 ) ) ;
#86660 = CARTESIAN_POINT ( 'NONE',  ( -51.54603119510975517, -25.26041023287835330, 7.131525817319249505 ) ) ;
#86661 = CARTESIAN_POINT ( 'NONE',  ( -121.5924648986724321, -23.48783264082477018, -1.443836473390087694 ) ) ;
#86662 = CARTESIAN_POINT ( 'NONE',  ( -6.720452724358975338, -6.376774720514411854, 19.46153846153846700 ) ) ;
#86663 = CARTESIAN_POINT ( 'NONE',  ( -47.62287095715005592, -24.33927499327854704, 9.819080762295826048 ) ) ;
#86664 = CARTESIAN_POINT ( 'NONE',  ( -17.05807961832342912, 14.25954964135033265, -1.500000000000002220 ) ) ;
#86665 = CARTESIAN_POINT ( 'NONE',  ( -49.57708068730813267, -25.13941455849516515, 7.373516634279884130 ) ) ;
#86666 = ADVANCED_FACE ( 'NONE', ( #63264 ), #38403, .T. ) ;
#86667 = CIRCLE ( 'NONE', #46249, 4.450000000000000178 ) ;
#86668 = ORIENTED_EDGE ( 'NONE', *, *, #100198, .T. ) ;
#86669 = CARTESIAN_POINT ( 'NONE',  ( -110.6228709571500843, -23.47596703998600631, 11.44779298504227860 ) ) ;
#86670 = CARTESIAN_POINT ( 'NONE',  ( -37.61806166826795561, -23.48783264082478084, -1.443836473390075703 ) ) ;
#86671 = CARTESIAN_POINT ( 'NONE',  ( -40.09687989520371332, -25.30461012899484174, 5.519286114388885167 ) ) ;
#86672 = CARTESIAN_POINT ( 'NONE',  ( -100.5881607692819699, -24.63355581998384380, 0.9682620441943933232 ) ) ;
#86673 = CARTESIAN_POINT ( 'NONE',  ( -33.52287095715006160, -24.65952944569303895, 1.056160979905690134 ) ) ;
#86674 = CARTESIAN_POINT ( 'NONE',  ( 15.68791110202092476, 11.56419973807686219, -1.500000000000002220 ) ) ;
#86675 = EDGE_CURVE ( 'NONE', #87869, #45450, #46735, .T. ) ;
#86676 = CARTESIAN_POINT ( 'NONE',  ( 10.55508701655855575, -18.62573008410804221, -1.500000000000002220 ) ) ;
#86677 = CARTESIAN_POINT ( 'NONE',  ( 11.62916340711181284, -5.965225279485572685, 28.75961759920349792 ) ) ;
#86678 = CARTESIAN_POINT ( 'NONE',  ( -59.56094173781918499, -25.21083105912962097, 3.409327675794633805 ) ) ;
#86679 = EDGE_CURVE ( 'NONE', #16727, #60162, #8458, .T. ) ;
#86680 = CARTESIAN_POINT ( 'NONE',  ( -51.49050306338898508, -24.51314013834315730, 0.6176544820404109570 ) ) ;
#86681 = CARTESIAN_POINT ( 'NONE',  ( -101.2457357660222641, -25.27360070449644880, 3.734960848544197187 ) ) ;
#86682 = CARTESIAN_POINT ( 'NONE',  ( -21.73129956901698989, 6.668506094012985663, -1.500000000000002220 ) ) ;
#86683 = DIRECTION ( 'NONE',  ( -3.773278334453079030E-23, 0.9999999999976377785, 2.173523156925979128E-06 ) ) ;
#86684 = CARTESIAN_POINT ( 'NONE',  ( -73.22287095715006444, -23.47593901973090169, -1.443836447538997536 ) ) ;
#86685 = CARTESIAN_POINT ( 'NONE',  ( -7.150643268323968904, -18.52920452239153448, 11.49999999999999645 ) ) ;
#86686 = CARTESIAN_POINT ( 'NONE',  ( -123.5570543124543548, -23.48786465467241413, 11.44779295918253759 ) ) ;
#86687 = CARTESIAN_POINT ( 'NONE',  ( 22.02124265030973760, -5.356774720514425603, 19.55402280011862004 ) ) ;
#86688 = FACE_OUTER_BOUND ( 'NONE', #50977, .T. ) ;
#86689 = ORIENTED_EDGE ( 'NONE', *, *, #95764, .T. ) ;
#86690 = EDGE_CURVE ( 'NONE', #6469, #97458, #54642, .T. ) ;
#86691 = CARTESIAN_POINT ( 'NONE',  ( -123.5228709571501042, -23.48783264082477018, -1.443836473390084141 ) ) ;
#86692 = LINE ( 'NONE', #92796, #52369 ) ;
#86693 = CARTESIAN_POINT ( 'NONE',  ( -63.55620429048339304, -23.48786465467241058, 11.44779295918254824 ) ) ;
#86694 = CARTESIAN_POINT ( 'NONE',  ( -1.126084586642228436, -21.63456646517454729, -1.500000000000002220 ) ) ;
#86695 = CARTESIAN_POINT ( 'NONE',  ( -17.22176335520693158, -9.073154711715998744, -1.500000000000002220 ) ) ;
#86696 = CARTESIAN_POINT ( 'NONE',  ( -112.6228709571500559, -29.50250243563736774, 8.947779886222136270 ) ) ;
#86697 = ORIENTED_EDGE ( 'NONE', *, *, #30636, .F. ) ;
#86698 = VECTOR ( 'NONE', #95688, 1000.000000000000114 ) ;
#86699 = CARTESIAN_POINT ( 'NONE',  ( 8.094744887094867281, -18.73235182305680624, 11.49999999999999645 ) ) ;
#86700 = DIRECTION ( 'NONE',  ( 0.7512896232465891000, 0.000000000000000000, 0.6599726524652351767 ) ) ;
#86701 = CARTESIAN_POINT ( 'NONE',  ( -104.5562042904834072, -23.48783264082478084, -1.443836473390061936 ) ) ;
#86702 = EDGE_LOOP ( 'NONE', ( #69363, #59950, #24744, #42102 ) ) ;
#86703 = LINE ( 'NONE', #17193, #11874 ) ;
#86704 = DIRECTION ( 'NONE',  ( 0.000000000000000000, 0.9999999999976377785, 2.173523156925979975E-06 ) ) ;
#86705 = CARTESIAN_POINT ( 'NONE',  ( 7.275731542451676859, -6.376774720514415407, 20.06332870126568224 ) ) ;
#86706 =( BOUNDED_SURFACE ( )  B_SPLINE_SURFACE ( 3, 2, ( 
 ( #91513, #15381, #30614 ),
 ( #53477, #100100, #6776 ),
 ( #22980, #6283, #75785 ),
 ( #29616, #14385, #40614 ),
 ( #94886, #63467, #77276 ),
 ( #94389, #84404, #53970 ),
 ( #71569, #2062, #55847 ),
 ( #99119, #37731, #24871 ) ),
 .UNSPECIFIED., .F., .F., .F. ) 
 B_SPLINE_SURFACE_WITH_KNOTS ( ( 4, 2, 2, 4 ),
 ( 3, 3 ),
 ( 0.04217399329892001364, 0.04593451325143335651, 0.04781477322769002447, 0.04969503320394669937 ),
 ( 0.000000000000000000, 1.000000000000000000 ),
 .UNSPECIFIED. ) 
 GEOMETRIC_REPRESENTATION_ITEM ( )  RATIONAL_B_SPLINE_SURFACE ( (
 ( 1.000000000000000000, 0.7071067811865475727, 1.000000000000000000),
 ( 1.000000000000000000, 0.7337798844374378016, 1.000000000000000000),
 ( 1.000000000000000000, 0.7590275050786486899, 1.000000000000000000),
 ( 1.000000000000000000, 0.7948576648490734975, 1.000000000000000000),
 ( 1.000000000000000000, 0.8064603411375558251, 1.000000000000000000),
 ( 1.000000000000000000, 0.8289835611541060967, 1.000000000000000000),
 ( 1.000000000000000000, 0.8399042809640585583, 1.000000000000000000),
 ( 1.000000000000000000, 0.8504728678901986028, 1.000000000000000000) ) ) 
 REPRESENTATION_ITEM ( '' )  SURFACE ( )  );
#86707 = B_SPLINE_CURVE_WITH_KNOTS ( 'NONE', 3,
 ( #83233, #83731, #84229, #14716, #29947, #53800 ),
 .UNSPECIFIED., .F., .F.,
 ( 4, 2, 4 ),
 ( 0.000000000000000000, 0.001380764517853246432, 0.002761529035706492864 ),
 .UNSPECIFIED. ) ;
#86708 = LINE ( 'NONE', #17198, #68954 ) ;
#86709 = CARTESIAN_POINT ( 'NONE',  ( 10.48293302797296356, 17.13603372422173976, 11.49999999999998934 ) ) ;
#86710 = ADVANCED_FACE ( 'NONE', ( #17063 ), #77451, .F. ) ;
#86711 = DIRECTION ( 'NONE',  ( 0.7512896232465891000, 1.109416176496794925E-16, 0.6599726524652351767 ) ) ;
#86712 = ORIENTED_EDGE ( 'NONE', *, *, #30538, .T. ) ;
#86713 = FACE_OUTER_BOUND ( 'NONE', #3604, .T. ) ;
#86714 = ADVANCED_FACE ( 'NONE', ( #100275 ), #93685, .F. ) ;
#86715 = CARTESIAN_POINT ( 'NONE',  ( -22.94451526424785115, -1.264959178018935315, 11.49999999999999645 ) ) ;
#86716 = CARTESIAN_POINT ( 'NONE',  ( 21.15473741701296362, -8.388382055385795510, -1.500000000000002220 ) ) ;
#86717 = ORIENTED_EDGE ( 'NONE', *, *, #97324, .T. ) ;
#86718 = CARTESIAN_POINT ( 'NONE',  ( -45.52287095715004739, -23.48783264082477018, -1.443836473390097019 ) ) ;
#86719 = CARTESIAN_POINT ( 'NONE',  ( -7.749999999999996447, 24.84999999999999787, 2.100000000000000089 ) ) ;
#86720 = CARTESIAN_POINT ( 'NONE',  ( -90.54595667564740324, -24.63355581998384736, 0.9682620441943978751 ) ) ;
#86721 = DIRECTION ( 'NONE',  ( 0.1489078231574191002, 6.845827386180410961E-16, -0.9888510809027407644 ) ) ;
#86722 = CIRCLE ( 'NONE', #42997, 3.060000000000000497 ) ;
#86723 = EDGE_CURVE ( 'NONE', #48372, #13321, #78733, .T. ) ;
#86724 = DIRECTION ( 'NONE',  ( 0.000000000000000000, 0.000000000000000000, 1.000000000000000000 ) ) ;
#86725 = EDGE_CURVE ( 'NONE', #27806, #61427, #59548, .T. ) ;
#86726 = CARTESIAN_POINT ( 'NONE',  ( -121.5228709571500616, -24.64898659630529565, 1.056161002820833028 ) ) ;
#86727 = CARTESIAN_POINT ( 'NONE',  ( -39.62287095715005592, -24.65952944569304606, 1.056160979905692354 ) ) ;
#86728 = CARTESIAN_POINT ( 'NONE',  ( -98.89580656140421411, -25.25460702255793777, 6.002154820449574935 ) ) ;
#86729 = VERTEX_POINT ( 'NONE', #47530 ) ;
#86730 = CARTESIAN_POINT ( 'NONE',  ( -14.54385459823299875, 14.27422344363935025, 11.49999999999998934 ) ) ;
#86731 = ORIENTED_EDGE ( 'NONE', *, *, #60438, .F. ) ;
#86732 = ORIENTED_EDGE ( 'NONE', *, *, #72940, .F. ) ;
#86733 = CARTESIAN_POINT ( 'NONE',  ( -19.99251892732797486, -11.32171818645973538, 11.49999999999998934 ) ) ;
#86734 = CARTESIAN_POINT ( 'NONE',  ( -1.595974963000059477, -6.376774720514408301, 19.39236848396478408 ) ) ;
#86735 = AXIS2_PLACEMENT_3D ( 'NONE', #92620, #54089, #29735 ) ;
#86736 = VERTEX_POINT ( 'NONE', #8955 ) ;
#86737 = CARTESIAN_POINT ( 'NONE',  ( -108.6335398323394230, -23.48786465467241413, 11.44779295918253759 ) ) ;
#86738 = DIRECTION ( 'NONE',  ( 0.000000000000000000, -0.4450093991605204025, 0.8955258983741301027 ) ) ;
#86739 = VECTOR ( 'NONE', #99206, 1000.000000000000000 ) ;
#86740 = CARTESIAN_POINT ( 'NONE',  ( -78.55620429048339304, -24.64965694238574656, 8.947790433994198267 ) ) ;
#86741 = CARTESIAN_POINT ( 'NONE',  ( -119.1722160062776226, -25.27149295872829882, 5.922904214524349342 ) ) ;
#86743 = VERTEX_POINT ( 'NONE', #89085 ) ;
#86742 = CARTESIAN_POINT ( 'NONE',  ( -9.236746577462426444, 19.23066362772381055, 11.49999999999999645 ) ) ;
#86744 = EDGE_LOOP ( 'NONE', ( #55820, #59813, #88787, #22845, #74672, #81120, #47281, #78256, #45440, #80518, #36156, #35117, #31319, #37349, #21208 ) ) ;
#86745 = CARTESIAN_POINT ( 'NONE',  ( 10.78255534502030777, 19.45608938089507234, -1.500000000000002220 ) ) ;
#86746 = CARTESIAN_POINT ( 'NONE',  ( 20.62939718826500979, -0.8834638802319035866, 11.49999999999998934 ) ) ;
#86747 = EDGE_CURVE ( 'NONE', #71994, #53606, #57157, .T. ) ;
#86748 = ORIENTED_EDGE ( 'NONE', *, *, #94322, .F. ) ;
#86749 = FACE_OUTER_BOUND ( 'NONE', #92119, .T. ) ;
#86750 = CARTESIAN_POINT ( 'NONE',  ( -95.58789313718423841, -24.63419186844610920, 9.035850630976922204 ) ) ;
#86751 = VERTEX_POINT ( 'NONE', #88095 ) ;
#86752 = CARTESIAN_POINT ( 'NONE',  ( -73.62287095715005592, -29.50250243563736774, 8.947779886222143375 ) ) ;
#86753 = ORIENTED_EDGE ( 'NONE', *, *, #53630, .F. ) ;
#86754 = CARTESIAN_POINT ( 'NONE',  ( 5.271800844963591359, -3.316774720514426456, -28.56638892015329745 ) ) ;
#86755 = CARTESIAN_POINT ( 'NONE',  ( 6.044871794871792048, -6.376774720514401196, 18.16025641025640880 ) ) ;
#86756 = CARTESIAN_POINT ( 'NONE',  ( -16.98601802344612111, -12.12340321765213069, -1.500000000000002220 ) ) ;
#86757 = CARTESIAN_POINT ( 'NONE',  ( -6.661741538832703036, 20.79550341630197607, 11.49999999999999645 ) ) ;
#86758 = CARTESIAN_POINT ( 'NONE',  ( 25.42782340596018287, -5.181097800357524541, -8.121040708313532974 ) ) ;
#86759 = CARTESIAN_POINT ( 'NONE',  ( 5.090559816868301724, -3.309281602496330521, -27.56260619295190040 ) ) ;
#86760 = CARTESIAN_POINT ( 'NONE',  ( -15.60622653811170402, 16.18669697583415967, 11.49999999999998934 ) ) ;
#86761 = EDGE_CURVE ( 'NONE', #50194, #98189, #80032, .T. ) ;
#86762 = EDGE_CURVE ( 'NONE', #55399, #3242, #72858, .T. ) ;
#86763 = CARTESIAN_POINT ( 'NONE',  ( -118.5911711092949332, -23.96169478059713853, 10.65365249895717170 ) ) ;
#86764 = CARTESIAN_POINT ( 'NONE',  ( -125.5228709571500616, -29.50248789122583659, 2.256150453626215580 ) ) ;
#86765 = CARTESIAN_POINT ( 'NONE',  ( -59.52287095715006160, -23.47596703998600631, 11.44779298504228926 ) ) ;
#86766 = ORIENTED_EDGE ( 'NONE', *, *, #88150, .T. ) ;
#86767 = VECTOR ( 'NONE', #20301, 1000.000000000000114 ) ;
#86768 = ORIENTED_EDGE ( 'NONE', *, *, #51977, .F. ) ;
#86769 = ORIENTED_EDGE ( 'NONE', *, *, #30392, .F. ) ;
#86770 = CARTESIAN_POINT ( 'NONE',  ( -100.0836892525862254, -25.26221310139842302, 7.064315631329017187 ) ) ;
#86771 = VERTEX_POINT ( 'NONE', #42431 ) ;
#86772 = CARTESIAN_POINT ( 'NONE',  ( -13.24026558610970916, 16.85365899302435722, -1.500000000000002220 ) ) ;
#86773 = CARTESIAN_POINT ( 'NONE',  ( -21.65924713590726469, 5.634197536097032888, 11.49999999999999645 ) ) ;
#86774 = VERTEX_POINT ( 'NONE', #1852 ) ;
#86775 = PLANE ( 'NONE',  #69930 ) ;
#86776 = CARTESIAN_POINT ( 'NONE',  ( 13.75562813033083742, -15.94169299924578453, 11.49999999999998934 ) ) ;
#86777 = CARTESIAN_POINT ( 'NONE',  ( -30.55373813234560032, -24.38552179065370851, 9.702671485061733492 ) ) ;
#86778 = CARTESIAN_POINT ( 'NONE',  ( 18.80405327530603543, -6.659971710459020144, -1.500000000000002220 ) ) ;
#86779 = FACE_OUTER_BOUND ( 'NONE', #45934, .T. ) ;
#86780 = CARTESIAN_POINT ( 'NONE',  ( 0.01063402156994475850, -0.1430980438411110500, 9.000000000000000000 ) ) ;
#86781 = CARTESIAN_POINT ( 'NONE',  ( -20.36895902721504825, -8.506870616244709637, -1.500000000000002220 ) ) ;
#86782 = VERTEX_POINT ( 'NONE', #71369 ) ;
#86783 = CARTESIAN_POINT ( 'NONE',  ( -65.53712136039511904, -24.73531770709095312, 8.716586749053508498 ) ) ;
#86784 = ADVANCED_FACE ( 'NONE', ( #27189 ), #34302, .F. ) ;
#86785 = DIRECTION ( 'NONE',  ( 0.000000000000000000, 0.000000000000000000, 1.000000000000000000 ) ) ;
#86786 = CARTESIAN_POINT ( 'NONE',  ( 12.46380520747237419, 16.70348211664046900, 11.49999999999999645 ) ) ;
#86787 = CARTESIAN_POINT ( 'NONE',  ( 31.67769140193634314, -4.988134948533209823, 28.98636546410035564 ) ) ;
#86788 = DIRECTION ( 'NONE',  ( 0.000000000000000000, -2.173523156925980399E-06, 0.9999999999976378895 ) ) ;
#86789 = DIRECTION ( 'NONE',  ( -0.09824042138329623641, -0.9951627101165078093, -3.504396110891626425E-15 ) ) ;
#86790 = CARTESIAN_POINT ( 'NONE',  ( -12.43717309395686499, -17.31322327496724611, -1.500000000000002220 ) ) ;
#86791 = CARTESIAN_POINT ( 'NONE',  ( -81.52287095715006160, -23.94994826722564696, -0.6494450866342743600 ) ) ;
#86792 = CARTESIAN_POINT ( 'NONE',  ( -33.62287095715005592, -29.50248528299804818, 1.056150453629029817 ) ) ;
#86793 = EDGE_CURVE ( 'NONE', #62739, #59306, #15842, .T. ) ;
#86794 = CARTESIAN_POINT ( 'NONE',  ( -96.52287095715006160, -23.48786465467241769, 11.44779295918254114 ) ) ;
#86795 = CARTESIAN_POINT ( 'NONE',  ( 25.83488407601165093, 3.407774720514426647, -11.31196583263649558 ) ) ;
#86796 = CARTESIAN_POINT ( 'NONE',  ( -20.50338545487000275, 9.463669735852004550, -1.500000000000002220 ) ) ;
#86797 = AXIS2_PLACEMENT_3D ( 'NONE', #36692, #98578, #60047 ) ;
#86798 = ADVANCED_FACE ( 'NONE', ( #11951 ), #49038, .F. ) ;
#86799 = CARTESIAN_POINT ( 'NONE',  ( -51.52287095715008292, -23.96177878511308634, 10.65340807706329862 ) ) ;
#86800 = ORIENTED_EDGE ( 'NONE', *, *, #5024, .F. ) ;
#86801 = DIRECTION ( 'NONE',  ( 1.000000000000000000, -0.000000000000000000, 0.000000000000000000 ) ) ;
#86802 = CARTESIAN_POINT ( 'NONE',  ( -122.6228709571500417, -24.64898659630368627, 1.056161002820833028 ) ) ;
#86803 = CARTESIAN_POINT ( 'NONE',  ( -8.025172913017740939, -17.94849717234452768, 11.49999999999999645 ) ) ;
#86804 = CARTESIAN_POINT ( 'NONE',  ( -2.449489742783178770, 4.293056017849825601, 2.499999999999999556 ) ) ;
#86805 = VECTOR ( 'NONE', #53855, 1000.000000000000000 ) ;
#86806 = CARTESIAN_POINT ( 'NONE',  ( -119.5228709571500758, -24.64965694238408034, 8.947790433994191162 ) ) ;
#86807 = ORIENTED_EDGE ( 'NONE', *, *, #46281, .T. ) ;
#86808 = EDGE_CURVE ( 'NONE', #57983, #91978, #100146, .T. ) ;
#86809 = CARTESIAN_POINT ( 'NONE',  ( -9.299999999999991829, 12.00000000000002309, 2.100000000000000089 ) ) ;
#86810 = CARTESIAN_POINT ( 'NONE',  ( -41.32836283488544638, 4.132774720514426292, 39.26872235229541985 ) ) ;
#86811 = DIRECTION ( 'NONE',  ( 0.000000000000000000, -2.173523156925979552E-06, 0.9999999999976378895 ) ) ;
#86813 = CARTESIAN_POINT ( 'NONE',  ( 19.24418710706453339, -0.5000000000000000000, 2.346898003627108320 ) ) ;
#86812 = AXIS2_PLACEMENT_3D ( 'NONE', #11245, #57940, #94476 ) ;
#86814 = ADVANCED_FACE ( 'NONE', ( #26184 ), #20029, .T. ) ;
#86815 = CARTESIAN_POINT ( 'NONE',  ( -2.169994883066378222, 10.75358048763950869, 3.549999999999999822 ) ) ;
#86816 = CARTESIAN_POINT ( 'NONE',  ( 19.69962056004252560, 1.334664424591413434, 11.49999999999998934 ) ) ;
#86817 = ORIENTED_EDGE ( 'NONE', *, *, #70573, .T. ) ;
#86818 = CARTESIAN_POINT ( 'NONE',  ( -1.055277534996966970, 20.15608268182561247, 11.49999999999999645 ) ) ;
#86819 = CARTESIAN_POINT ( 'NONE',  ( -6.775140224358976226, -5.876774720514409189, 19.14743589743590846 ) ) ;
#86820 = ORIENTED_EDGE ( 'NONE', *, *, #99589, .T. ) ;
#86821 = LINE ( 'NONE', #45762, #49116 ) ;
#86822 = DIRECTION ( 'NONE',  ( 0.000000000000000000, 1.000000000000000000, 0.000000000000000000 ) ) ;
#86823 = CARTESIAN_POINT ( 'NONE',  ( -10.24059822343757986, -5.876774720514426953, 22.82308057603840368 ) ) ;
#86824 = CARTESIAN_POINT ( 'NONE',  ( -69.75867036063475268, -25.12509700652633171, 2.913778224305814124 ) ) ;
#86825 = DIRECTION ( 'NONE',  ( -3.773278334453079030E-23, 0.9999999999976377785, 2.173523156925979128E-06 ) ) ;
#86826 = CARTESIAN_POINT ( 'NONE',  ( -58.52287095715006160, -24.64898659630528499, 1.056161002820822592 ) ) ;
#86827 = CARTESIAN_POINT ( 'NONE',  ( 16.76344175524385705, -10.90933549886441156, 11.49999999999998934 ) ) ;
#86828 = CARTESIAN_POINT ( 'NONE',  ( -99.49608100277511369, -25.27532937069960184, 3.179641110928470127 ) ) ;
#86829 = CARTESIAN_POINT ( 'NONE',  ( -116.6272977626530292, -23.96169478059714208, 10.65365249895717348 ) ) ;
#86830 = ORIENTED_EDGE ( 'NONE', *, *, #83801, .T. ) ;
#86831 = EDGE_CURVE ( 'NONE', #80901, #48067, #31674, .T. ) ;
#86832 = LINE ( 'NONE', #16823, #24281 ) ;
#86833 = CARTESIAN_POINT ( 'NONE',  ( -35.63364392773276990, -24.73486907724918282, 1.287355809206967461 ) ) ;
#86834 = CARTESIAN_POINT ( 'NONE',  ( -48.58953762381672448, -24.64965694238407323, 8.947790433994656567 ) ) ;
#86835 = CARTESIAN_POINT ( 'NONE',  ( -118.7287160163637481, -25.33540118152307841, 3.690489000554330712 ) ) ;
#86836 = PLANE ( 'NONE',  #43747 ) ;
#86837 = CARTESIAN_POINT ( 'NONE',  ( -45.52287095715006160, -23.47596703998600631, 11.44779298504229104 ) ) ;
#86838 = PLANE ( 'NONE',  #9650 ) ;
#86839 = ORIENTED_EDGE ( 'NONE', *, *, #41188, .F. ) ;
#86840 = CARTESIAN_POINT ( 'NONE',  ( -2.359408512905806443, -20.17289352931189583, -1.500000000000002220 ) ) ;
#86841 = CARTESIAN_POINT ( 'NONE',  ( 31.69086887328987956, 3.760767191028115519, 29.45064099519496992 ) ) ;
#86842 = CARTESIAN_POINT ( 'NONE',  ( -34.53217422167019635, -24.51314013834315375, 0.6176544820404091807 ) ) ;
#86843 = CARTESIAN_POINT ( 'NONE',  ( -59.55981053866136676, -23.73791477778911840, 11.05961554403171299 ) ) ;
#86844 = AXIS2_PLACEMENT_3D ( 'NONE', #41036, #18676, #79076 ) ;
#86845 = ORIENTED_EDGE ( 'NONE', *, *, #83212, .T. ) ;
#86846 = DIRECTION ( 'NONE',  ( 0.000000000000000000, -0.9999999999976377785, -2.173523156925979128E-06 ) ) ;
#86847 = CARTESIAN_POINT ( 'NONE',  ( 12.02422309597069017, 16.21794576832014556, -1.500000000000002220 ) ) ;
#86848 = CARTESIAN_POINT ( 'NONE',  ( -20.79277273739468512, 3.736189789763188607, 11.49999999999999645 ) ) ;
#86849 = CARTESIAN_POINT ( 'NONE',  ( 19.88262469969689050, -9.776007750257504014, -1.500000000000002220 ) ) ;
#86850 = CARTESIAN_POINT ( 'NONE',  ( -14.32454646668868747, 14.77526322620295929, 11.49999999999998934 ) ) ;
#86851 = AXIS2_PLACEMENT_3D ( 'NONE', #76841, #68266, #62156 ) ;
#86852 = EDGE_CURVE ( 'NONE', #46688, #16912, #11024, .T. ) ;
#86853 = FACE_OUTER_BOUND ( 'NONE', #61478, .T. ) ;
#86854 = ORIENTED_EDGE ( 'NONE', *, *, #96521, .T. ) ;
#86855 = CARTESIAN_POINT ( 'NONE',  ( -43.52287095715006160, -24.64898659630528854, 1.056161002820819261 ) ) ;
#86856 = ORIENTED_EDGE ( 'NONE', *, *, #17910, .T. ) ;
#86857 = CARTESIAN_POINT ( 'NONE',  ( -36.62287095715004170, -23.47596703998600276, 11.44779298504227505 ) ) ;
#86858 = CARTESIAN_POINT ( 'NONE',  ( -109.5228709571500332, -23.95044443724992789, 10.65354141964649237 ) ) ;
#86859 = EDGE_LOOP ( 'NONE', ( #91601, #34324, #48943, #84928 ) ) ;
#86860 = AXIS2_PLACEMENT_3D ( 'NONE', #32502, #53845, #1562 ) ;
#86861 = VERTEX_POINT ( 'NONE', #98677 ) ;
#86862 = CIRCLE ( 'NONE', #72257, 2.349999999999999645 ) ;
#86863 = ORIENTED_EDGE ( 'NONE', *, *, #31347, .T. ) ;
#86864 = DIRECTION ( 'NONE',  ( 0.000000000000000000, 0.000000000000000000, -1.000000000000000000 ) ) ;
#86865 = CARTESIAN_POINT ( 'NONE',  ( -28.92287090416851214, -23.34271810397723357, -1.443836447538997314 ) ) ;
#86866 = CARTESIAN_POINT ( 'NONE',  ( -108.5228709571500616, -24.64965694238408034, 8.947790433994192938 ) ) ;
#86867 = CARTESIAN_POINT ( 'NONE',  ( -10.41657757243416604, 17.86655067824183618, -1.500000000000002220 ) ) ;
#86868 = AXIS2_PLACEMENT_3D ( 'NONE', #43263, #65120, #11303 ) ;
#86869 = CARTESIAN_POINT ( 'NONE',  ( -6.031157642910047301, -20.80930661755759203, 11.49999999999999645 ) ) ;
#86870 = ORIENTED_EDGE ( 'NONE', *, *, #84970, .T. ) ;
#86871 = EDGE_CURVE ( 'NONE', #18354, #73552, #2582, .T. ) ;
#86872 = CARTESIAN_POINT ( 'NONE',  ( -99.07956767207025450, -25.29825536674003672, 5.429397271924422341 ) ) ;
#86873 = CARTESIAN_POINT ( 'NONE',  ( -33.52287095715006160, -29.50247984919015209, -1.443849546365062242 ) ) ;
#86874 = CARTESIAN_POINT ( 'NONE',  ( 18.65981798208652265, 12.38953945867474360, 11.49999999999998934 ) ) ;
#86875 = EDGE_CURVE ( 'NONE', #34853, #8365, #43420, .T. ) ;
#86876 = AXIS2_PLACEMENT_3D ( 'NONE', #79979, #47545, #63789 ) ;
#86877 = ADVANCED_FACE ( 'NONE', ( #27690 ), #75338, .F. ) ;
#86878 = CARTESIAN_POINT ( 'NONE',  ( -46.52287095715006160, -29.50250243563736774, 8.947779886222146928 ) ) ;
#86879 = DIRECTION ( 'NONE',  ( -1.000000000000000000, -3.773278334444166432E-23, -8.201307841325785021E-29 ) ) ;
#86880 = ORIENTED_EDGE ( 'NONE', *, *, #15219, .T. ) ;
#86881 = CARTESIAN_POINT ( 'NONE',  ( 26.73860345374794178, -1.477225279485574028, 19.84760796525321780 ) ) ;
#86882 = CARTESIAN_POINT ( 'NONE',  ( -35.61370034920652472, -23.85049219812685095, 10.88485053497527488 ) ) ;
#86883 = EDGE_CURVE ( 'NONE', #43602, #27656, #11093, .T. ) ;
#86884 = ORIENTED_EDGE ( 'NONE', *, *, #73080, .T. ) ;
#86885 = EDGE_LOOP ( 'NONE', ( #69141, #40989, #49926, #68890 ) ) ;
#86886 = CARTESIAN_POINT ( 'NONE',  ( -45.52287095715006870, -24.51254535375846189, 9.355368624242117903 ) ) ;
#86887 = ORIENTED_EDGE ( 'NONE', *, *, #73487, .T. ) ;
#86888 = PLANE ( 'NONE',  #17951 ) ;
#86889 = CARTESIAN_POINT ( 'NONE',  ( -21.21068194950259311, 0.7780057951688260642, -1.500000000000002220 ) ) ;
#86890 = ORIENTED_EDGE ( 'NONE', *, *, #48589, .F. ) ;
#86891 = CARTESIAN_POINT ( 'NONE',  ( -50.48315116308123862, -24.73486907724918282, 1.287355809206963464 ) ) ;
#86892 = CARTESIAN_POINT ( 'NONE',  ( 1.801620404824296084, -21.73869551012647605, 11.49999999999998934 ) ) ;
#86893 = CARTESIAN_POINT ( 'NONE',  ( -103.5131093972200773, -24.35071581493543391, 9.817618358456027039 ) ) ;
#86894 = B_SPLINE_CURVE_WITH_KNOTS ( 'NONE', 3,
 ( #25416, #73105, #81205, #33034 ),
 .UNSPECIFIED., .F., .F.,
 ( 4, 4 ),
 ( 0.01303003236488493519, 0.01305095637151315775 ),
 .UNSPECIFIED. ) ;
#86895 = LINE ( 'NONE', #17387, #21013 ) ;
#86896 = FACE_OUTER_BOUND ( 'NONE', #21475, .T. ) ;
#86897 = CARTESIAN_POINT ( 'NONE',  ( 21.05697796394607835, 5.830696701215154043, -1.500000000000002220 ) ) ;
#86898 = FACE_OUTER_BOUND ( 'NONE', #52826, .T. ) ;
#86899 = VERTEX_POINT ( 'NONE', #82460 ) ;
#86900 = CARTESIAN_POINT ( 'NONE',  ( -65.62287095715007013, -24.63287334234177806, 0.9662140553045478475 ) ) ;
#86901 = CARTESIAN_POINT ( 'NONE',  ( -85.50201578033416183, -24.63419186844611275, 9.035850630976915099 ) ) ;
#86902 = EDGE_CURVE ( 'NONE', #40713, #95088, #8686, .T. ) ;
#86903 = VERTEX_POINT ( 'NONE', #91069 ) ;
#86904 = VECTOR ( 'NONE', #20282, 1000.000000000000000 ) ;
#86905 = ORIENTED_EDGE ( 'NONE', *, *, #98545, .T. ) ;
#86906 = EDGE_CURVE ( 'NONE', #58835, #30291, #52518, .T. ) ;
#86907 = VERTEX_POINT ( 'NONE', #83451 ) ;
#86908 = CARTESIAN_POINT ( 'NONE',  ( -89.46310519935767047, -25.12049752546737480, 2.832404795212219106 ) ) ;
#86909 = CARTESIAN_POINT ( 'NONE',  ( -82.63299566570569255, -24.15543982623907482, -0.2315651400026497997 ) ) ;
#86910 = CARTESIAN_POINT ( 'NONE',  ( 20.49604761983493972, 5.601127818285958071, -1.500000000000002220 ) ) ;
#86911 = CARTESIAN_POINT ( 'NONE',  ( -27.68651082257923335, -29.50249951851372643, 7.605662314874230390 ) ) ;
#86912 = CARTESIAN_POINT ( 'NONE',  ( 6.499999999999992895, 2.239999999999996660, 2.100000000000000977 ) ) ;
#86913 = EDGE_CURVE ( 'NONE', #98477, #27379, #95845, .T. ) ;
#86914 = DIRECTION ( 'NONE',  ( -0.000000000000000000, -1.000000000000000000, -0.000000000000000000 ) ) ;
#86915 = CARTESIAN_POINT ( 'NONE',  ( -91.52287095715003318, -23.48783264082477018, -1.443836473390089248 ) ) ;
#86916 = CARTESIAN_POINT ( 'NONE',  ( 17.07123823605233781, 9.195568589125342029, -1.500000000000002220 ) ) ;
#86917 = CARTESIAN_POINT ( 'NONE',  ( -45.49175542960804819, -24.40034930558990922, 0.3402023900116019073 ) ) ;
#86918 = ORIENTED_EDGE ( 'NONE', *, *, #22848, .T. ) ;
#86919 = CARTESIAN_POINT ( 'NONE',  ( 2.628080361126900133, -19.32819128710564272, 11.49999999999999645 ) ) ;
#86920 = DIRECTION ( 'NONE',  ( -1.000000000000000000, 0.000000000000000000, 0.000000000000000000 ) ) ;
#86921 = CARTESIAN_POINT ( 'NONE',  ( -68.52287095715007581, -23.47593901973090524, -1.443836447538997092 ) ) ;
#86922 = VERTEX_POINT ( 'NONE', #35797 ) ;
#86923 = EDGE_CURVE ( 'NONE', #54685, #89496, #66770, .T. ) ;
#86924 = CARTESIAN_POINT ( 'NONE',  ( 4.689770114687411784, -6.376774720514424288, 21.33175327469028915 ) ) ;
#86925 = CARTESIAN_POINT ( 'NONE',  ( -89.58353647075207959, -24.65952944569304250, 1.056160979905701902 ) ) ;
#86927 = EDGE_CURVE ( 'NONE', #53725, #20580, #37295, .T. ) ;
#86926 = CARTESIAN_POINT ( 'NONE',  ( -7.326923076923074873, -5.876774720514426953, 21.75000000000001066 ) ) ;
#86928 = CARTESIAN_POINT ( 'NONE',  ( -81.79035934495350091, -25.03155870187092447, 6.685840044562571194 ) ) ;
#86929 = CARTESIAN_POINT ( 'NONE',  ( -19.44079195400435012, 3.002763184081948200, -1.500000000000002220 ) ) ;
#86930 = B_SPLINE_CURVE_WITH_KNOTS ( 'NONE', 3,
 ( #20686, #91693, #74969, #67384, #4973, #44540 ),
 .UNSPECIFIED., .F., .F.,
 ( 4, 2, 4 ),
 ( 0.000000000000000000, 0.001380764517853249251, 0.002761529035706498502 ),
 .UNSPECIFIED. ) ;
#86931 = VERTEX_POINT ( 'NONE', #98176 ) ;
#86932 = CARTESIAN_POINT ( 'NONE',  ( -109.6228709571500559, -29.50247984919015209, -1.443849546365048253 ) ) ;
#86933 = CARTESIAN_POINT ( 'NONE',  ( -23.06710473063640165, 0.7821689226722955413, -1.500000000000002220 ) ) ;
#86934 = AXIS2_PLACEMENT_3D ( 'NONE', #71258, #55544, #78846 ) ;
#86935 = PERSON_AND_ORGANIZATION ( #70597, #27821 ) ;
#86936 = CARTESIAN_POINT ( 'NONE',  ( 3.094204744773375815, -5.876774720514421624, 21.02053020447315745 ) ) ;
#86937 = CARTESIAN_POINT ( 'NONE',  ( -51.52287095715006870, -29.50248528299804818, 1.056150453629033370 ) ) ;
#86938 = CARTESIAN_POINT ( 'NONE',  ( -109.7112239897570163, -25.13124142841114050, 2.950745540745953743 ) ) ;
#86939 = CARTESIAN_POINT ( 'NONE',  ( -97.58870659920341950, -24.35071581493544102, 9.817618358456025263 ) ) ;
#86940 = CARTESIAN_POINT ( 'NONE',  ( -79.91702284995605510, -25.31249729222309242, 5.276660411446114196 ) ) ;
#86941 = VECTOR ( 'NONE', #65440, 1000.000000000000000 ) ;
#86943 = CARTESIAN_POINT ( 'NONE',  ( 6.377880655330028681, -5.876774720514423400, 21.48000012937543346 ) ) ;
#86942 = CIRCLE ( 'NONE', #44798, 251.4258649670780699 ) ;
#86944 = CARTESIAN_POINT ( 'NONE',  ( 31.31283134548411340, -4.772774720514425972, -10.20862453625735178 ) ) ;
#86945 = CARTESIAN_POINT ( 'NONE',  ( -111.3663525145439053, -25.29779355382247985, 4.214194357447069272 ) ) ;
#86946 = CARTESIAN_POINT ( 'NONE',  ( -19.91179686852411734, 0.6080443046932394457, 11.49999999999998934 ) ) ;
#86947 = B_SPLINE_CURVE_WITH_KNOTS ( 'NONE', 3,
 ( #32653, #16929, #94052, #70721, #46383, #77317 ),
 .UNSPECIFIED., .F., .F.,
 ( 4, 2, 4 ),
 ( 0.000000000000000000, 0.001380901958385393966, 0.002761803916770787931 ),
 .UNSPECIFIED. ) ;
#86948 = DIRECTION ( 'NONE',  ( -1.000000000000000000, -3.773278334444166432E-23, -8.201307841325785021E-29 ) ) ;
#86949 = CARTESIAN_POINT ( 'NONE',  ( -11.05534852661189937, -16.44151763790470966, -1.500000000000002220 ) ) ;
#86950 = ORIENTED_EDGE ( 'NONE', *, *, #86551, .T. ) ;
#86951 = AXIS2_PLACEMENT_3D ( 'NONE', #53031, #67260, #35801 ) ;
#86952 = LINE ( 'NONE', #27062, #99374 ) ;
#86953 = CARTESIAN_POINT ( 'NONE',  ( 32.40199294184732537, -6.475225279485573360, -12.82361242714782712 ) ) ;
#86954 = CARTESIAN_POINT ( 'NONE',  ( -35.62287095715005592, -24.91570333823099404, 8.075032458375558164 ) ) ;
#86955 = CARTESIAN_POINT ( 'NONE',  ( -7.464567774302189207, 19.34240081622845153, 11.49999999999999645 ) ) ;
#86956 = DIRECTION ( 'NONE',  ( -3.773278334444167608E-23, 1.000000000000000000, 0.000000000000000000 ) ) ;
#86957 = CARTESIAN_POINT ( 'NONE',  ( -78.52287095715006160, -23.47596703998600631, 11.44779298504228571 ) ) ;
#86958 = CARTESIAN_POINT ( 'NONE',  ( 22.53581206741051446, 3.480912172000575122, 11.49999999999999645 ) ) ;
#86959 = ORIENTED_EDGE ( 'NONE', *, *, #73518, .T. ) ;
#86960 = CARTESIAN_POINT ( 'NONE',  ( -69.54473523537089363, -24.34968618360934300, 0.1864209137778826408 ) ) ;
#86961 = CARTESIAN_POINT ( 'NONE',  ( 0.000000000000000000, -4.056774720514426669, 0.000000000000000000 ) ) ;
#86962 = ORIENTED_EDGE ( 'NONE', *, *, #39920, .T. ) ;
#86963 = CARTESIAN_POINT ( 'NONE',  ( 17.48260522047220888, -10.12088315688240314, 11.49999999999998934 ) ) ;
#86964 = FACE_OUTER_BOUND ( 'NONE', #19515, .T. ) ;
#86965 = CARTESIAN_POINT ( 'NONE',  ( -110.5228709571500616, -24.83620972994592435, 8.398175272781363887 ) ) ;
#86966 = AXIS2_PLACEMENT_3D ( 'NONE', #86878, #140, #33098 ) ;
#86967 = ORIENTED_EDGE ( 'NONE', *, *, #97462, .T. ) ;
#86968 = CARTESIAN_POINT ( 'NONE',  ( -127.5228709571499763, -23.48783264082477373, -1.443836473390082586 ) ) ;
#86969 = CARTESIAN_POINT ( 'NONE',  ( -30.57287095715006231, -23.47596702059239604, 11.43887032355635647 ) ) ;
#86970 = CARTESIAN_POINT ( 'NONE',  ( 1.534201407001029027, 19.92515851932037663, -1.500000000000002220 ) ) ;
#86971 = DIRECTION ( 'NONE',  ( -0.000000000000000000, -0.000000000000000000, -1.000000000000000000 ) ) ;
#86972 = CARTESIAN_POINT ( 'NONE',  ( -20.92093621315066443, -1.481899440790641842, 11.49999999999999645 ) ) ;
#86973 = AXIS2_PLACEMENT_3D ( 'NONE', #38728, #15891, #45370 ) ;
#86974 = CARTESIAN_POINT ( 'NONE',  ( 15.63605935613269438, 5.965225279485572685, -27.55169773172585934 ) ) ;
#86975 = CARTESIAN_POINT ( 'NONE',  ( 11.16000000000000014, -10.15233964170348457, 0.003711184059992174607 ) ) ;
#86976 = CARTESIAN_POINT ( 'NONE',  ( 1.153593019990587942, -22.03401787307112869, -1.500000000000002220 ) ) ;
#86977 = CARTESIAN_POINT ( 'NONE',  ( -127.4728709571500360, -25.40674640480649416, 5.000950437805943061 ) ) ;
#86978 = ORIENTED_EDGE ( 'NONE', *, *, #14947, .F. ) ;
#86979 = DIRECTION ( 'NONE',  ( 0.000000000000000000, -0.9999999999976377785, -2.173523156925979975E-06 ) ) ;
#86980 = CARTESIAN_POINT ( 'NONE',  ( -35.62287095715005592, -23.47593901973091235, -1.443836447539011525 ) ) ;
#86981 = CARTESIAN_POINT ( 'NONE',  ( 27.86270917940689174, -5.965225279485572685, 29.49402280011862487 ) ) ;
#86982 = ORIENTED_EDGE ( 'NONE', *, *, #53927, .F. ) ;
#86983 = DIRECTION ( 'NONE',  ( 0.000000000000000000, -2.173523156925980399E-06, 0.9999999999976378895 ) ) ;
#86984 = EDGE_CURVE ( 'NONE', #61220, #54573, #15435, .T. ) ;
#86985 = ORIENTED_EDGE ( 'NONE', *, *, #96884, .F. ) ;
#86986 = ADVANCED_FACE ( 'NONE', ( #38275 ), #38860, .T. ) ;
#86987 = ORIENTED_EDGE ( 'NONE', *, *, #69830, .T. ) ;
#86988 = CARTESIAN_POINT ( 'NONE',  ( -118.5228709571501184, -24.66019654487200441, 8.947790411086110396 ) ) ;
#86989 = LINE ( 'NONE', #33714, #76167 ) ;
#86990 = CARTESIAN_POINT ( 'NONE',  ( -94.62287095715005592, -23.47596703998600631, 11.44779298504227860 ) ) ;
#86991 = CARTESIAN_POINT ( 'NONE',  ( -20.41219973434085944, 2.133827299322149429, -1.500000000000002220 ) ) ;
#86992 = EDGE_CURVE ( 'NONE', #73682, #59253, #99427, .T. ) ;
#86993 = ORIENTED_EDGE ( 'NONE', *, *, #50274, .T. ) ;
#86994 = CARTESIAN_POINT ( 'NONE',  ( -116.5228709571500332, -24.66019654487200086, 8.947790411086113949 ) ) ;
#86995 = CARTESIAN_POINT ( 'NONE',  ( -10.23894677657808749, 4.339657088724310441, 29.22408179085893210 ) ) ;
#86996 = CARTESIAN_POINT ( 'NONE',  ( -41.52287095715008292, -23.95044443724991723, 10.65354141964649237 ) ) ;
#86997 = CARTESIAN_POINT ( 'NONE',  ( -20.55042600948665310, 8.738301046694649798, -1.500000000000002220 ) ) ;
#86998 = EDGE_CURVE ( 'NONE', #50083, #65105, #67889, .T. ) ;
#86999 = AXIS2_PLACEMENT_3D ( 'NONE', #21779, #6072, #91310 ) ;
#87000 = EDGE_CURVE ( 'NONE', #70182, #5644, #70234, .T. ) ;
#87001 = CARTESIAN_POINT ( 'NONE',  ( -0.07181233839971860877, -22.12033284636825314, 9.440663514584120009 ) ) ;
#87002 = CARTESIAN_POINT ( 'NONE',  ( -55.52287095715006870, -29.50248528299804818, 1.056150453629034924 ) ) ;
#87003 = VERTEX_POINT ( 'NONE', #78329 ) ;
#87004 = CARTESIAN_POINT ( 'NONE',  ( 14.76093561896379214, 3.316774720514426456, -27.37148769130089931 ) ) ;
#87005 = LINE ( 'NONE', #48461, #45901 ) ;
#87006 = CARTESIAN_POINT ( 'NONE',  ( 2.550444227103870531, -20.70361394434535285, -1.500000000000002220 ) ) ;
#87007 = EDGE_LOOP ( 'NONE', ( #4392, #2554, #16599, #40949 ) ) ;
#87009 = EDGE_LOOP ( 'NONE', ( #53991, #39638, #96267, #84839 ) ) ;
#87008 = LINE ( 'NONE', #80401, #47394 ) ;
#87010 = AXIS2_PLACEMENT_3D ( 'NONE', #88989, #19459, #18466 ) ;
#87011 = ORIENTED_EDGE ( 'NONE', *, *, #80374, .T. ) ;
#87012 = CARTESIAN_POINT ( 'NONE',  ( -32.66693324679340549, -24.96126789006231306, 2.105721083233587532 ) ) ;
#87013 = CARTESIAN_POINT ( 'NONE',  ( 18.99863377428308198, 9.053671573812124507, -1.500000000000002220 ) ) ;
#87014 = EDGE_LOOP ( 'NONE', ( #61496, #98329, #19495, #67778 ) ) ;
#87015 = AXIS2_PLACEMENT_3D ( 'NONE', #9897, #55592, #71310 ) ;
#87016 = DIRECTION ( 'NONE',  ( 0.000000000000000000, -2.173523156925979552E-06, 0.9999999999976378895 ) ) ;
#87017 = CARTESIAN_POINT ( 'NONE',  ( -0.3244794670026783234, -9.612687562450236811, 9.000000000000000000 ) ) ;
#87018 = CARTESIAN_POINT ( 'NONE',  ( -105.5228709571500758, -25.00182538069145366, 7.747789668545101094 ) ) ;
#87019 = VECTOR ( 'NONE', #96624, 1000.000000000000114 ) ;
#87020 = CARTESIAN_POINT ( 'NONE',  ( -86.50205518092207058, -24.66019654487200086, 8.947790411086117501 ) ) ;
#87021 = CARTESIAN_POINT ( 'NONE',  ( -73.55620429048342146, -24.65952944569304606, 1.056160979905697461 ) ) ;
#87022 = LINE ( 'NONE', #25113, #52908 ) ;
#87023 = CARTESIAN_POINT ( 'NONE',  ( -65.62287095715005592, -25.00182538069145721, 7.747789668545100206 ) ) ;
#87025 = VERTEX_POINT ( 'NONE', #62633 ) ;
#87024 = CARTESIAN_POINT ( 'NONE',  ( -13.56020932195406203, -17.60290058955388659, 11.49999999999999645 ) ) ;
#87026 = DIRECTION ( 'NONE',  ( -3.773278334453079618E-23, 0.9999999999976377785, 2.173523156925979975E-06 ) ) ;
#87027 = CARTESIAN_POINT ( 'NONE',  ( -37.62287095715005592, -23.48786465467240347, 11.44779295918255180 ) ) ;
#87028 = VERTEX_POINT ( 'NONE', #55017 ) ;
#87029 = CARTESIAN_POINT ( 'NONE',  ( -22.58250372949163420, -2.080990182559540269, -1.500000000000002220 ) ) ;
#87031 = VERTEX_POINT ( 'NONE', #85955 ) ;
#87030 = DIRECTION ( 'NONE',  ( -3.773278334453079618E-23, 0.9999999999976377785, 2.173523156925978705E-06 ) ) ;
#87032 = EDGE_CURVE ( 'NONE', #92497, #45676, #32239, .T. ) ;
#87033 = ORIENTED_EDGE ( 'NONE', *, *, #15686, .T. ) ;
#87034 = FACE_OUTER_BOUND ( 'NONE', #74462, .T. ) ;
#87035 = B_SPLINE_CURVE_WITH_KNOTS ( 'NONE', 3,
 ( #15818, #61517, #85840, #54398, #94452, #31548, #76701, #46277 ),
 .UNSPECIFIED., .F., .F.,
 ( 4, 2, 2, 4 ),
 ( 6.391158118973814098E-06, 0.002007136338672923983, 0.003007508928949901694, 0.004007881519226879838 ),
 .UNSPECIFIED. ) ;
#87036 = CARTESIAN_POINT ( 'NONE',  ( -10.68008619461380704, -17.10268970254769982, 11.49999999999998934 ) ) ;
#87037 = CARTESIAN_POINT ( 'NONE',  ( -84.52287095715006160, -23.47596703998600631, 11.44779298504228571 ) ) ;
#87038 = EDGE_LOOP ( 'NONE', ( #12038, #2216, #89437, #36641 ) ) ;
#87039 = CARTESIAN_POINT ( 'NONE',  ( -130.5728709571500303, -25.40560073940965324, 5.290910518220999670 ) ) ;
#87040 = CARTESIAN_POINT ( 'NONE',  ( 20.53814608839396527, -8.957171556794316203, -1.500000000000002220 ) ) ;
#87041 = ORIENTED_EDGE ( 'NONE', *, *, #64392, .T. ) ;
#87042 = ORIENTED_EDGE ( 'NONE', *, *, #30893, .F. ) ;
#87043 = CARTESIAN_POINT ( 'NONE',  ( -112.5553928173894036, -23.96169478059713498, 10.65365249895717170 ) ) ;
#87044 = CARTESIAN_POINT ( 'NONE',  ( -48.55620429048340014, -24.66019654487199020, 8.947790411086135265 ) ) ;
#87045 = CARTESIAN_POINT ( 'NONE',  ( -61.52287095715007581, -23.72773821059535848, 11.05748984161097326 ) ) ;
#87046 = AXIS2_PLACEMENT_3D ( 'NONE', #40728, #10278, #1170 ) ;
#87047 = LINE ( 'NONE', #57123, #48177 ) ;
#87049 = EDGE_CURVE ( 'NONE', #63165, #39828, #44998, .T. ) ;
#87048 = CARTESIAN_POINT ( 'NONE',  ( 16.30000000000000071, 0.000000000000000000, 0.000000000000000000 ) ) ;
#87050 = CARTESIAN_POINT ( 'NONE',  ( -19.49195742049215241, -1.735909528584683947, 11.49999999999998934 ) ) ;
#87051 = CARTESIAN_POINT ( 'NONE',  ( -46.51386545360935543, -23.73766607897669800, -1.055555164236460230 ) ) ;
#87052 = VERTEX_POINT ( 'NONE', #1229 ) ;
#87053 = CARTESIAN_POINT ( 'NONE',  ( 19.32660459246815421, -9.429101867163046435, -1.500000000000002220 ) ) ;
#87054 = VECTOR ( 'NONE', #312, 1000.000000000000000 ) ;
#87055 = CARTESIAN_POINT ( 'NONE',  ( -36.62287095715005592, -23.47593901973091235, -1.443836447539011525 ) ) ;
#87056 = DIRECTION ( 'NONE',  ( -0.000000000000000000, -0.000000000000000000, 1.000000000000000000 ) ) ;
#87057 = CARTESIAN_POINT ( 'NONE',  ( -123.5228709571500616, -23.48786465467242479, 11.44779295918253759 ) ) ;
#87058 = ADVANCED_FACE ( 'NONE', ( #6827 ), #61140, .T. ) ;
#87059 = DIRECTION ( 'NONE',  ( -3.773278334453080206E-23, 0.9999999999976377785, 2.173523156925979975E-06 ) ) ;
#87060 = CARTESIAN_POINT ( 'NONE',  ( 22.81499323874321661, -2.031749852351878882, -1.500000000000002220 ) ) ;
#87061 = PERSON_AND_ORGANIZATION ( #70597, #27821 ) ;
#87062 = CARTESIAN_POINT ( 'NONE',  ( -92.58953762381672448, -23.47593901973091235, -1.443836447539002865 ) ) ;
#87063 = CARTESIAN_POINT ( 'NONE',  ( -120.5228709571500616, -29.50248789122583659, 2.256150453626215580 ) ) ;
#87064 = CARTESIAN_POINT ( 'NONE',  ( -15.22981678846565856, -13.14137338692033907, 11.49999999999999645 ) ) ;
#87065 = CARTESIAN_POINT ( 'NONE',  ( -40.52287095715007581, -25.00182538069145011, 7.747789668545104647 ) ) ;
#87066 = PLANE ( 'NONE',  #88992 ) ;
#87067 = PRODUCT_DEFINITION_SHAPE ( 'NONE', 'NONE',  #14113 ) ;
#87068 = DIRECTION ( 'NONE',  ( 0.000000000000000000, -0.3081562241202470687, -0.9513357669802772199 ) ) ;
#87069 = CARTESIAN_POINT ( 'NONE',  ( -6.499999999999992895, 3.299745742347187193E-16, 2.100000000000000977 ) ) ;
#87070 = FACE_OUTER_BOUND ( 'NONE', #9360, .T. ) ;
#87071 = CARTESIAN_POINT ( 'NONE',  ( 17.96171645398845129, 8.431260308876343146, -1.500000000000002220 ) ) ;
#87072 = CARTESIAN_POINT ( 'NONE',  ( 21.40858030128615397, -3.853468400179685727, -1.500000000000002220 ) ) ;
#87073 = DIRECTION ( 'NONE',  ( -0.000000000000000000, 1.000000000000000000, -0.000000000000000000 ) ) ;
#87074 = CARTESIAN_POINT ( 'NONE',  ( 10.60981200654714307, 16.52409317135366607, -1.500000000000002220 ) ) ;
#87075 = AXIS2_PLACEMENT_3D ( 'NONE', #81442, #76665, #11921 ) ;
#87076 = CARTESIAN_POINT ( 'NONE',  ( -60.52287095715008292, -23.48783264082477018, -1.443836473390092801 ) ) ;
#87077 = CARTESIAN_POINT ( 'NONE',  ( -54.52287095715007581, -23.73934037231755667, 11.05740245334329330 ) ) ;
#87078 = CARTESIAN_POINT ( 'NONE',  ( -103.5228709571501042, -23.47593901973090524, -1.443836447538996204 ) ) ;
#87079 = LINE ( 'NONE', #48541, #34544 ) ;
#87080 = CARTESIAN_POINT ( 'NONE',  ( -20.17529555308526668, -4.016306826964139098, 11.49999999999999645 ) ) ;
#87081 = DIRECTION ( 'NONE',  ( -3.773278334444166432E-23, 1.000000000000000000, 0.000000000000000000 ) ) ;
#87082 = VECTOR ( 'NONE', #38450, 1000.000000000000000 ) ;
#87083 = CARTESIAN_POINT ( 'NONE',  ( -47.62287095715004881, -24.51283580621364777, 0.6167428607019750375 ) ) ;
#87084 = CARTESIAN_POINT ( 'NONE',  ( 14.59886444729927923, 17.24780449347180067, 11.49999999999999645 ) ) ;
#87085 = ORIENTED_EDGE ( 'NONE', *, *, #18957, .T. ) ;
#87086 = CARTESIAN_POINT ( 'NONE',  ( -99.93377387090225739, -25.31296416273143279, 4.577608519080482274 ) ) ;
#87087 = DIRECTION ( 'NONE',  ( -0.000000000000000000, 1.000000000000000000, -0.000000000000000000 ) ) ;
#87088 = CARTESIAN_POINT ( 'NONE',  ( -109.6228709571501128, -23.95044443724993144, 10.65354141964649592 ) ) ;
#87089 = CARTESIAN_POINT ( 'NONE',  ( -26.66703638657053688, -24.80367924758092002, 2.752295699766668324 ) ) ;
#87090 = VECTOR ( 'NONE', #28637, 1000.000000000000114 ) ;
#87091 = B_SPLINE_CURVE_WITH_KNOTS ( 'NONE', 3,
 ( #59443, #6140, #92374, #90880, #68057, #52824, #76636, #44714 ),
 .UNSPECIFIED., .F., .F.,
 ( 4, 2, 2, 4 ),
 ( 1.199502015590836694E-17, 0.001846270405096679841, 0.003692540810193348840, 0.007385081620386685537 ),
 .UNSPECIFIED. ) ;
#87092 = CARTESIAN_POINT ( 'NONE',  ( -50.62287095715005592, -25.00158670708909625, 2.256160236439165967 ) ) ;
#87093 = LINE ( 'NONE', #95211, #99826 ) ;
#87094 = ORIENTED_EDGE ( 'NONE', *, *, #76680, .T. ) ;
#87095 = CARTESIAN_POINT ( 'NONE',  ( 19.40787663092975279, -12.54570180764831377, 11.49999999999999645 ) ) ;
#87096 = CARTESIAN_POINT ( 'NONE',  ( -22.57016884136470125, -3.422276288085174478, 11.49999999999998934 ) ) ;
#87097 = FACE_OUTER_BOUND ( 'NONE', #73586, .T. ) ;
#87098 = CARTESIAN_POINT ( 'NONE',  ( -96.51590239563874718, -23.96119346886881019, -0.6495511937832061378 ) ) ;
#87099 = CARTESIAN_POINT ( 'NONE',  ( -63.58765420552874303, -24.35071581493543036, 9.817618358456027039 ) ) ;
#87100 = CARTESIAN_POINT ( 'NONE',  ( 19.77564376705174709, 10.73071584254150856, 11.49999999999999645 ) ) ;
#87101 = ORIENTED_EDGE ( 'NONE', *, *, #49918, .F. ) ;
#87102 = CARTESIAN_POINT ( 'NONE',  ( -43.59363013195762449, -24.15543982623907127, -0.2315651400026568496 ) ) ;
#87103 = CARTESIAN_POINT ( 'NONE',  ( 19.17116566557315949, -10.70166234769870961, 11.49999999999998934 ) ) ;
#87104 = CARTESIAN_POINT ( 'NONE',  ( -114.5228709571500616, -23.47596703998600631, 11.44779298504228038 ) ) ;
#87105 = CARTESIAN_POINT ( 'NONE',  ( -44.60008577590918577, -23.96169478059712787, 10.65365249895718414 ) ) ;
#87106 = CARTESIAN_POINT ( 'NONE',  ( -69.00489863181175565, -25.19577062647930177, 6.635084460666881512 ) ) ;
#87107 = ORIENTED_EDGE ( 'NONE', *, *, #9691, .F. ) ;
#87108 = CARTESIAN_POINT ( 'NONE',  ( -92.55620429048340725, -24.64898659630529210, 1.056161002820829919 ) ) ;
#87109 = CARTESIAN_POINT ( 'NONE',  ( -20.27875734969026311, 6.143225279485574397, 24.00402280011862288 ) ) ;
#87110 = ORIENTED_EDGE ( 'NONE', *, *, #15111, .F. ) ;
#87111 = EDGE_CURVE ( 'NONE', #38526, #61427, #69738, .T. ) ;
#87112 = CARTESIAN_POINT ( 'NONE',  ( -5.951451697817415010, -19.63005813332872762, 11.49999999999998934 ) ) ;
#87113 = ORIENTED_EDGE ( 'NONE', *, *, #61204, .F. ) ;
#87114 = ORIENTED_EDGE ( 'NONE', *, *, #69014, .T. ) ;
#87115 = VERTEX_POINT ( 'NONE', #33166 ) ;
#87116 = ORIENTED_EDGE ( 'NONE', *, *, #4444, .F. ) ;
#87117 = CARTESIAN_POINT ( 'NONE',  ( 8.651921485055520833, -21.43433228965458781, 11.49999999999998934 ) ) ;
#87118 = CARTESIAN_POINT ( 'NONE',  ( -41.52287095715005449, -23.73934037231755667, 11.05740245334329686 ) ) ;
#87119 = CARTESIAN_POINT ( 'NONE',  ( -16.58479117878708209, 11.75282063728064053, -1.500000000000002220 ) ) ;
#87120 = EDGE_CURVE ( 'NONE', #40372, #48919, #25726, .T. ) ;
#87121 = ORIENTED_EDGE ( 'NONE', *, *, #23191, .T. ) ;
#87122 = VECTOR ( 'NONE', #9891, 1000.000000000000114 ) ;
#87123 = CARTESIAN_POINT ( 'NONE',  ( -65.05438548721848235, -3.316774720514426456, 27.45402280011862572 ) ) ;
#87124 = CARTESIAN_POINT ( 'NONE',  ( -38.52287095715006870, -29.50250243563736774, 8.947779886222148704 ) ) ;
#87125 = EDGE_CURVE ( 'NONE', #2242, #88521, #79336, .T. ) ;
#87126 = CARTESIAN_POINT ( 'NONE',  ( -114.6228709571500559, -24.66019654487199730, 8.947790411086122830 ) ) ;
#87127 = CARTESIAN_POINT ( 'NONE',  ( 3.787259615384621192, -5.876774720514405637, 18.51923076923076295 ) ) ;
#87129 = ORIENTED_EDGE ( 'NONE', *, *, #64830, .T. ) ;
#87128 = CARTESIAN_POINT ( 'NONE',  ( -8.943896628894790979, 19.53434260886740503, 11.49999999999999645 ) ) ;
#87130 = CARTESIAN_POINT ( 'NONE',  ( -125.5228709571500616, -24.99132157543084531, 2.256160258750667502 ) ) ;
#87131 = CARTESIAN_POINT ( 'NONE',  ( -49.69311491917191148, -25.31573826004878569, 4.912235031306626531 ) ) ;
#87132 = ADVANCED_FACE ( 'NONE', ( #18938 ), #72244, .F. ) ;
#87133 = ORIENTED_EDGE ( 'NONE', *, *, #70845, .T. ) ;
#87134 = EDGE_CURVE ( 'NONE', #58829, #91753, #30421, .T. ) ;
#87135 = CARTESIAN_POINT ( 'NONE',  ( -1.268444833121266546, 20.69640364028325052, 11.49999999999998934 ) ) ;
#87136 = EDGE_LOOP ( 'NONE', ( #3285, #94240, #6638, #58677 ) ) ;
#87138 = EDGE_LOOP ( 'NONE', ( #91336, #67052, #88823, #49809 ) ) ;
#87137 = CARTESIAN_POINT ( 'NONE',  ( -125.6234887985724953, -25.00158670708911046, 2.256160236439218369 ) ) ;
#87139 = B_SPLINE_SURFACE_WITH_KNOTS ( 'NONE', 3, 1, ( 
 ( #35244, #74297 ),
 ( #11402, #51467 ),
 ( #97625, #35744 ),
 ( #50973, #96627 ),
 ( #42376, #82401 ),
 ( #67202, #4789 ),
 ( #28129, #3803 ),
 ( #34741, #5778 ),
 ( #92999, #99112 ),
 ( #84398, #7264 ),
 ( #29608, #14377 ),
 ( #46338, #98618 ),
 ( #36733, #61079 ),
 ( #53469, #69174 ),
 ( #82894, #92503 ) ),
 .UNSPECIFIED., .F., .F., .F.,
 ( 4, 1, 1, 1, 1, 1, 1, 1, 1, 1, 1, 1, 4 ),
 ( 2, 2 ),
 ( 0.000000000000000000, 0.08762222184221857280, 0.1714015232428990343, 0.2501655146837731269, 0.3257011369098756770, 0.3963425794403447888, 0.4627261202239039140, 0.5255277688564403693, 0.5841885094617105256, 0.6947236425220619793, 0.8002739465981734135, 0.9021818103852868864, 1.000000000000000000 ),
 ( 0.000000000000000000, 1.000000000000000000 ),
 .UNSPECIFIED. ) ;
#87140 = CARTESIAN_POINT ( 'NONE',  ( -77.52287095715004739, -23.94994826722564696, -0.6494450866342714734 ) ) ;
#87141 = CARTESIAN_POINT ( 'NONE',  ( -28.98875734969026041, 5.965225279485572685, -0.08597719988137116076 ) ) ;
#87142 = ORIENTED_EDGE ( 'NONE', *, *, #67143, .T. ) ;
#87143 = VERTEX_POINT ( 'NONE', #86953 ) ;
#87144 = CARTESIAN_POINT ( 'NONE',  ( -6.265203266387573855, -5.876774720514408301, 19.29154511076646017 ) ) ;
#87145 = DIRECTION ( 'NONE',  ( 0.000000000000000000, -0.9999999999976377785, -2.173523156925979128E-06 ) ) ;
#87146 = EDGE_CURVE ( 'NONE', #5411, #78009, #17687, .T. ) ;
#87147 = CARTESIAN_POINT ( 'NONE',  ( -29.81175120719462512, -25.25636103033882307, 4.942810967025194735 ) ) ;
#87149 = VERTEX_POINT ( 'NONE', #72746 ) ;
#87148 = CARTESIAN_POINT ( 'NONE',  ( -0.4018715335629812202, -22.01094342083549193, 11.49999999999999645 ) ) ;
#87150 = CARTESIAN_POINT ( 'NONE',  ( -103.5477577631356354, -24.65952944569305316, 1.056160979905703234 ) ) ;
#87151 = CARTESIAN_POINT ( 'NONE',  ( 11.79716412695777272, 19.27136520130675024, 11.49999999999998934 ) ) ;
#87152 = AXIS2_PLACEMENT_3D ( 'NONE', #33149, #59494, #90932 ) ;
#87153 = CARTESIAN_POINT ( 'NONE',  ( 14.98681507544721292, -14.71779577663021321, 11.49999999999998934 ) ) ;
#87155 = VERTEX_POINT ( 'NONE', #2236 ) ;
#87154 = DIRECTION ( 'NONE',  ( 0.4771587602595988020, 0.8788171126619706008, -0.000000000000000000 ) ) ;
#87156 = ORIENTED_EDGE ( 'NONE', *, *, #95826, .T. ) ;
#87157 = CARTESIAN_POINT ( 'NONE',  ( -5.366453405989239478, 14.49999999999999645, 12.73734666247253244 ) ) ;
#87158 = CIRCLE ( 'NONE', #40152, 2.399999999999999911 ) ;
#87159 = DIRECTION ( 'NONE',  ( -0.000000000000000000, 2.173523156925979552E-06, -0.9999999999976378895 ) ) ;
#87160 = ORIENTED_EDGE ( 'NONE', *, *, #78625, .F. ) ;
#87161 = CARTESIAN_POINT ( 'NONE',  ( 8.100108036306837178, -19.54698220168213041, 11.49999999999998934 ) ) ;
#87162 = DIRECTION ( 'NONE',  ( 0.000000000000000000, 0.000000000000000000, -1.000000000000000000 ) ) ;
#87163 = CARTESIAN_POINT ( 'NONE',  ( -51.90898564286461436, -25.03148495602775725, 6.429377976798327232 ) ) ;
#87164 = CIRCLE ( 'NONE', #61250, 84.48086791635431325 ) ;
#87165 = CARTESIAN_POINT ( 'NONE',  ( -125.6228709571500275, -23.84047902841601640, -0.8780736468305819775 ) ) ;
#87166 = FACE_OUTER_BOUND ( 'NONE', #39187, .T. ) ;
#87167 = CARTESIAN_POINT ( 'NONE',  ( 20.56832688555235222, -8.368550285707721414, -1.500000000000002220 ) ) ;
#87168 = CARTESIAN_POINT ( 'NONE',  ( -114.5873130560532900, -24.65952944569305316, 1.056160979905706343 ) ) ;
#87169 = B_SPLINE_CURVE_WITH_KNOTS ( 'NONE', 3,
 ( #39126, #31516, #23384, #86307, #92907, #16792 ),
 .UNSPECIFIED., .F., .F.,
 ( 4, 2, 4 ),
 ( 6.391158118952235087E-06, 0.001387004593080770317, 0.002767618028042588118 ),
 .UNSPECIFIED. ) ;
#87170 = EDGE_CURVE ( 'NONE', #76269, #33339, #57527, .T. ) ;
#87171 = ORIENTED_EDGE ( 'NONE', *, *, #12441, .F. ) ;
#87172 = CARTESIAN_POINT ( 'NONE',  ( 13.43165536947796213, -3.316774720514427344, -28.18099828186571187 ) ) ;
#87173 = CARTESIAN_POINT ( 'NONE',  ( -48.62287095715004881, -23.72747288104441310, -1.053458166803663332 ) ) ;
#87174 = CARTESIAN_POINT ( 'NONE',  ( -17.66094656686658482, 7.961706694365092041, 11.49999999999999645 ) ) ;
#87175 = CARTESIAN_POINT ( 'NONE',  ( -122.6228709571500417, -29.50248528299804818, 1.056150453629045360 ) ) ;
#87176 = DIRECTION ( 'NONE',  ( 0.000000000000000000, 1.000000000000000000, 0.000000000000000000 ) ) ;
#87177 = CARTESIAN_POINT ( 'NONE',  ( -8.384790838521158918, 17.58144419890746235, 11.49999999999998934 ) ) ;
#87178 = CARTESIAN_POINT ( 'NONE',  ( -5.333777546869826303, -20.73983961313815172, 11.49999999999998934 ) ) ;
#87179 = CARTESIAN_POINT ( 'NONE',  ( -85.52287095715006160, -24.82576562948883492, 8.398263436605596155 ) ) ;
#87180 = CARTESIAN_POINT ( 'NONE',  ( 0.000000000000000000, -2.056774720514426669, 0.000000000000000000 ) ) ;
#87181 = CARTESIAN_POINT ( 'NONE',  ( -51.65966576824040146, -23.48783264082476308, -1.443836473390094133 ) ) ;
#87182 = CARTESIAN_POINT ( 'NONE',  ( -52.62287095715005592, -29.50248528299804818, 1.056150453629033370 ) ) ;
#87183 = CARTESIAN_POINT ( 'NONE',  ( -2.506051680461856890, -22.62920675306992280, -1.500000000000002220 ) ) ;
#87184 = EDGE_CURVE ( 'NONE', #65117, #80623, #35296, .T. ) ;
#87185 = CARTESIAN_POINT ( 'NONE',  ( 0.000000000000000000, 0.000000000000000000, 0.000000000000000000 ) ) ;
#87186 = DIRECTION ( 'NONE',  ( -1.000000000000000000, -3.773278334444167608E-23, -8.201307833595939069E-29 ) ) ;
#87187 = CARTESIAN_POINT ( 'NONE',  ( -98.62287095715004170, -23.73907113216990794, -1.053371485793225704 ) ) ;
#87188 = CARTESIAN_POINT ( 'NONE',  ( -19.77004505525285083, 2.005399880840008642, 11.49999999999999645 ) ) ;
#87189 = CARTESIAN_POINT ( 'NONE',  ( 5.963731207934512391, -6.376774720514413630, 19.80418863844947097 ) ) ;
#87190 = CARTESIAN_POINT ( 'NONE',  ( 6.660000000000001030, -5.396855673853237919E-16, 5.288828319098142217 ) ) ;
#87191 = DIRECTION ( 'NONE',  ( 0.000000000000000000, -0.000000000000000000, 1.000000000000000000 ) ) ;
#87192 = EDGE_LOOP ( 'NONE', ( #36377, #43292, #568, #4121 ) ) ;
#87193 = PLANE ( 'NONE',  #91458 ) ;
#87194 = EDGE_CURVE ( 'NONE', #5560, #43445, #94576, .T. ) ;
#87195 = CARTESIAN_POINT ( 'NONE',  ( -80.52287095715007581, -24.14406661686764366, 10.28769366194071821 ) ) ;
#87196 = DIRECTION ( 'NONE',  ( 0.000000000000000000, 0.000000000000000000, 1.000000000000000000 ) ) ;
#87197 = CARTESIAN_POINT ( 'NONE',  ( -20.76051858633888259, -6.224802954461835292, -1.500000000000002220 ) ) ;
#87198 = CARTESIAN_POINT ( 'NONE',  ( -56.61228501525301482, -23.48786465467241413, 11.44779295918254647 ) ) ;
#87199 = CARTESIAN_POINT ( 'NONE',  ( 4.201609111248720829, -18.99613120386805676, -1.500000000000002220 ) ) ;
#87200 = DIRECTION ( 'NONE',  ( 0.000000000000000000, 1.000000000000000000, 0.000000000000000000 ) ) ;
#87201 = VERTEX_POINT ( 'NONE', #56526 ) ;
#87202 = CARTESIAN_POINT ( 'NONE',  ( -10.01004151551622456, -17.79114453763541093, 11.49999999999999645 ) ) ;
#87203 = CARTESIAN_POINT ( 'NONE',  ( -49.52287095715006160, -23.47596703998600631, 11.44779298504229104 ) ) ;
#87204 = CC_DESIGN_DATE_AND_TIME_ASSIGNMENT ( #59762, #74954, ( #83064 ) ) ;
#87205 = CARTESIAN_POINT ( 'NONE',  ( 23.50000000000000000, -0.9000000000000000222, 1.103411337323757735 ) ) ;
#87206 = ORIENTED_EDGE ( 'NONE', *, *, #60330, .T. ) ;
#87207 = FACE_OUTER_BOUND ( 'NONE', #42224, .T. ) ;
#87208 = CARTESIAN_POINT ( 'NONE',  ( 33.62498039647005044, 3.398310449796175359, -11.43903334458933507 ) ) ;
#87209 = CARTESIAN_POINT ( 'NONE',  ( -39.06913928595307084, -25.31628511282779925, 4.503859277642591863 ) ) ;
#87210 = FACE_OUTER_BOUND ( 'NONE', #54692, .T. ) ;
#87211 = CARTESIAN_POINT ( 'NONE',  ( -1.036876607668611117, -6.376774720514417183, 20.14881673916291405 ) ) ;
#87212 = CARTESIAN_POINT ( 'NONE',  ( -28.32169924589829080, 0.3587747205143964613, -8.244178532169451401 ) ) ;
#87213 = ORIENTED_EDGE ( 'NONE', *, *, #14388, .T. ) ;
#87214 = CARTESIAN_POINT ( 'NONE',  ( -66.62726695432588997, -24.51419770103157347, 9.386484678747176957 ) ) ;
#87215 = VECTOR ( 'NONE', #97672, 1000.000000000000000 ) ;
#87216 = CARTESIAN_POINT ( 'NONE',  ( -9.034649315346676701, 21.08484869742704504, 11.49999999999999645 ) ) ;
#87217 = CARTESIAN_POINT ( 'NONE',  ( 22.46337926046256328, 3.617889471270266277, -1.500000000000002220 ) ) ;
#87218 = ORIENTED_EDGE ( 'NONE', *, *, #62982, .T. ) ;
#87219 = CARTESIAN_POINT ( 'NONE',  ( -110.5116820962086592, -24.83644354573579349, 8.397322867130096569 ) ) ;
#87220 = CARTESIAN_POINT ( 'NONE',  ( -98.52287095715001897, -24.34917612406837151, 0.1852690917426555450 ) ) ;
#87221 = CARTESIAN_POINT ( 'NONE',  ( -123.5562042904833788, -24.66019654487199730, 8.947790411086119278 ) ) ;
#87222 = CARTESIAN_POINT ( 'NONE',  ( -73.52287095715010423, -23.48783264082477018, -1.443836473390093689 ) ) ;
#87223 = B_SPLINE_CURVE_WITH_KNOTS ( 'NONE', 3,
 ( #29032, #60511, #90936, #91425 ),
 .UNSPECIFIED., .F., .F.,
 ( 4, 4 ),
 ( 0.000000000000000000, 9.999999999998897304E-05 ),
 .UNSPECIFIED. ) ;
#87224 = CARTESIAN_POINT ( 'NONE',  ( -74.52287095715006160, -24.50216790748204687, 0.6166512839542546143 ) ) ;
#87225 = CARTESIAN_POINT ( 'NONE',  ( -27.61288548982546232, -24.76667042481958703, 2.278808687314067161 ) ) ;
#87226 = CARTESIAN_POINT ( 'NONE',  ( 22.02124265030973760, -6.376774720514428729, 16.20402280011862217 ) ) ;
#87227 = CARTESIAN_POINT ( 'NONE',  ( 30.43908124610670285, 1.477225279485574028, -13.86910542224428866 ) ) ;
#87228 = EDGE_LOOP ( 'NONE', ( #17982, #88625, #18691, #61940 ) ) ;
#87229 = CARTESIAN_POINT ( 'NONE',  ( 4.102729645046709450, 19.96921287702725323, 11.49999999999998934 ) ) ;
#87230 = EDGE_LOOP ( 'NONE', ( #83742, #68086, #20745, #38054 ) ) ;
#87231 = VERTEX_POINT ( 'NONE', #87458 ) ;
#87232 = CARTESIAN_POINT ( 'NONE',  ( -22.84742429131147645, -2.885717679200183738, -1.500000000000002220 ) ) ;
#87233 = CARTESIAN_POINT ( 'NONE',  ( -99.62287095715004170, -24.66019654487199730, 8.947790411086122830 ) ) ;
#87234 = ORIENTED_EDGE ( 'NONE', *, *, #86913, .F. ) ;
#87235 = CARTESIAN_POINT ( 'NONE',  ( -65.05438548721848235, 5.356774720514425603, 0.7300228001186309656 ) ) ;
#87236 = CARTESIAN_POINT ( 'NONE',  ( -101.5228709571500758, -23.72747288104470087, -1.053458166803225460 ) ) ;
#87237 = B_SPLINE_CURVE_WITH_KNOTS ( 'NONE', 3,
 ( #16034, #821, #31774, #76428 ),
 .UNSPECIFIED., .F., .F.,
 ( 4, 4 ),
 ( 0.8704074611401169115, 0.8794138924122323342 ),
 .UNSPECIFIED. ) ;
#87238 = CARTESIAN_POINT ( 'NONE',  ( -95.59855702225377172, -23.85016227208581086, -0.8807180028928282001 ) ) ;
#87239 = CARTESIAN_POINT ( 'NONE',  ( -29.55620429048340725, -24.57875649265860574, 1.056161290661043584 ) ) ;
#87240 = VECTOR ( 'NONE', #67257, 1000.000000000000114 ) ;
#87242 = ORIENTED_EDGE ( 'NONE', *, *, #67093, .T. ) ;
#87241 = CARTESIAN_POINT ( 'NONE',  ( -20.89022842043660688, 4.291957016416017900, 11.49999999999999645 ) ) ;
#87243 = EDGE_CURVE ( 'NONE', #49692, #83380, #89736, .T. ) ;
#87244 = ORIENTED_EDGE ( 'NONE', *, *, #1557, .T. ) ;
#87245 = CARTESIAN_POINT ( 'NONE',  ( 10.78255534502030777, 19.45608938089507234, 11.49999999999998934 ) ) ;
#87246 = EDGE_CURVE ( 'NONE', #22752, #64178, #34966, .T. ) ;
#87247 = CARTESIAN_POINT ( 'NONE',  ( 14.37238272058661259, 14.81585024043302035, -1.500000000000002220 ) ) ;
#87248 = VERTEX_POINT ( 'NONE', #55424 ) ;
#87249 = CARTESIAN_POINT ( 'NONE',  ( -0.7395115731254272573, 18.09566585216508727, 8.999999999999998224 ) ) ;
#87250 = CARTESIAN_POINT ( 'NONE',  ( -56.62287095715005592, -23.48783264082478084, -1.443836473390068820 ) ) ;
#87251 = EDGE_LOOP ( 'NONE', ( #59823, #19215, #38238, #26855 ) ) ;
#87252 = CARTESIAN_POINT ( 'NONE',  ( -95.52287095715004739, -24.62226745350443124, 0.9660975649729501846 ) ) ;
#87253 = ORIENTED_EDGE ( 'NONE', *, *, #97852, .T. ) ;
#87254 = CARTESIAN_POINT ( 'NONE',  ( -58.55986427732528199, -23.73791477778912196, 11.05961554403170588 ) ) ;
#87255 = PLANE ( 'NONE',  #61737 ) ;
#87256 = CARTESIAN_POINT ( 'NONE',  ( 17.92008016455634589, 10.74458801173053324, -1.500000000000002220 ) ) ;
#87257 = EDGE_CURVE ( 'NONE', #18015, #53541, #75161, .T. ) ;
#87258 = CARTESIAN_POINT ( 'NONE',  ( 12.52028139621776326, 17.89958603277719718, 11.49999999999999645 ) ) ;
#87259 = DIRECTION ( 'NONE',  ( 0.000000000000000000, 1.000000000000000000, -0.000000000000000000 ) ) ;
#87260 = FACE_OUTER_BOUND ( 'NONE', #79619, .T. ) ;
#87261 = CARTESIAN_POINT ( 'NONE',  ( 0.003324065884441271702, 22.49086686382009503, 11.49999999999998934 ) ) ;
#87262 = CARTESIAN_POINT ( 'NONE',  ( -8.544475976622297964, 19.10969517993760292, -1.500000000000002220 ) ) ;
#87263 = CARTESIAN_POINT ( 'NONE',  ( -62.52287095715006160, -24.64898659630367561, 1.056161002820822592 ) ) ;
#87264 = DIRECTION ( 'NONE',  ( 0.9976052577199501226, 0.000000000000000000, 0.06916465693916179491 ) ) ;
#87265 = CARTESIAN_POINT ( 'NONE',  ( 4.465438306463536122, -5.876774720514426065, 21.59631214011467293 ) ) ;
#87266 = ORIENTED_EDGE ( 'NONE', *, *, #4430, .F. ) ;
#87267 = ORIENTED_EDGE ( 'NONE', *, *, #57693, .F. ) ;
#87268 = ORIENTED_EDGE ( 'NONE', *, *, #45236, .T. ) ;
#87269 = CARTESIAN_POINT ( 'NONE',  ( -52.58733020142698678, -24.34968618360933945, 0.1864209137778880532 ) ) ;
#87270 = ORIENTED_EDGE ( 'NONE', *, *, #27562, .F. ) ;
#87271 = CARTESIAN_POINT ( 'NONE',  ( 16.24497012180664868, 13.92215130028523973, -1.500000000000002220 ) ) ;
#87272 = CARTESIAN_POINT ( 'NONE',  ( -13.11617634606977489, 18.14055439154125438, 11.49999999999999645 ) ) ;
#87273 = VERTEX_POINT ( 'NONE', #96861 ) ;
#87274 = PLANE ( 'NONE',  #26190 ) ;
#87275 = CARTESIAN_POINT ( 'NONE',  ( 20.41947327098772647, -5.118016103960565388, 11.49999999999998934 ) ) ;
#87276 = CARTESIAN_POINT ( 'NONE',  ( -30.42977181688026533, -24.56940358145610048, 9.174392229302920754 ) ) ;
#87277 = CARTESIAN_POINT ( 'NONE',  ( -2.986242917674419850, -19.73498743542299749, -1.500000000000002220 ) ) ;
#87278 = CARTESIAN_POINT ( 'NONE',  ( -8.599999999999997868, 24.84999999999999787, 2.100000000000000089 ) ) ;
#87279 = CARTESIAN_POINT ( 'NONE',  ( -101.5105966293721877, -24.51314013834316086, 0.6176544820404185065 ) ) ;
#87280 = CARTESIAN_POINT ( 'NONE',  ( -17.89045161427552699, -12.92718102017995641, -1.500000000000002220 ) ) ;
#87281 = ORIENTED_EDGE ( 'NONE', *, *, #79212, .T. ) ;
#87282 = B_SPLINE_CURVE_WITH_KNOTS ( 'NONE', 3,
 ( #58080, #28112, #20977, #35728, #42851, #65699, #96613, #4773, #34232, #65205, #26615, #50957 ),
 .UNSPECIFIED., .F., .F.,
 ( 4, 2, 2, 2, 2, 4 ),
 ( 0.000000000000000000, 0.0003036893844903788245, 0.0006073787689807576490, 0.0009110681534711365277, 0.001062912845716322335, 0.001214757537961508359 ),
 .UNSPECIFIED. ) ;
#87283 = CARTESIAN_POINT ( 'NONE',  ( -65.62787617961251385, -24.83644354573579349, 8.397322867130094792 ) ) ;
#87284 = DIRECTION ( 'NONE',  ( -3.773278334453079618E-23, 0.9999999999976377785, 2.173523156925979975E-06 ) ) ;
#87285 = CARTESIAN_POINT ( 'NONE',  ( 4.135342931496230001, -20.44547621892628797, 11.49999999999999645 ) ) ;
#87286 = VECTOR ( 'NONE', #36649, 1000.000000000000000 ) ;
#87287 = ADVANCED_FACE ( 'NONE', ( #12620 ), #57818, .T. ) ;
#87288 = CARTESIAN_POINT ( 'NONE',  ( -47.52287095715007581, -23.72747288104469732, -1.053458166803227236 ) ) ;
#87289 = CARTESIAN_POINT ( 'NONE',  ( -25.57936158321581033, -24.88095430358513838, 4.018852390678397057 ) ) ;
#87291 = CARTESIAN_POINT ( 'NONE',  ( -117.5228709571500474, -24.51283580621365843, 0.6167428607019750375 ) ) ;
#87290 = AXIS2_PLACEMENT_3D ( 'NONE', #79332, #48904, #47899 ) ;
#87292 = CARTESIAN_POINT ( 'NONE',  ( -13.37813101364405100, 16.61575060780308277, -1.500000000000002220 ) ) ;
#87293 = CARTESIAN_POINT ( 'NONE',  ( 30.09341516180546350, -1.682774720514426114, -11.39311774897855933 ) ) ;
#87294 = CARTESIAN_POINT ( 'NONE',  ( 30.53060340732036337, 5.340035977923285770, 2.705756132044150775 ) ) ;
#87295 = ADVANCED_FACE ( 'NONE', ( #86853 ), #4020, .T. ) ;
#87296 = CARTESIAN_POINT ( 'NONE',  ( -83.62287095715005592, -23.48783264082478794, -1.443836473390065711 ) ) ;
#87297 = CARTESIAN_POINT ( 'NONE',  ( -5.382328594919684406, -5.876774720514414518, 19.61227901093090864 ) ) ;
#87298 = CARTESIAN_POINT ( 'NONE',  ( 1.525329354412473970, -22.51392980886878448, -1.500000000000002220 ) ) ;
#87299 = DIRECTION ( 'NONE',  ( -2.504262461560503878E-15, -0.000000000000000000, -1.000000000000000000 ) ) ;
#87300 = EDGE_LOOP ( 'NONE', ( #51593, #33202, #87405, #98587 ) ) ;
#87301 = CARTESIAN_POINT ( 'NONE',  ( -111.3776484685884327, -29.50249240399202222, 4.332395270848422797 ) ) ;
#87302 = CARTESIAN_POINT ( 'NONE',  ( 0.000000000000000000, -4.056774720514426669, -1.399999999999999911 ) ) ;
#87303 = CARTESIAN_POINT ( 'NONE',  ( 3.669390655483735220, -19.36157329643844704, 11.49999999999999645 ) ) ;
#87304 = CARTESIAN_POINT ( 'NONE',  ( -32.52287095715004739, -23.47593901973090169, -1.443836447538997092 ) ) ;
#87305 = AXIS2_PLACEMENT_3D ( 'NONE', #96326, #35435, #95822 ) ;
#87306 = B_SPLINE_CURVE_WITH_KNOTS ( 'NONE', 3,
 ( #96952, #52281, #44171, #98432, #36544, #21806 ),
 .UNSPECIFIED., .F., .F.,
 ( 4, 2, 4 ),
 ( 0.000000000000000000, 0.001380764517853250552, 0.002761529035706501104 ),
 .UNSPECIFIED. ) ;
#87307 = CARTESIAN_POINT ( 'NONE',  ( 5.395440699609681090, 0.3587747205144061202, -28.51842087987364849 ) ) ;
#87308 = ORIENTED_EDGE ( 'NONE', *, *, #56908, .F. ) ;
#87309 = CARTESIAN_POINT ( 'NONE',  ( -89.52287095715006160, -23.47596703998600631, 11.44779298504228393 ) ) ;
#87310 = DIRECTION ( 'NONE',  ( 0.000000000000000000, 0.000000000000000000, -1.000000000000000000 ) ) ;
#87311 = CARTESIAN_POINT ( 'NONE',  ( -124.5569032301564363, -23.48786465467241769, 11.44779295918253581 ) ) ;
#87312 = CARTESIAN_POINT ( 'NONE',  ( -76.62287095715007013, -24.64898659630367916, 1.056161002820826145 ) ) ;
#87313 = DIRECTION ( 'NONE',  ( -0.000000000000000000, -1.000000000000000000, -0.000000000000000000 ) ) ;
#87314 = DIRECTION ( 'NONE',  ( 1.000000000000000000, 3.773278334444167608E-23, 8.201307833595939069E-29 ) ) ;
#87315 = CARTESIAN_POINT ( 'NONE',  ( 6.816645498261984848, 18.52099371530728789, 11.49999999999998934 ) ) ;
#87316 = ORIENTED_EDGE ( 'NONE', *, *, #51205, .F. ) ;
#87317 = CARTESIAN_POINT ( 'NONE',  ( 16.36621611169882229, 11.82581248522330064, 11.49999999999999645 ) ) ;
#87318 = DIRECTION ( 'NONE',  ( 0.000000000000000000, 0.000000000000000000, 1.000000000000000000 ) ) ;
#87319 = EDGE_CURVE ( 'NONE', #43640, #45268, #58314, .T. ) ;
#87320 = CLOSED_SHELL ( 'NONE', ( #96194, #82411, #46925, #93054, #4089, #89341, #80866, #97295, #33625, #54493, #62648, #50036, #11393, #72715, #26212, #619, #94374, #46519, #55165, #94490, #52116, #92098, #51735, #55882, #33738, #94342, #94765, #65503, #11560, #62149, #292, #74568, #6117, #100402, #64761, #63546, #56481, #86427, #76232, #64702, #47670 ) ) ;
#87321 = ORIENTED_EDGE ( 'NONE', *, *, #14979, .T. ) ;
#87322 = LINE ( 'NONE', #34549, #483 ) ;
#87323 = CARTESIAN_POINT ( 'NONE',  ( -41.62287095715006302, -23.47596703998600276, 11.44779298504227505 ) ) ;
#87324 = DIRECTION ( 'NONE',  ( 1.000000000000000000, 0.000000000000000000, -0.000000000000000000 ) ) ;
#87325 = CARTESIAN_POINT ( 'NONE',  ( -82.62287095715005592, -23.72747288104469376, -1.053458166803226792 ) ) ;
#87326 = CARTESIAN_POINT ( 'NONE',  ( 10.75273025779354796, -5.876774720514426953, 23.03521261039436752 ) ) ;
#87327 = CARTESIAN_POINT ( 'NONE',  ( -81.55620429048340725, -24.65952944569304606, 1.056160979905699238 ) ) ;
#87328 = CARTESIAN_POINT ( 'NONE',  ( -19.63739455291241498, 3.909132673056371132, -1.500000000000002220 ) ) ;
#87329 = LINE ( 'NONE', #9201, #80725 ) ;
#87330 = DIRECTION ( 'NONE',  ( 3.773278334444166432E-23, -1.000000000000000000, 0.000000000000000000 ) ) ;
#87331 = ORIENTED_EDGE ( 'NONE', *, *, #30397, .F. ) ;
#87332 = EDGE_CURVE ( 'NONE', #75504, #98076, #34024, .T. ) ;
#87333 = CARTESIAN_POINT ( 'NONE',  ( -79.63359060245308285, -24.15620529776628089, 10.23563542870660470 ) ) ;
#87334 = CARTESIAN_POINT ( 'NONE',  ( 32.66876533700883556, -6.475225279485573360, -12.58926540598386445 ) ) ;
#87335 = DIRECTION ( 'NONE',  ( -1.000000000000000000, -3.773278334444166432E-23, -8.201307841325785021E-29 ) ) ;
#87336 = CARTESIAN_POINT ( 'NONE',  ( -38.52287095715008292, -23.48783264083452593, -1.443836473374935592 ) ) ;
#87337 = CARTESIAN_POINT ( 'NONE',  ( -73.51656568446136930, -23.73766607897670511, -1.055555164236457344 ) ) ;
#87338 = DIRECTION ( 'NONE',  ( -3.773278334453080206E-23, 0.9999999999976377785, 2.173523156925979975E-06 ) ) ;
#87339 = DIRECTION ( 'NONE',  ( 0.000000000000000000, -0.9999999999976377785, -2.173523156925979975E-06 ) ) ;
#87340 = ORIENTED_EDGE ( 'NONE', *, *, #53927, .T. ) ;
#87341 = AXIS2_PLACEMENT_3D ( 'NONE', #28316, #83591, #28820 ) ;
#87342 = CIRCLE ( 'NONE', #29033, 253.2618649670780826 ) ;
#87343 = CARTESIAN_POINT ( 'NONE',  ( 20.05691770114479766, 3.104179615465487707, -1.500000000000002220 ) ) ;
#87344 = EDGE_CURVE ( 'NONE', #47463, #73040, #24956, .T. ) ;
#87345 = EDGE_CURVE ( 'NONE', #36941, #25228, #89251, .T. ) ;
#87346 = B_SPLINE_CURVE_WITH_KNOTS ( 'NONE', 3,
 ( #63612, #70701, #85417, #1199, #9802, #86921 ),
 .UNSPECIFIED., .F., .F.,
 ( 4, 2, 4 ),
 ( 0.000000000000000000, 0.001380764517854764098, 0.002761529035709528197 ),
 .UNSPECIFIED. ) ;
#87347 = CARTESIAN_POINT ( 'NONE',  ( -109.5228709571500474, -23.48783264082477018, -1.443836473390083253 ) ) ;
#87348 = CARTESIAN_POINT ( 'NONE',  ( -127.5894455380119865, -24.51419770103158768, 9.386484678747160970 ) ) ;
#87349 = VECTOR ( 'NONE', #46952, 1000.000000000000114 ) ;
#87350 = CARTESIAN_POINT ( 'NONE',  ( -88.62287095715004170, -23.48786465467241769, 11.44779295918254114 ) ) ;
#87351 = CARTESIAN_POINT ( 'NONE',  ( -81.62287095715007013, -23.73907113216990794, -1.053371485793228368 ) ) ;
#87352 = CARTESIAN_POINT ( 'NONE',  ( -30.47287095715006444, -24.91388280771538533, 8.081096783492887070 ) ) ;
#87353 = CARTESIAN_POINT ( 'NONE',  ( -6.202713861520617655, -20.23501359363181962, 11.49999999999999645 ) ) ;
#87354 = B_SPLINE_CURVE_WITH_KNOTS ( 'NONE', 3,
 ( #73959, #3461, #43514, #42525 ),
 .UNSPECIFIED., .F., .F.,
 ( 4, 4 ),
 ( 0.000000000000000000, 9.999999999998897304E-05 ),
 .UNSPECIFIED. ) ;
#87355 = CONICAL_SURFACE ( 'NONE', #98650, 1.249999999999996003, 0.7853981633974514986 ) ;
#87356 = CARTESIAN_POINT ( 'NONE',  ( 21.55033589006239936, 5.121329677682045833, -1.500000000000002220 ) ) ;
#87357 = ADVANCED_FACE ( 'NONE', ( #80638 ), #81639, .F. ) ;
#87358 = CARTESIAN_POINT ( 'NONE',  ( -18.72588118538106272, -8.511115862834014223, 11.49999999999998934 ) ) ;
#87359 = ORIENTED_EDGE ( 'NONE', *, *, #38789, .T. ) ;
#87360 = CARTESIAN_POINT ( 'NONE',  ( -88.52287095715009002, -23.48783264082477018, -1.443836473390089692 ) ) ;
#87361 = ORIENTED_EDGE ( 'NONE', *, *, #53700, .T. ) ;
#87362 = EDGE_CURVE ( 'NONE', #44716, #62727, #74028, .T. ) ;
#87363 = FACE_OUTER_BOUND ( 'NONE', #36670, .T. ) ;
#87364 = CARTESIAN_POINT ( 'NONE',  ( -70.52287095715009002, -24.62285846331437256, 9.038163153548294915 ) ) ;
#87365 = ORIENTED_EDGE ( 'NONE', *, *, #38202, .F. ) ;
#87366 = EDGE_LOOP ( 'NONE', ( #97016, #26723, #98634, #45569 ) ) ;
#87367 = AXIS2_PLACEMENT_3D ( 'NONE', #47566, #46555, #31832 ) ;
#87368 = ORIENTED_EDGE ( 'NONE', *, *, #5143, .T. ) ;
#87369 = CARTESIAN_POINT ( 'NONE',  ( -117.5228709571500758, -23.47593901973090524, -1.443836447538996204 ) ) ;
#87370 = CARTESIAN_POINT ( 'NONE',  ( -80.62287095715005592, -29.50250786944525672, 11.44777988621623521 ) ) ;
#87371 = CARTESIAN_POINT ( 'NONE',  ( 5.329826657887789310, -5.876774720514418071, 20.66144943787464783 ) ) ;
#87372 = CARTESIAN_POINT ( 'NONE',  ( -17.23291202157775359, 11.51834372740795231, -1.500000000000002220 ) ) ;
#87373 = EDGE_CURVE ( 'NONE', #62610, #55233, #97364, .T. ) ;
#87374 = CARTESIAN_POINT ( 'NONE',  ( -21.36891742734480104, 3.643610035731704055, 11.49999999999999645 ) ) ;
#87375 = ORIENTED_EDGE ( 'NONE', *, *, #53589, .F. ) ;
#87376 = CARTESIAN_POINT ( 'NONE',  ( -127.5562042904834215, -24.65952944569304606, 1.056160979905708563 ) ) ;
#87377 = DIRECTION ( 'NONE',  ( -0.000000000000000000, 1.000000000000000000, -0.000000000000000000 ) ) ;
#87378 = CARTESIAN_POINT ( 'NONE',  ( -3.217810451210200817, -22.18463865543611391, 11.49999999999998934 ) ) ;
#87379 = ADVANCED_FACE ( 'NONE', ( #6005 ), #59304, .T. ) ;
#87380 = CARTESIAN_POINT ( 'NONE',  ( -47.60695248165256288, -23.73791477778911485, 11.05961554403170766 ) ) ;
#87381 = CARTESIAN_POINT ( 'NONE',  ( -123.5228709571500616, -24.65952944569304961, 1.056160979905705899 ) ) ;
#87382 = ORIENTED_EDGE ( 'NONE', *, *, #16675, .T. ) ;
#87383 = DIRECTION ( 'NONE',  ( -1.000000000000000000, 0.000000000000000000, -0.000000000000000000 ) ) ;
#87384 = CARTESIAN_POINT ( 'NONE',  ( 23.07151214508650128, 3.625915217019311583E-15, -1.699999999999999956 ) ) ;
#87385 = ORIENTED_EDGE ( 'NONE', *, *, #27378, .F. ) ;
#87386 = ORIENTED_EDGE ( 'NONE', *, *, #38154, .F. ) ;
#87387 = CARTESIAN_POINT ( 'NONE',  ( -45.52287095715006870, -23.84081130425358097, 10.88220057483157888 ) ) ;
#87388 = ORIENTED_EDGE ( 'NONE', *, *, #69839, .T. ) ;
#87389 = AXIS2_PLACEMENT_3D ( 'NONE', #586, #23919, #69094 ) ;
#87390 = B_SPLINE_CURVE_WITH_KNOTS ( 'NONE', 3,
 ( #54453, #46842, #16881, #62571, #39214, #100092 ),
 .UNSPECIFIED., .F., .F.,
 ( 4, 2, 4 ),
 ( 6.391158118972359742E-06, 0.001387004593080787881, 0.002767618028042603297 ),
 .UNSPECIFIED. ) ;
#87391 = CARTESIAN_POINT ( 'NONE',  ( -4.621320343559254695, 11.49999999999999467, 2.100000000000000089 ) ) ;
#87392 = CARTESIAN_POINT ( 'NONE',  ( 12.26186175617451113, -17.30295086655154080, -1.500000000000002220 ) ) ;
#87393 = ORIENTED_EDGE ( 'NONE', *, *, #73723, .F. ) ;
#87394 = PLANE ( 'NONE',  #65688 ) ;
#87395 = B_SPLINE_CURVE_WITH_KNOTS ( 'NONE', 3,
 ( #6692, #38137, #83313, #22892 ),
 .UNSPECIFIED., .F., .F.,
 ( 4, 4 ),
 ( 0.000000000000000000, 9.999999999998900014E-05 ),
 .UNSPECIFIED. ) ;
#87396 = CARTESIAN_POINT ( 'NONE',  ( -15.04333773895388937, -15.80532200100455498, -1.500000000000002220 ) ) ;
#87397 = CARTESIAN_POINT ( 'NONE',  ( -52.54748251683253102, -24.15620529776627734, 10.23563542870661180 ) ) ;
#87398 = DIRECTION ( 'NONE',  ( 0.000000000000000000, -1.000000000000000000, 0.000000000000000000 ) ) ;
#87399 = DIRECTION ( 'NONE',  ( 0.000000000000000000, 1.000000000000000000, -0.000000000000000000 ) ) ;
#87400 = CARTESIAN_POINT ( 'NONE',  ( 8.176594470695947692, -20.27425322898990601, -1.500000000000002220 ) ) ;
#87401 = DIRECTION ( 'NONE',  ( 0.000000000000000000, 0.000000000000000000, 1.000000000000000000 ) ) ;
#87402 = EDGE_LOOP ( 'NONE', ( #78717, #69046, #16480, #5620 ) ) ;
#87403 = DIRECTION ( 'NONE',  ( 0.000000000000000000, 0.9999999999976377785, 2.173523156925979552E-06 ) ) ;
#87404 = CARTESIAN_POINT ( 'NONE',  ( -85.55305756195892286, -24.15602025860895807, 10.28564288303535967 ) ) ;
#87405 = ORIENTED_EDGE ( 'NONE', *, *, #56463, .T. ) ;
#87406 = B_SPLINE_CURVE_WITH_KNOTS ( 'NONE', 3,
 ( #15416, #16923, #63623, #93037, #32646, #22518, #69724, #69214 ),
 .UNSPECIFIED., .F., .F.,
 ( 4, 2, 2, 4 ),
 ( 6.391158118970574197E-06, 0.002007136338672929621, 0.003007508928949906898, 0.004007881519226884175 ),
 .UNSPECIFIED. ) ;
#87407 = VERTEX_POINT ( 'NONE', #99831 ) ;
#87408 = ORIENTED_EDGE ( 'NONE', *, *, #80306, .T. ) ;
#87409 = FACE_OUTER_BOUND ( 'NONE', #99784, .T. ) ;
#87410 = CARTESIAN_POINT ( 'NONE',  ( -82.58520315302067161, -24.51314013834315375, 0.6176544820404169522 ) ) ;
#87411 = CARTESIAN_POINT ( 'NONE',  ( -19.96038302963917488, -7.207760892512529161, 11.49999999999998934 ) ) ;
#87412 = CARTESIAN_POINT ( 'NONE',  ( 13.57151214508650305, -9.529487854913506695, -1.500000000000000666 ) ) ;
#87413 = CARTESIAN_POINT ( 'NONE',  ( -130.5728709571500588, -24.14929313691198232, 10.49653219292474482 ) ) ;
#87414 = DIRECTION ( 'NONE',  ( 0.000000000000000000, -1.000000000000000000, 0.000000000000000000 ) ) ;
#87415 = CARTESIAN_POINT ( 'NONE',  ( 8.160000000000000142, 0.1579206558577706254, 7.788828319098143105 ) ) ;
#87416 = CARTESIAN_POINT ( 'NONE',  ( 3.148799746435844593, 19.17640706095922098, -1.500000000000002220 ) ) ;
#87417 = EDGE_CURVE ( 'NONE', #47644, #73404, #93808, .T. ) ;
#87418 = CARTESIAN_POINT ( 'NONE',  ( -80.58953762381671027, -23.48786465467241058, 11.44779295918254469 ) ) ;
#87419 = ORIENTED_EDGE ( 'NONE', *, *, #8107, .T. ) ;
#87420 = CARTESIAN_POINT ( 'NONE',  ( 19.19537281719634336, 3.394423509666608663, 11.49999999999999645 ) ) ;
#87421 = CARTESIAN_POINT ( 'NONE',  ( 31.60706529141452137, -4.540774720514427543, 26.12024523944105070 ) ) ;
#87422 = VECTOR ( 'NONE', #38672, 1000.000000000000114 ) ;
#87423 = CARTESIAN_POINT ( 'NONE',  ( 33.69795529655567634, 0.6647747205144264315, 23.11160796525322070 ) ) ;
#87424 = ORIENTED_EDGE ( 'NONE', *, *, #60925, .F. ) ;
#87425 = CARTESIAN_POINT ( 'NONE',  ( 4.527536911777373163, -6.376774720514422512, 21.53954785142818196 ) ) ;
#87426 = FACE_OUTER_BOUND ( 'NONE', #74970, .T. ) ;
#87427 = AXIS2_PLACEMENT_3D ( 'NONE', #83760, #37594, #14241 ) ;
#87428 = CARTESIAN_POINT ( 'NONE',  ( -80.55620429048342146, -23.47596703998600276, 11.44779298504227683 ) ) ;
#87429 = DIRECTION ( 'NONE',  ( 0.000000000000000000, -1.000000000000000000, 0.000000000000000000 ) ) ;
#87430 = CARTESIAN_POINT ( 'NONE',  ( -10.66912846187372210, -16.51573522771486324, -1.500000000000002220 ) ) ;
#87431 = AXIS2_PLACEMENT_3D ( 'NONE', #90115, #27223, #66298 ) ;
#87432 = ORIENTED_EDGE ( 'NONE', *, *, #9737, .T. ) ;
#87433 = CIRCLE ( 'NONE', #56678, 6.000000000000000888 ) ;
#87434 = B_SPLINE_CURVE_WITH_KNOTS ( 'NONE', 3,
 ( #20964, #59054, #90488, #74754 ),
 .UNSPECIFIED., .F., .F.,
 ( 4, 4 ),
 ( 0.000000000000000000, 0.0001000000000000028644 ),
 .UNSPECIFIED. ) ;
#87435 = DIRECTION ( 'NONE',  ( 0.000000000000000000, -0.9999999999976377785, -2.173523156925979975E-06 ) ) ;
#87436 = CARTESIAN_POINT ( 'NONE',  ( -21.10450430117995424, 9.351148110661185342, -1.500000000000002220 ) ) ;
#87437 = EDGE_CURVE ( 'NONE', #79765, #17650, #90248, .T. ) ;
#87438 = AXIS2_PLACEMENT_3D ( 'NONE', #7263, #37723, #68683 ) ;
#87439 = COORDINATED_UNIVERSAL_TIME_OFFSET ( 0, 0, .AHEAD. ) ;
#87440 = CARTESIAN_POINT ( 'NONE',  ( 3.748501943728875574, -5.876774720514425177, 21.47917144995767558 ) ) ;
#87441 = CARTESIAN_POINT ( 'NONE',  ( -60.52287095715006160, -23.47596703998600631, 11.44779298504228926 ) ) ;
#87442 = CARTESIAN_POINT ( 'NONE',  ( -109.8778697195837992, -25.12043765296585818, 2.888617715527074470 ) ) ;
#87443 = CARTESIAN_POINT ( 'NONE',  ( -97.54779265495582763, -24.51419770103157703, 9.386484678747176957 ) ) ;
#87444 = FACE_OUTER_BOUND ( 'NONE', #40754, .T. ) ;
#87445 = APPLICATION_CONTEXT ( 'configuration controlled 3d designs of mechanical parts and assemblies' ) ;
#87446 = CARTESIAN_POINT ( 'NONE',  ( -44.52287095715009713, -23.96127896941631619, -0.6493128931038062435 ) ) ;
#87447 = PLANE ( 'NONE',  #70020 ) ;
#87448 = CARTESIAN_POINT ( 'NONE',  ( -114.6307875202147812, -23.48786465467241769, 11.44779295918253759 ) ) ;
#87449 = CARTESIAN_POINT ( 'NONE',  ( 1.402406813841059030, 19.88454085074057076, -1.500000000000002220 ) ) ;
#87451 = EDGE_CURVE ( 'NONE', #98355, #18610, #32751, .T. ) ;
#87450 = FACE_OUTER_BOUND ( 'NONE', #13368, .T. ) ;
#87452 = CARTESIAN_POINT ( 'NONE',  ( -1.769646468872753120, 19.80360307839763934, -1.500000000000002220 ) ) ;
#87453 = ORIENTED_EDGE ( 'NONE', *, *, #8305, .T. ) ;
#87454 = ADVANCED_FACE ( 'NONE', ( #61312 ), #60312, .F. ) ;
#87455 = CARTESIAN_POINT ( 'NONE',  ( -29.52287095715004739, -24.41831317116936262, 0.6165372783097629039 ) ) ;
#87456 = EDGE_CURVE ( 'NONE', #92122, #51818, #83119, .T. ) ;
#87457 = ADVANCED_FACE ( 'NONE', ( #21713 ), #99345, .F. ) ;
#87458 = CARTESIAN_POINT ( 'NONE',  ( 11.22434917415779054, -4.132774715458839232, -26.87660878605755599 ) ) ;
#87459 = CARTESIAN_POINT ( 'NONE',  ( 19.24418710706453339, 0.000000000000000000, -2.153101996372891236 ) ) ;
#87460 = CARTESIAN_POINT ( 'NONE',  ( -3.686900873480770002, -20.48319827837541141, 11.49999999999999645 ) ) ;
#87461 = CARTESIAN_POINT ( 'NONE',  ( -81.64115287866665938, -23.73766607897671221, -1.055555164236432919 ) ) ;
#87462 = CARTESIAN_POINT ( 'NONE',  ( -75.62287095715004170, -24.99156045073392818, 7.747789690856161648 ) ) ;
#87463 = CARTESIAN_POINT ( 'NONE',  ( 22.20583189720066741, -5.198064566299082756, 11.49999999999999645 ) ) ;
#87464 = ORIENTED_EDGE ( 'NONE', *, *, #54601, .F. ) ;
#87465 = CARTESIAN_POINT ( 'NONE',  ( -56.52287095715006870, -29.50248528299804818, 1.056150453629034924 ) ) ;
#87466 = CARTESIAN_POINT ( 'NONE',  ( 7.480769230769231726, -5.876774720514430506, 20.77403846153845635 ) ) ;
#87467 = ORIENTED_EDGE ( 'NONE', *, *, #59817, .F. ) ;
#87468 = CARTESIAN_POINT ( 'NONE',  ( -18.82339984186270598, 7.397194320553815317, -1.500000000000002220 ) ) ;
#87469 = B_SPLINE_CURVE_WITH_KNOTS ( 'NONE', 3,
 ( #23701, #29321, #21693, #38435 ),
 .UNSPECIFIED., .F., .F.,
 ( 4, 4 ),
 ( 0.000000000000000000, 0.0001000000000000167422 ),
 .UNSPECIFIED. ) ;
#87470 = EDGE_CURVE ( 'NONE', #8126, #4386, #4911, .T. ) ;
#87471 = CARTESIAN_POINT ( 'NONE',  ( 7.480769230769231726, -5.876774720514420736, 20.77403846153845635 ) ) ;
#87472 = CARTESIAN_POINT ( 'NONE',  ( -40.54486904600227604, -25.30535573344747036, 5.077984538006014681 ) ) ;
#87473 = LINE ( 'NONE', #96095, #42792 ) ;
#87474 = ORIENTED_EDGE ( 'NONE', *, *, #20837, .F. ) ;
#87475 = CARTESIAN_POINT ( 'NONE',  ( -30.64427850938831099, -23.56000036390796382, 11.50200000000000067 ) ) ;
#87476 = CARTESIAN_POINT ( 'NONE',  ( -104.5562042904834072, -23.47596703998600631, 11.44779298504227683 ) ) ;
#87477 = CARTESIAN_POINT ( 'NONE',  ( 1.468936567494551593, -19.95401460376903913, -1.500000000000002220 ) ) ;
#87478 = CARTESIAN_POINT ( 'NONE',  ( -123.5190373946633429, -24.65952944569305316, 1.056160979905706343 ) ) ;
#87479 = CARTESIAN_POINT ( 'NONE',  ( -17.07941033872765146, 12.18221932706078370, 11.49999999999999645 ) ) ;
#87480 = CARTESIAN_POINT ( 'NONE',  ( 10.40578984036287302, 5.965225279485572685, -28.04626194901324965 ) ) ;
#87481 = CARTESIAN_POINT ( 'NONE',  ( -79.62287095715005592, -24.64965695001468404, 8.947790433994182280 ) ) ;
#87482 = CARTESIAN_POINT ( 'NONE',  ( -13.14421341422731260, -17.72855101262432242, -1.500000000000002220 ) ) ;
#87483 = VECTOR ( 'NONE', #39661, 1000.000000000000227 ) ;
#87484 = EDGE_CURVE ( 'NONE', #83384, #6469, #98846, .T. ) ;
#87485 = CARTESIAN_POINT ( 'NONE',  ( 8.016553709168819708, 5.226461770140181429, -25.82553693194279276 ) ) ;
#87486 = ORIENTED_EDGE ( 'NONE', *, *, #95, .T. ) ;
#87487 = LINE ( 'NONE', #17472, #47022 ) ;
#87488 = CARTESIAN_POINT ( 'NONE',  ( -49.50910156767503878, -25.27344905013621101, 3.963068828678178335 ) ) ;
#87489 = ADVANCED_FACE ( 'NONE', ( #75505 ), #14612, .F. ) ;
#87490 = DIRECTION ( 'NONE',  ( 0.000000000000000000, 1.000000000000000000, -0.000000000000000000 ) ) ;
#87491 = ORIENTED_EDGE ( 'NONE', *, *, #40213, .T. ) ;
#87492 = CARTESIAN_POINT ( 'NONE',  ( 3.252808283508203058, -6.376774720514402972, 18.30939203766361345 ) ) ;
#87493 = EDGE_LOOP ( 'NONE', ( #67978, #12199, #84360, #97230 ) ) ;
#87494 = AXIS2_PLACEMENT_3D ( 'NONE', #18975, #43820, #96598 ) ;
#87495 = ORIENTED_EDGE ( 'NONE', *, *, #28593, .T. ) ;
#87496 = CARTESIAN_POINT ( 'NONE',  ( -1.877194073982709988, 8.794404527355018431, 9.000000000000000000 ) ) ;
#87497 = PLANE ( 'NONE',  #64859 ) ;
#87498 = DIRECTION ( 'NONE',  ( -0.000000000000000000, 0.000000000000000000, -1.000000000000000000 ) ) ;
#87499 = CARTESIAN_POINT ( 'NONE',  ( 6.429960413904108663, -19.47341730443774921, -1.500000000000002220 ) ) ;
#87500 = ADVANCED_FACE ( 'NONE', ( #5506 ), #29843, .T. ) ;
#87501 = EDGE_LOOP ( 'NONE', ( #64102, #21089, #51453, #44087 ) ) ;
#87502 = CARTESIAN_POINT ( 'NONE',  ( -126.5228709571500616, -24.65952944569305316, 1.056160979905707675 ) ) ;
#87503 = AXIS2_PLACEMENT_3D ( 'NONE', #95518, #33119, #42261 ) ;
#87504 = FACE_OUTER_BOUND ( 'NONE', #27578, .T. ) ;
#87505 = CARTESIAN_POINT ( 'NONE',  ( -64.52287095715006160, -24.64965694238407323, 8.947790433994201820 ) ) ;
#87506 = CARTESIAN_POINT ( 'NONE',  ( 2.183928509170398602, -22.20744181112294413, 11.49999999999998934 ) ) ;
#87507 = EDGE_CURVE ( 'NONE', #32756, #30205, #59355, .T. ) ;
#87508 = CARTESIAN_POINT ( 'NONE',  ( -101.5562042904833788, -24.64965694238575011, 8.947790433994192938 ) ) ;
#87509 = CARTESIAN_POINT ( 'NONE',  ( -2.148731487934370410, -5.876774720514411854, 19.46295461892501422 ) ) ;
#87510 = ORIENTED_EDGE ( 'NONE', *, *, #13909, .T. ) ;
#87511 = EDGE_CURVE ( 'NONE', #80236, #95000, #23022, .T. ) ;
#87512 = DIRECTION ( 'NONE',  ( 1.000000000000000000, 0.000000000000000000, 0.000000000000000000 ) ) ;
#87513 = VECTOR ( 'NONE', #61321, 1000.000000000000114 ) ;
#87514 = CARTESIAN_POINT ( 'NONE',  ( -32.07722060962682775, -29.50248914092071928, 2.831113219569932227 ) ) ;
#87515 = AXIS2_PLACEMENT_3D ( 'NONE', #49802, #11218, #42193 ) ;
#87516 = CARTESIAN_POINT ( 'NONE',  ( 20.84756458399398937, 0.1950554047328266483, 11.49999999999998934 ) ) ;
#87517 = EDGE_LOOP ( 'NONE', ( #15265, #90142, #56322, #66734 ) ) ;
#87518 = B_SPLINE_CURVE_WITH_KNOTS ( 'NONE', 3,
 ( #99125, #76287, #60600, #21995 ),
 .UNSPECIFIED., .F., .F.,
 ( 4, 4 ),
 ( 0.000000000000000000, 9.999999999998897304E-05 ),
 .UNSPECIFIED. ) ;
#87520 = ORIENTED_EDGE ( 'NONE', *, *, #63878, .F. ) ;
#87519 = CARTESIAN_POINT ( 'NONE',  ( -79.52287095715006160, -24.66019654487199375, 8.947790411086122830 ) ) ;
#87521 = ORIENTED_EDGE ( 'NONE', *, *, #95629, .T. ) ;
#87522 = AXIS2_PLACEMENT_3D ( 'NONE', #81925, #90529, #21502 ) ;
#87524 = EDGE_CURVE ( 'NONE', #11386, #23547, #84626, .T. ) ;
#87523 = LINE ( 'NONE', #48966, #21195 ) ;
#87525 = CARTESIAN_POINT ( 'NONE',  ( -19.97109070424261645, 6.737033823242594366, -1.500000000000002220 ) ) ;
#87526 = ORIENTED_EDGE ( 'NONE', *, *, #20476, .F. ) ;
#87527 = CARTESIAN_POINT ( 'NONE',  ( -110.6228709571500559, -24.99132157543166954, 2.256160258750667502 ) ) ;
#87528 = CARTESIAN_POINT ( 'NONE',  ( -7.326923076923074873, -6.376774720514427841, 21.75000000000001066 ) ) ;
#87529 = PLANE ( 'NONE',  #10826 ) ;
#87530 = FACE_OUTER_BOUND ( 'NONE', #57237, .T. ) ;
#87531 = CARTESIAN_POINT ( 'NONE',  ( 2.230654205607476737, -0.1647943925233645579, -7.922169807384186089E-16 ) ) ;
#87532 = CARTESIAN_POINT ( 'NONE',  ( 2.849777056880220982, 21.50153301832798647, -1.500000000000002220 ) ) ;
#87533 = FACE_OUTER_BOUND ( 'NONE', #70512, .T. ) ;
#87535 = ORIENTED_EDGE ( 'NONE', *, *, #54377, .F. ) ;
#87534 = CARTESIAN_POINT ( 'NONE',  ( 21.15429367616652101, -6.912965584596229895, 11.49999999999999645 ) ) ;
#87536 = CARTESIAN_POINT ( 'NONE',  ( -50.82761139903328029, -25.24728739217141538, 5.269904184087572219 ) ) ;
#87537 = DIRECTION ( 'NONE',  ( -3.773278334453079030E-23, 0.9999999999976377785, 2.173523156925979128E-06 ) ) ;
#87538 = ORIENTED_EDGE ( 'NONE', *, *, #70450, .F. ) ;
#87540 = VERTEX_POINT ( 'NONE', #77000 ) ;
#87539 = CARTESIAN_POINT ( 'NONE',  ( -118.6228709571500275, -24.33927499327855415, 9.819080762295808285 ) ) ;
#87541 = ORIENTED_EDGE ( 'NONE', *, *, #38426, .F. ) ;
#87542 = DIRECTION ( 'NONE',  ( -0.000000000000000000, -1.000000000000000000, -0.000000000000000000 ) ) ;
#87543 = CARTESIAN_POINT ( 'NONE',  ( 16.68447708738676383, -11.30049470069299922, 11.49999999999998934 ) ) ;
#87544 = CARTESIAN_POINT ( 'NONE',  ( 33.61456970919601872, -6.376774720514426953, -11.35828564741663627 ) ) ;
#87545 = ORIENTED_EDGE ( 'NONE', *, *, #14157, .T. ) ;
#87546 = CARTESIAN_POINT ( 'NONE',  ( -130.5728709571500588, -24.48854083826206463, 0.3146758927689199958 ) ) ;
#87547 = CARTESIAN_POINT ( 'NONE',  ( 22.28251467978060063, -2.329348454117679879, -1.500000000000002220 ) ) ;
#87548 = ORIENTED_EDGE ( 'NONE', *, *, #83132, .F. ) ;
#87549 = ORIENTED_EDGE ( 'NONE', *, *, #65552, .T. ) ;
#87550 = CARTESIAN_POINT ( 'NONE',  ( -112.6317049575896334, -23.48786465467241769, 11.44779295918253936 ) ) ;
#87551 = CARTESIAN_POINT ( 'NONE',  ( -94.51866276539982437, -23.73791477778911840, 11.05961554403170588 ) ) ;
#87552 = DIRECTION ( 'NONE',  ( -0.7512896232465891000, -0.000000000000000000, -0.6599726524652351767 ) ) ;
#87553 = DIRECTION ( 'NONE',  ( -2.417950247244706201E-16, 0.000000000000000000, 1.000000000000000000 ) ) ;
#87554 = CARTESIAN_POINT ( 'NONE',  ( -30.60163303648719690, -24.57143472585066135, 0.8294870405985536044 ) ) ;
#87555 = CARTESIAN_POINT ( 'NONE',  ( -9.542874777335924819, 17.09510996321218101, -1.500000000000002220 ) ) ;
#87556 = CARTESIAN_POINT ( 'NONE',  ( -46.65379568173771929, -23.73766607897669800, -1.055555164236460008 ) ) ;
#87557 = ORIENTED_EDGE ( 'NONE', *, *, #83422, .T. ) ;
#87558 = CARTESIAN_POINT ( 'NONE',  ( -5.740839400147730309, 20.75665450205591966, 11.49999999999998934 ) ) ;
#87559 = CARTESIAN_POINT ( 'NONE',  ( -128.6234765650372935, -24.65952944569304961, 1.056160979905706787 ) ) ;
#87560 = CARTESIAN_POINT ( 'NONE',  ( -71.14319566529317740, -25.25639514997889989, 6.703707704318174088 ) ) ;
#87561 = DIRECTION ( 'NONE',  ( -1.000000000000000000, -3.773278334444166432E-23, -8.201307841325785021E-29 ) ) ;
#87562 = CIRCLE ( 'NONE', #61643, 0.3000000000000016542 ) ;
#87563 = LINE ( 'NONE', #72849, #94155 ) ;
#87564 = CARTESIAN_POINT ( 'NONE',  ( 15.01570752033863165, -17.30494853738164096, -1.500000000000002220 ) ) ;
#87565 = EDGE_CURVE ( 'NONE', #89859, #79893, #41206, .T. ) ;
#87566 = DATE_AND_TIME ( #38882, #14830 ) ;
#87567 = CARTESIAN_POINT ( 'NONE',  ( -128.5228709571500758, -24.64898659630368627, 1.056161002820834804 ) ) ;
#87568 = PLANE ( 'NONE',  #70096 ) ;
#87569 = CARTESIAN_POINT ( 'NONE',  ( 4.282148337517553749, -19.64591042314588165, 11.49999999999999645 ) ) ;
#87570 = CARTESIAN_POINT ( 'NONE',  ( -110.0261373028301080, -25.28814073874244173, 2.855322185807698254 ) ) ;
#87571 = CARTESIAN_POINT ( 'NONE',  ( -119.5228709571500474, -23.47593901973090524, -1.443836447538996204 ) ) ;
#87572 = EDGE_CURVE ( 'NONE', #77746, #40606, #74032, .T. ) ;
#87573 = CARTESIAN_POINT ( 'NONE',  ( -99.52287095715010423, -24.34917612407053156, 0.1852690917483114930 ) ) ;
#87574 = CARTESIAN_POINT ( 'NONE',  ( -126.5895376238167529, -23.47596703998600631, 11.44779298504227683 ) ) ;
#87575 = CARTESIAN_POINT ( 'NONE',  ( 15.10352928271630724, 3.582999323269832725, -27.29968155418892195 ) ) ;
#87576 = CARTESIAN_POINT ( 'NONE',  ( 19.22361159462649027, -4.937694622890139939, 11.49999999999998934 ) ) ;
#87577 = ADVANCED_FACE ( 'NONE', ( #75008 ), #92729, .T. ) ;
#87578 = DIRECTION ( 'NONE',  ( -1.000000000000000000, 0.000000000000000000, 0.000000000000000000 ) ) ;
#87579 = CARTESIAN_POINT ( 'NONE',  ( -8.025172913017740939, -17.94849717234452768, -1.500000000000002220 ) ) ;
#87580 = ADVANCED_FACE ( 'NONE', ( #47083 ), #69907, .F. ) ;
#87581 = DIRECTION ( 'NONE',  ( 1.000000000000000000, -0.000000000000000000, 2.417950247244706201E-16 ) ) ;
#87582 = EDGE_CURVE ( 'NONE', #90981, #88018, #392, .T. ) ;
#87583 = VECTOR ( 'NONE', #21750, 1000.000000000000114 ) ;
#87584 = CARTESIAN_POINT ( 'NONE',  ( -58.58953762381672448, -23.48786465467241769, 11.44779295918254824 ) ) ;
#87585 = COORDINATED_UNIVERSAL_TIME_OFFSET ( 0, 0, .AHEAD. ) ;
#87587 = EDGE_CURVE ( 'NONE', #60599, #58829, #150, .T. ) ;
#87586 = AXIS2_PLACEMENT_3D ( 'NONE', #44935, #27706, #60166 ) ;
#87588 = CARTESIAN_POINT ( 'NONE',  ( -60.52287095715004028, -24.14406661686764366, 10.28769366194078216 ) ) ;
#87589 = CARTESIAN_POINT ( 'NONE',  ( -39.07220902699673104, -25.29584393180295265, 4.512460029652592297 ) ) ;
#87590 = CARTESIAN_POINT ( 'NONE',  ( 10.54205562766345672, -17.70522803435136083, 11.49999999999999645 ) ) ;
#87591 = CARTESIAN_POINT ( 'NONE',  ( 4.373554412633047228, -5.876774720514421624, 21.19197260575996822 ) ) ;
#87592 = FACE_OUTER_BOUND ( 'NONE', #23574, .T. ) ;
#87593 = AXIS2_PLACEMENT_3D ( 'NONE', #62873, #39512, #93789 ) ;
#87594 = CARTESIAN_POINT ( 'NONE',  ( -21.16596634977960179, 8.012090315382277339, 11.49999999999999645 ) ) ;
#87595 = EDGE_LOOP ( 'NONE', ( #45839, #3055, #95635, #92581, #13515, #41452, #34499, #67538 ) ) ;
#87596 = CARTESIAN_POINT ( 'NONE',  ( -115.6228709571500417, -23.48783264082478794, -1.443836473390058384 ) ) ;
#87597 = CARTESIAN_POINT ( 'NONE',  ( -7.160000000000000142, -6.754662360505033547, 7.925641719537454222 ) ) ;
#87598 = CARTESIAN_POINT ( 'NONE',  ( -56.52287095715009002, -23.48783264082476308, -1.443836473390091690 ) ) ;
#87599 = CARTESIAN_POINT ( 'NONE',  ( -58.52287095715006160, -29.50247984919015209, -1.443849546365056913 ) ) ;
#87600 = ADVANCED_FACE ( 'NONE', ( #17115 ), #91470, .T. ) ;
#87601 = CARTESIAN_POINT ( 'NONE',  ( 23.91005183030481263, 2.682774720514426559, -14.40591128290692069 ) ) ;
#87602 = CARTESIAN_POINT ( 'NONE',  ( -75.52287095715007581, -23.47593901973090169, -1.443836447538996870 ) ) ;
#87603 = ORIENTED_EDGE ( 'NONE', *, *, #74950, .F. ) ;
#87604 = EDGE_CURVE ( 'NONE', #97072, #17304, #22509, .T. ) ;
#87605 = CARTESIAN_POINT ( 'NONE',  ( 8.286623624103266097E-13, -23.05000000000000426, 11.49999999999999645 ) ) ;
#87606 = CARTESIAN_POINT ( 'NONE',  ( -5.953223121155255981, 22.05028593715628560, 11.49999999999998934 ) ) ;
#87607 = FACE_OUTER_BOUND ( 'NONE', #46481, .T. ) ;
#87608 = CARTESIAN_POINT ( 'NONE',  ( -96.63278121929289455, -23.96119346886881019, -0.6495511937832062488 ) ) ;
#87609 = CARTESIAN_POINT ( 'NONE',  ( -63.49529785725831488, -24.51419770103156992, 9.386484678747175181 ) ) ;
#87610 = CARTESIAN_POINT ( 'NONE',  ( -20.52357230491503159, 9.176553703681571861, 11.49999999999999645 ) ) ;
#87611 = EDGE_LOOP ( 'NONE', ( #70702, #49614, #13480, #18440 ) ) ;
#87612 = DIRECTION ( 'NONE',  ( -3.773278334453079030E-23, 0.9999999999976377785, 2.173523156925979128E-06 ) ) ;
#87613 = CARTESIAN_POINT ( 'NONE',  ( -21.26704322615652032, -5.532269525099344776, 11.49999999999998934 ) ) ;
#87614 = B_SPLINE_CURVE_WITH_KNOTS ( 'NONE', 3,
 ( #84136, #16127, #4656, #58943 ),
 .UNSPECIFIED., .F., .F.,
 ( 4, 4 ),
 ( 0.9511792137939691916, 0.9601856450660847253 ),
 .UNSPECIFIED. ) ;
#87615 = CARTESIAN_POINT ( 'NONE',  ( -54.62287095715005592, -24.65952944569304606, 1.056160979905694131 ) ) ;
#87616 = CARTESIAN_POINT ( 'NONE',  ( -34.51265709502276735, -23.73791477778911485, 11.05961554403171299 ) ) ;
#87617 = DIRECTION ( 'NONE',  ( 1.000000000000000000, 0.000000000000000000, 0.000000000000000000 ) ) ;
#87618 = ORIENTED_EDGE ( 'NONE', *, *, #17223, .F. ) ;
#87619 = FACE_OUTER_BOUND ( 'NONE', #85343, .T. ) ;
#87620 = FACE_OUTER_BOUND ( 'NONE', #70403, .T. ) ;
#87621 = ORIENTED_EDGE ( 'NONE', *, *, #94936, .F. ) ;
#87622 = CARTESIAN_POINT ( 'NONE',  ( -54.57824257350981156, -24.66019654487199375, 8.947790411086119278 ) ) ;
#87623 = CARTESIAN_POINT ( 'NONE',  ( 3.385237411341575964, -20.22741857368478335, 11.49999999999998934 ) ) ;
#87624 = ORIENTED_EDGE ( 'NONE', *, *, #85492, .T. ) ;
#87625 = ORIENTED_EDGE ( 'NONE', *, *, #25739, .F. ) ;
#87626 = ORIENTED_EDGE ( 'NONE', *, *, #83715, .T. ) ;
#87627 = EDGE_LOOP ( 'NONE', ( #31052, #28335 ) ) ;
#87628 = CARTESIAN_POINT ( 'NONE',  ( 13.57151214508650305, -9.529487854913506695, 0.000000000000000000 ) ) ;
#87629 = CARTESIAN_POINT ( 'NONE',  ( 18.33865528945960577, 14.04639130150205872, -1.500000000000002220 ) ) ;
#87630 = CARTESIAN_POINT ( 'NONE',  ( -104.5103158840345117, -24.66019654487200441, 8.947790411086108620 ) ) ;
#87631 = CARTESIAN_POINT ( 'NONE',  ( -5.548086588741434788, -19.59138962566686004, -1.500000000000002220 ) ) ;
#87632 = VERTEX_POINT ( 'NONE', #89632 ) ;
#87633 = LINE ( 'NONE', #39951, #12059 ) ;
#87634 = FACE_OUTER_BOUND ( 'NONE', #18615, .T. ) ;
#87635 = EDGE_CURVE ( 'NONE', #56601, #31048, #34353, .T. ) ;
#87636 = CARTESIAN_POINT ( 'NONE',  ( -112.9228709571500531, -23.47593901973090524, -1.443836447538996648 ) ) ;
#87637 = CARTESIAN_POINT ( 'NONE',  ( -63.52287095715010423, -23.95044443724991723, 10.65354141964649948 ) ) ;
#87638 = VERTEX_POINT ( 'NONE', #27240 ) ;
#87639 = CARTESIAN_POINT ( 'NONE',  ( -29.24636659181000198, -24.76881433503877616, 4.940287988257682450 ) ) ;
#87640 = DIRECTION ( 'NONE',  ( 1.000000000000000000, 0.000000000000000000, 0.000000000000000000 ) ) ;
#87641 = VERTEX_POINT ( 'NONE', #11502 ) ;
#87642 = CARTESIAN_POINT ( 'NONE',  ( -3.546427018491999483, -20.45703643143680850, 11.49999999999998934 ) ) ;
#87644 = EDGE_CURVE ( 'NONE', #62185, #92377, #41464, .T. ) ;
#87643 = CIRCLE ( 'NONE', #3349, 3.060000000000000053 ) ;
#87645 = ORIENTED_EDGE ( 'NONE', *, *, #17753, .F. ) ;
#87647 = EDGE_LOOP ( 'NONE', ( #10460, #76345, #68515, #91352, #51771, #78205, #85781, #41852 ) ) ;
#87646 = CARTESIAN_POINT ( 'NONE',  ( -125.5192795453270378, -25.00158670708911046, 2.256160236439218369 ) ) ;
#87648 = DIRECTION ( 'NONE',  ( -0.000000000000000000, -1.000000000000000000, 0.000000000000000000 ) ) ;
#87650 = CARTESIAN_POINT ( 'NONE',  ( -122.6228709571500417, -24.66019654487199730, 8.947790411086121054 ) ) ;
#87649 = B_SPLINE_CURVE_WITH_KNOTS ( 'NONE', 3,
 ( #19262, #26886, #4560, #50233, #66482, #35508 ),
 .UNSPECIFIED., .F., .F.,
 ( 4, 2, 4 ),
 ( 1.570755371633856203E-05, 0.001396183895866085368, 0.002776660238015832109 ),
 .UNSPECIFIED. ) ;
#87651 = ORIENTED_EDGE ( 'NONE', *, *, #55997, .T. ) ;
#87652 = ORIENTED_EDGE ( 'NONE', *, *, #12814, .T. ) ;
#87653 = DIRECTION ( 'NONE',  ( -0.000000000000000000, 1.000000000000000000, -0.000000000000000000 ) ) ;
#87654 = CARTESIAN_POINT ( 'NONE',  ( -98.52287095715006160, -23.48786465467241769, 11.44779295918254114 ) ) ;
#87655 = CARTESIAN_POINT ( 'NONE',  ( -30.93930388503498818, -23.47593901973090169, -1.443836447538998424 ) ) ;
#87657 = ORIENTED_EDGE ( 'NONE', *, *, #26200, .F. ) ;
#87656 = CARTESIAN_POINT ( 'NONE',  ( 9.306852550357104903, -20.00191182576189064, 11.49999999999999645 ) ) ;
#87658 = CARTESIAN_POINT ( 'NONE',  ( -47.62287095715004881, -23.73934037231756733, 11.05740245334329153 ) ) ;
#87659 = CARTESIAN_POINT ( 'NONE',  ( 18.14931799402153345, 13.46472642042223633, -1.500000000000002220 ) ) ;
#87661 = VERTEX_POINT ( 'NONE', #65819 ) ;
#87660 = CARTESIAN_POINT ( 'NONE',  ( -79.11611000704996854, -25.13069340115296058, 2.947789388436138580 ) ) ;
#87662 = VECTOR ( 'NONE', #35877, 1000.000000000000000 ) ;
#87663 = ORIENTED_EDGE ( 'NONE', *, *, #94435, .F. ) ;
#87664 = CIRCLE ( 'NONE', #56897, 0.8160000000000007248 ) ;
#87665 = CARTESIAN_POINT ( 'NONE',  ( -84.62287095715005592, -29.50248528299804818, 1.056150453629038477 ) ) ;
#87666 = CARTESIAN_POINT ( 'NONE',  ( -57.54249901568284997, -24.35071581493543036, 9.817618358456028815 ) ) ;
#87667 = ORIENTED_EDGE ( 'NONE', *, *, #60770, .F. ) ;
#87668 = CARTESIAN_POINT ( 'NONE',  ( -0.1268723920767304558, 21.18662008908366445, -1.500000000000002220 ) ) ;
#87669 = CARTESIAN_POINT ( 'NONE',  ( -34.62287095715005592, -23.96177878511307568, 10.65340807706330573 ) ) ;
#87670 = CARTESIAN_POINT ( 'NONE',  ( 30.61643171255909479, -3.477635932356431869, 27.37433006808820579 ) ) ;
#87671 = CARTESIAN_POINT ( 'NONE',  ( -32.52287095715006160, -23.47596703998600631, 11.44779298504229459 ) ) ;
#87672 = CARTESIAN_POINT ( 'NONE',  ( -82.52287095715006160, -29.50250243563736774, 8.947779886222141599 ) ) ;
#87673 = CARTESIAN_POINT ( 'NONE',  ( -4.330935931041660858, -21.79039167146679290, -1.500000000000002220 ) ) ;
#87674 = CARTESIAN_POINT ( 'NONE',  ( -114.5149094425525504, -24.65952944569305316, 1.056160979905706121 ) ) ;
#87675 = ORIENTED_EDGE ( 'NONE', *, *, #57419, .T. ) ;
#87676 = DIRECTION ( 'NONE',  ( 0.000000000000000000, -0.000000000000000000, 1.000000000000000000 ) ) ;
#87677 = LINE ( 'NONE', #56746, #54104 ) ;
#87678 = CARTESIAN_POINT ( 'NONE',  ( -19.24332624019526961, -2.196797614219411443, 11.49999999999999645 ) ) ;
#87679 = PLANE ( 'NONE',  #59293 ) ;
#87680 = CARTESIAN_POINT ( 'NONE',  ( -44.92287095715005307, -23.47596703998600631, 11.44779298504227683 ) ) ;
#87681 = B_SPLINE_CURVE_WITH_KNOTS ( 'NONE', 3,
 ( #83536, #22127, #83032, #59218, #51107, #5919 ),
 .UNSPECIFIED., .F., .F.,
 ( 4, 2, 4 ),
 ( 6.391158118967745954E-06, 0.001387004593080787230, 0.002767618028042606766 ),
 .UNSPECIFIED. ) ;
#87682 = CARTESIAN_POINT ( 'NONE',  ( 12.63578256557813795, 14.83599306707809085, 11.49999999999998934 ) ) ;
#87683 = CARTESIAN_POINT ( 'NONE',  ( 17.72605931280000391, -11.99821887194124770, -1.500000000000002220 ) ) ;
#87684 = DIRECTION ( 'NONE',  ( 1.000000000000000000, 3.773278334444166432E-23, 8.201307841325785021E-29 ) ) ;
#87685 = CARTESIAN_POINT ( 'NONE',  ( -60.66488840562722373, -23.48786465467241058, 11.44779295918254824 ) ) ;
#87686 = DIRECTION ( 'NONE',  ( -1.226388327005079762E-16, -0.000000000000000000, 1.000000000000000000 ) ) ;
#87687 = CARTESIAN_POINT ( 'NONE',  ( -120.5895376238167245, -24.99156044556202971, 7.747789690856173195 ) ) ;
#87688 = CARTESIAN_POINT ( 'NONE',  ( 19.62911079104473444, -11.51699945595908758, -1.500000000000002220 ) ) ;
#87689 = ADVANCED_FACE ( 'NONE', ( #58195 ), #67168, .T. ) ;
#87690 = DIRECTION ( 'NONE',  ( 1.000000000000000000, 0.000000000000000000, 0.000000000000000000 ) ) ;
#87691 = CARTESIAN_POINT ( 'NONE',  ( -102.5574996872169891, -23.73766607897671577, -1.055555164236430254 ) ) ;
#87692 = DIRECTION ( 'NONE',  ( -3.773278334453080206E-23, 0.9999999999976377785, 2.173523156925979975E-06 ) ) ;
#87693 = CARTESIAN_POINT ( 'NONE',  ( -17.57349146297605103, 9.389787994052484876, 11.49999999999999645 ) ) ;
#87694 = CARTESIAN_POINT ( 'NONE',  ( -69.52287095715007581, -24.51283580621366198, 0.6167428607019654896 ) ) ;
#87695 = ADVANCED_FACE ( 'NONE', ( #18122 ), #49088, .F. ) ;
#87696 = CARTESIAN_POINT ( 'NONE',  ( -98.89303308397303738, -29.50249626970221328, 6.110940943921145951 ) ) ;
#87697 = DIRECTION ( 'NONE',  ( 7.960204194457801640E-17, 1.000000000000000000, -0.000000000000000000 ) ) ;
#87698 = ORIENTED_EDGE ( 'NONE', *, *, #85531, .T. ) ;
#87699 = DIRECTION ( 'NONE',  ( -0.000000000000000000, -0.000000000000000000, -1.000000000000000000 ) ) ;
#87700 = DIRECTION ( 'NONE',  ( -0.000000000000000000, 0.000000000000000000, -1.000000000000000000 ) ) ;
#87701 = EDGE_CURVE ( 'NONE', #48999, #78774, #60692, .T. ) ;
#87702 = CARTESIAN_POINT ( 'NONE',  ( -15.83346750871019992, -14.79491179806518630, -1.500000000000002220 ) ) ;
#87703 = PLANE ( 'NONE',  #25296 ) ;
#87704 = CARTESIAN_POINT ( 'NONE',  ( 15.68791110202092476, 11.56419973807686219, -1.500000000000002220 ) ) ;
#87705 = ADVANCED_FACE ( 'NONE', ( #37351 ), #59694, .T. ) ;
#87706 = CARTESIAN_POINT ( 'NONE',  ( -55.52200627751408746, -23.48786465467241413, 11.44779295918254647 ) ) ;
#87707 = VERTEX_POINT ( 'NONE', #5886 ) ;
#87708 = DIRECTION ( 'NONE',  ( 1.000000000000000000, 3.773278334444167608E-23, 8.201307833595939069E-29 ) ) ;
#87709 = CARTESIAN_POINT ( 'NONE',  ( -9.871001836803966256, -17.81128643866572148, 11.49999999999999645 ) ) ;
#87710 = CARTESIAN_POINT ( 'NONE',  ( -42.62287095715004881, -29.50248528299804818, 1.056150453629031594 ) ) ;
#87711 = EDGE_CURVE ( 'NONE', #20125, #13115, #95771, .T. ) ;
#87712 = CIRCLE ( 'NONE', #98983, 21.89999999999999858 ) ;
#87713 = B_SPLINE_CURVE_WITH_KNOTS ( 'NONE', 3,
 ( #35872, #75914, #58709, #97764, #83026, #60223, #73936, #91145, #36870, #21623, #6419, #68319, #66841, #59214, #4436, #35382 ),
 .UNSPECIFIED., .F., .F.,
 ( 4, 2, 2, 2, 2, 2, 2, 4 ),
 ( -2.611475609838436325E-05, 0.001181507984664241897, 0.001785319355045555511, 0.002389130725426869776, 0.002992942095808183173, 0.003596753466189497005, 0.004200564836570811270, 0.004804376206952124667 ),
 .UNSPECIFIED. ) ;
#87714 = DIRECTION ( 'NONE',  ( -0.000000000000000000, 1.000000000000000000, -0.000000000000000000 ) ) ;
#87715 = B_SPLINE_CURVE_WITH_KNOTS ( 'NONE', 3,
 ( #17733, #80128, #25339, #63429 ),
 .UNSPECIFIED., .F., .F.,
 ( 4, 4 ),
 ( 0.000000000000000000, 9.999999999998897304E-05 ),
 .UNSPECIFIED. ) ;
#87716 = ORIENTED_EDGE ( 'NONE', *, *, #79350, .T. ) ;
#87717 = CARTESIAN_POINT ( 'NONE',  ( -72.52287095715003318, -23.73907113216989373, -1.053371485793251905 ) ) ;
#87718 = CARTESIAN_POINT ( 'NONE',  ( -122.6228709571500417, -29.50250786944525672, 11.44777988621622811 ) ) ;
#87719 = CARTESIAN_POINT ( 'NONE',  ( -39.10567952407142656, -25.31628543545969379, 4.652296572693673582 ) ) ;
#87720 = CARTESIAN_POINT ( 'NONE',  ( -41.32836283488544638, -6.376774720514426953, 39.26872235229541985 ) ) ;
#87721 = CARTESIAN_POINT ( 'NONE',  ( -126.6228709571500559, -29.50250243563736774, 8.947779886222132717 ) ) ;
#87722 = B_SPLINE_CURVE_WITH_KNOTS ( 'NONE', 3,
 ( #6470, #76459, #44536, #37917 ),
 .UNSPECIFIED., .F., .F.,
 ( 4, 4 ),
 ( 0.000000000000000000, 2.030847249360049860E-05 ),
 .UNSPECIFIED. ) ;
#87723 = CARTESIAN_POINT ( 'NONE',  ( -55.92287095715006018, -23.47593901973090169, -1.443836447538997758 ) ) ;
#87724 = ORIENTED_EDGE ( 'NONE', *, *, #45154, .F. ) ;
#87725 = CARTESIAN_POINT ( 'NONE',  ( -66.55385742457673359, -23.96169478059713143, 10.65365249895718058 ) ) ;
#87726 = AXIS2_PLACEMENT_3D ( 'NONE', #49272, #95422, #88316 ) ;
#87727 = CARTESIAN_POINT ( 'NONE',  ( 12.10309942457327992, -19.51426552955538085, 11.49999999999999645 ) ) ;
#87728 = CARTESIAN_POINT ( 'NONE',  ( 21.73672277138745201, -6.736064506363727666, 11.49999999999998934 ) ) ;
#87729 = FACE_OUTER_BOUND ( 'NONE', #85966, .T. ) ;
#87730 = CARTESIAN_POINT ( 'NONE',  ( -74.62287095715005592, -29.50250786944525672, 11.44777988621623699 ) ) ;
#87731 = CARTESIAN_POINT ( 'NONE',  ( -90.51647974171660849, -23.85016227208580730, -0.8807180028928305315 ) ) ;
#87732 = CARTESIAN_POINT ( 'NONE',  ( -29.49875734969026198, 5.965225279485572685, 7.870022800118625206 ) ) ;
#87733 = DIRECTION ( 'NONE',  ( -0.7071067811865475727, 0.000000000000000000, 0.7071067811865475727 ) ) ;
#87734 = CARTESIAN_POINT ( 'NONE',  ( -13.92312151449838531, -16.86485062357919773, -1.500000000000002220 ) ) ;
#87735 = PLANE ( 'NONE',  #18636 ) ;
#87736 = CARTESIAN_POINT ( 'NONE',  ( -115.6228709571500275, -24.52232992886362695, 0.6492154411906169154 ) ) ;
#87737 = FACE_OUTER_BOUND ( 'NONE', #19509, .T. ) ;
#87738 = DIRECTION ( 'NONE',  ( -0.000000000000000000, -1.000000000000000000, -0.000000000000000000 ) ) ;
#87739 = VERTEX_POINT ( 'NONE', #83000 ) ;
#87740 = CARTESIAN_POINT ( 'NONE',  ( -12.12210191164509965, 16.44476101713275185, -1.500000000000002220 ) ) ;
#87741 = ORIENTED_EDGE ( 'NONE', *, *, #37414, .F. ) ;
#87742 = EDGE_LOOP ( 'NONE', ( #12006, #46823, #81419, #79649 ) ) ;
#87743 = B_SPLINE_CURVE_WITH_KNOTS ( 'NONE', 3,
 ( #71773, #72277, #80379, #64685 ),
 .UNSPECIFIED., .F., .F.,
 ( 4, 4 ),
 ( 6.938893903907227607E-18, 9.999999999999593903E-05 ),
 .UNSPECIFIED. ) ;
#87744 = CARTESIAN_POINT ( 'NONE',  ( 22.64363655503811046, -4.068770074275382953, -1.500000000000002220 ) ) ;
#87745 = CARTESIAN_POINT ( 'NONE',  ( 14.87948092214613283, -4.970807589639874458, -27.40745209048265352 ) ) ;
#87746 = EDGE_LOOP ( 'NONE', ( #24999, #62196, #93852, #75946 ) ) ;
#87747 = CARTESIAN_POINT ( 'NONE',  ( -114.5228709571500616, -23.48786465467241769, 11.44779295918253936 ) ) ;
#87748 = DIRECTION ( 'NONE',  ( 0.000000000000000000, 0.000000000000000000, -1.000000000000000000 ) ) ;
#87749 = B_SPLINE_CURVE_WITH_KNOTS ( 'NONE', 3,
 ( #44512, #53133, #100258, #6939, #7431, #90678 ),
 .UNSPECIFIED., .F., .F.,
 ( 4, 2, 4 ),
 ( 6.384118694664676754E-06, 0.001386860460836404803, 0.002767336802978144928 ),
 .UNSPECIFIED. ) ;
#87750 = CARTESIAN_POINT ( 'NONE',  ( 24.50000000000000000, 0.000000000000000000, 1.103411337323757735 ) ) ;
#87751 = CARTESIAN_POINT ( 'NONE',  ( -53.57809142228946087, -24.66019654487199375, 8.947790411086122830 ) ) ;
#87753 = ORIENTED_EDGE ( 'NONE', *, *, #19314, .T. ) ;
#87752 = CARTESIAN_POINT ( 'NONE',  ( 18.99370601119529312, 9.851043883551550806, 11.49999999999999645 ) ) ;
#87754 = ORIENTED_EDGE ( 'NONE', *, *, #36844, .F. ) ;
#87755 = CARTESIAN_POINT ( 'NONE',  ( -4.073883676365832152, 21.86232641878667593, -1.500000000000002220 ) ) ;
#87756 = CARTESIAN_POINT ( 'NONE',  ( -20.26430336558559020, 4.098603726722801710, -1.500000000000002220 ) ) ;
#87757 = EDGE_CURVE ( 'NONE', #17644, #65087, #82464, .T. ) ;
#87758 = ORIENTED_EDGE ( 'NONE', *, *, #25121, .T. ) ;
#87759 = CARTESIAN_POINT ( 'NONE',  ( -6.775140224358976226, -6.376774720514408301, 19.14743589743590846 ) ) ;
#87760 = AXIS2_PLACEMENT_3D ( 'NONE', #66722, #90030, #98625 ) ;
#87761 = EDGE_CURVE ( 'NONE', #39929, #6907, #84005, .T. ) ;
#87762 = CARTESIAN_POINT ( 'NONE',  ( 2.949406532984364393, -5.876774720514410966, 19.42899254576129664 ) ) ;
#87763 = ORIENTED_EDGE ( 'NONE', *, *, #14792, .T. ) ;
#87764 = CARTESIAN_POINT ( 'NONE',  ( -55.52287095715006870, -23.47596703998600631, 11.44779298504228926 ) ) ;
#87765 = ORIENTED_EDGE ( 'NONE', *, *, #21830, .F. ) ;
#87766 = CARTESIAN_POINT ( 'NONE',  ( 8.205893897551582938, -3.316774720514426456, -27.11136772256261196 ) ) ;
#87767 = CARTESIAN_POINT ( 'NONE',  ( -70.44747929723452273, -25.12380530056864103, 7.096986476995511772 ) ) ;
#87768 = CARTESIAN_POINT ( 'NONE',  ( 10.02768300834196502, -18.34552750054021786, -1.500000000000002220 ) ) ;
#87769 = CARTESIAN_POINT ( 'NONE',  ( -6.606886629844116676, -20.84447163495035937, 11.49999999999999645 ) ) ;
#87770 = CARTESIAN_POINT ( 'NONE',  ( -26.33488822642538452, -24.89279768858262187, 6.524121853396118276 ) ) ;
#87771 = PLANE ( 'NONE',  #79108 ) ;
#87772 = CARTESIAN_POINT ( 'NONE',  ( 9.993301969596378953, 20.15287186522775542, -1.500000000000002220 ) ) ;
#87773 = CARTESIAN_POINT ( 'NONE',  ( 16.15719879640481338, -13.26386290209467944, 11.49999999999998934 ) ) ;
#87774 = CARTESIAN_POINT ( 'NONE',  ( -26.12923826827997686, -24.88148856164281852, 5.595194550550813162 ) ) ;
#87775 = CARTESIAN_POINT ( 'NONE',  ( -53.55620429048340725, -24.64898659630527789, 1.056161002820820594 ) ) ;
#87776 = DIRECTION ( 'NONE',  ( 0.000000000000000000, -0.000000000000000000, -1.000000000000000000 ) ) ;
#87777 = ORIENTED_EDGE ( 'NONE', *, *, #30994, .F. ) ;
#87778 = ORIENTED_EDGE ( 'NONE', *, *, #64121, .T. ) ;
#87779 = EDGE_LOOP ( 'NONE', ( #65883, #54700, #49654, #36059 ) ) ;
#87780 = VECTOR ( 'NONE', #93801, 1000.000000000000114 ) ;
#87781 = DIRECTION ( 'NONE',  ( 0.000000000000000000, -1.000000000000000000, 0.000000000000000000 ) ) ;
#87782 = EDGE_LOOP ( 'NONE', ( #21279, #99086, #46754, #7125 ) ) ;
#87783 = CARTESIAN_POINT ( 'NONE',  ( -20.78045986758521835, -5.208592277829342088, -1.500000000000002220 ) ) ;
#87784 = B_SPLINE_CURVE_WITH_KNOTS ( 'NONE', 3,
 ( #95431, #3103, #34038, #65014 ),
 .UNSPECIFIED., .F., .F.,
 ( 4, 4 ),
 ( 0.000000000000000000, 9.999999999998897304E-05 ),
 .UNSPECIFIED. ) ;
#87785 = CARTESIAN_POINT ( 'NONE',  ( 3.152853332073482839, 22.16862046936333286, 11.49999999999999645 ) ) ;
#87786 = ORIENTED_EDGE ( 'NONE', *, *, #44159, .T. ) ;
#87787 = DIRECTION ( 'NONE',  ( 0.000000000000000000, 1.000000000000000000, -0.000000000000000000 ) ) ;
#87788 = CARTESIAN_POINT ( 'NONE',  ( 1.225302832070333636, 21.05158420706169764, 11.49999999999998934 ) ) ;
#87789 = CARTESIAN_POINT ( 'NONE',  ( -30.60817598444602794, -24.49002127936269702, 9.440108529385042857 ) ) ;
#87790 = CARTESIAN_POINT ( 'NONE',  ( 17.47191945374660094, 9.613082372698542599, -1.500000000000002220 ) ) ;
#87791 = CARTESIAN_POINT ( 'NONE',  ( 7.160000000000000142, 1.682056942681651179, 5.192823660268256702 ) ) ;
#87792 = CARTESIAN_POINT ( 'NONE',  ( -46.62287095715004881, -29.50250243563736774, 8.947779886222146928 ) ) ;
#87793 = CARTESIAN_POINT ( 'NONE',  ( -21.92701646642465008, -2.088449908657787457, -1.500000000000002220 ) ) ;
#87794 = ORIENTED_EDGE ( 'NONE', *, *, #68567, .T. ) ;
#87795 = CARTESIAN_POINT ( 'NONE',  ( -116.5892976607136262, -24.34968618360935366, 0.1864209137779019310 ) ) ;
#87796 = LINE ( 'NONE', #58357, #17322 ) ;
#87797 = CARTESIAN_POINT ( 'NONE',  ( -41.36802863981588274, -25.31624677975437976, 5.250400717901936076 ) ) ;
#87798 = CARTESIAN_POINT ( 'NONE',  ( -29.83743700494218842, -25.25831489976056687, 4.936952632524851836 ) ) ;
#87799 = AXIS2_PLACEMENT_3D ( 'NONE', #75085, #60393, #21785 ) ;
#87800 = FACE_OUTER_BOUND ( 'NONE', #42736, .T. ) ;
#87801 = PRODUCT_DEFINITION_FORMATION_WITH_SPECIFIED_SOURCE ( 'ANY', '', #90652, .NOT_KNOWN. ) ;
#87802 = CARTESIAN_POINT ( 'NONE',  ( 8.376690734369038438, 11.49999999999999645, 2.100000000000000089 ) ) ;
#87803 = CARTESIAN_POINT ( 'NONE',  ( -18.01091527469349529, -11.40912366963296698, 11.49999999999998934 ) ) ;
#87804 = CARTESIAN_POINT ( 'NONE',  ( -70.74026866089610621, -25.31511106678998502, 4.894904372220056921 ) ) ;
#87805 = CARTESIAN_POINT ( 'NONE',  ( 2.899999999999999467, 31.80000000000000071, 0.000000000000000000 ) ) ;
#87806 = FACE_OUTER_BOUND ( 'NONE', #83730, .T. ) ;
#87807 = CARTESIAN_POINT ( 'NONE',  ( 4.712727796232543120, 5.356774720514425603, -25.55789472434992859 ) ) ;
#87808 = CARTESIAN_POINT ( 'NONE',  ( 21.71239400539012721, -6.292901409244172406, -1.500000000000002220 ) ) ;
#87809 = FACE_OUTER_BOUND ( 'NONE', #73635, .T. ) ;
#87810 = ORIENTED_EDGE ( 'NONE', *, *, #84459, .T. ) ;
#87811 = CARTESIAN_POINT ( 'NONE',  ( -50.92779201898847674, -25.31191645034120441, 5.304553393514395587 ) ) ;
#87812 = CARTESIAN_POINT ( 'NONE',  ( -120.5562042904833930, -23.47596703998600631, 11.44779298504227683 ) ) ;
#87813 = CARTESIAN_POINT ( 'NONE',  ( 17.05426814964238957, 9.943002105365778220, 11.49999999999999645 ) ) ;
#87814 = PLANE ( 'NONE',  #35869 ) ;
#87815 = ADVANCED_FACE ( 'NONE', ( #99222 ), #53077, .F. ) ;
#87816 = CARTESIAN_POINT ( 'NONE',  ( 19.24418710706453339, -0.5000000000000000000, -2.153101996372891236 ) ) ;
#87817 = ORIENTED_EDGE ( 'NONE', *, *, #45547, .F. ) ;
#87818 = DIRECTION ( 'NONE',  ( 0.000000000000000000, 0.000000000000000000, 1.000000000000000000 ) ) ;
#87819 = CARTESIAN_POINT ( 'NONE',  ( -127.4728709594060092, -25.40676174399604648, 8.000950335807015534 ) ) ;
#87820 = ADVANCED_FACE ( 'NONE', ( #5392 ), #44464, .F. ) ;
#87821 = CARTESIAN_POINT ( 'NONE',  ( -124.5548821316224064, -24.35071581493544457, 9.817618358456016381 ) ) ;
#87822 = CARTESIAN_POINT ( 'NONE',  ( -76.55620429048342146, -24.64898659630528854, 1.056161002820828587 ) ) ;
#87823 = PLANE ( 'NONE',  #70646 ) ;
#87824 = EDGE_CURVE ( 'NONE', #8909, #35157, #18202, .T. ) ;
#87825 = PLANE ( 'NONE',  #51296 ) ;
#87826 = CARTESIAN_POINT ( 'NONE',  ( 2.545096341412688812, 19.61957628810408849, 11.49999999999998934 ) ) ;
#87827 = VERTEX_POINT ( 'NONE', #68292 ) ;
#87828 = EDGE_CURVE ( 'NONE', #14476, #62563, #59189, .T. ) ;
#87829 = B_SPLINE_CURVE_WITH_KNOTS ( 'NONE', 3,
 ( #35196, #19454, #65666, #27585, #19952, #20447, #81862, #49433, #80366, #26585, #27081, #88485, #66168, #11355, #58047, #50420 ),
 .UNSPECIFIED., .F., .F.,
 ( 4, 2, 2, 2, 2, 2, 2, 4 ),
 ( 0.000000000000000000, 0.0002052712941191513771, 0.0004105425882383027542, 0.0008210851764766055084, 0.001026356470595756777, 0.001231627764714908263, 0.001436899058834059748, 0.001642170352953211017 ),
 .UNSPECIFIED. ) ;
#87830 = CARTESIAN_POINT ( 'NONE',  ( 2.532258636284850706, -20.04889675553949147, 11.49999999999999645 ) ) ;
#87831 = CARTESIAN_POINT ( 'NONE',  ( 12.98941176893815275, 6.376774720517114581, -28.15829778590956067 ) ) ;
#87832 = ADVANCED_FACE ( 'NONE', ( #61197 ), #14490, .T. ) ;
#87833 = AXIS2_PLACEMENT_3D ( 'NONE', #67332, #28260, #90162 ) ;
#87834 = VERTEX_POINT ( 'NONE', #45467 ) ;
#87835 = DIRECTION ( 'NONE',  ( 0.9951627101165076983, 0.000000000000000000, 0.09824042138329622254 ) ) ;
#87836 = CARTESIAN_POINT ( 'NONE',  ( -24.90875734969025501, -3.316774720514426456, 29.49402280011862487 ) ) ;
#87837 = CARTESIAN_POINT ( 'NONE',  ( -88.88918693012686845, -25.26680044519436663, 6.101892079195562424 ) ) ;
#87838 = LINE ( 'NONE', #96443, #62930 ) ;
#87839 = CARTESIAN_POINT ( 'NONE',  ( -62.55620429048337883, -23.48786465467241413, 11.44779295918254824 ) ) ;
#87840 = CARTESIAN_POINT ( 'NONE',  ( -86.62287095715005592, -24.66019654487199375, 8.947790411086124607 ) ) ;
#87841 = CARTESIAN_POINT ( 'NONE',  ( 12.85705330080557829, 15.37097598829428513, 11.49999999999998934 ) ) ;
#87842 = EDGE_CURVE ( 'NONE', #23691, #74261, #92116, .T. ) ;
#87843 = CARTESIAN_POINT ( 'NONE',  ( -67.58953762381672448, -23.48783264082478794, -1.443836473390067265 ) ) ;
#87844 = EDGE_LOOP ( 'NONE', ( #34117, #10708, #44238, #40840 ) ) ;
#87845 = CARTESIAN_POINT ( 'NONE',  ( -73.62287095715007013, -23.47596703998600276, 11.44779298504227860 ) ) ;
#87846 = CARTESIAN_POINT ( 'NONE',  ( -33.62287095715007013, -24.34917612406836795, 0.1852690917426547956 ) ) ;
#87847 = DIRECTION ( 'NONE',  ( -0.000000000000000000, 1.000000000000000000, -0.000000000000000000 ) ) ;
#87848 = AXIS2_PLACEMENT_3D ( 'NONE', #88339, #10210, #18813 ) ;
#87849 = FACE_OUTER_BOUND ( 'NONE', #21594, .T. ) ;
#87850 = CARTESIAN_POINT ( 'NONE',  ( -73.63478338152101799, -24.15543982623907127, -0.2315651400026654816 ) ) ;
#87851 = CARTESIAN_POINT ( 'NONE',  ( -45.58953762381671737, -23.47596703998600276, 11.44779298504227505 ) ) ;
#87852 = CARTESIAN_POINT ( 'NONE',  ( -100.9371098987261917, -25.30060005375480614, 6.009289253917324380 ) ) ;
#87853 = ORIENTED_EDGE ( 'NONE', *, *, #37536, .T. ) ;
#87854 = CARTESIAN_POINT ( 'NONE',  ( -20.07547297788957152, 3.163885811906596679, 11.49999999999998934 ) ) ;
#87855 = VERTEX_POINT ( 'NONE', #29226 ) ;
#87856 = CARTESIAN_POINT ( 'NONE',  ( -32.55273188169832110, -23.96119346886880663, -0.6495511937831992544 ) ) ;
#87857 = CARTESIAN_POINT ( 'NONE',  ( -127.5906370802701844, -23.48786465467242124, 11.44779295918253403 ) ) ;
#87858 = ORIENTED_EDGE ( 'NONE', *, *, #71060, .T. ) ;
#87859 = CARTESIAN_POINT ( 'NONE',  ( -59.60446161964285494, -23.73791477778911840, 11.05961554403171299 ) ) ;
#87861 = ADVANCED_FACE ( 'NONE', ( #28734 ), #43955, .T. ) ;
#87860 = DIRECTION ( 'NONE',  ( 2.504262461560503484E-15, -6.886721769291384876E-15, 1.000000000000000000 ) ) ;
#87862 = CIRCLE ( 'NONE', #74885, 1.835999999999993859 ) ;
#87863 = DIRECTION ( 'NONE',  ( 0.000000000000000000, -1.000000000000000000, 0.000000000000000000 ) ) ;
#87864 = CARTESIAN_POINT ( 'NONE',  ( 14.81885032312887240, -15.09863332352077592, 11.49999999999999645 ) ) ;
#87865 = CC_DESIGN_APPROVAL ( #5419, ( #30849 ) ) ;
#87866 = CARTESIAN_POINT ( 'NONE',  ( 19.88262469969689050, -9.776007750257504014, 11.49999999999998934 ) ) ;
#87867 = EDGE_CURVE ( 'NONE', #36332, #67804, #37837, .T. ) ;
#87868 = CARTESIAN_POINT ( 'NONE',  ( 16.43461662053371697, -12.34185696772103391, -1.500000000000002220 ) ) ;
#87869 = VERTEX_POINT ( 'NONE', #21595 ) ;
#87870 = CARTESIAN_POINT ( 'NONE',  ( -113.5562042904833930, -23.47596703998600631, 11.44779298504227683 ) ) ;
#87871 = ORIENTED_EDGE ( 'NONE', *, *, #84386, .F. ) ;
#87872 = DIRECTION ( 'NONE',  ( -0.2488812114211667037, 0.000000000000000000, -0.9685340172660599212 ) ) ;
#87873 = CARTESIAN_POINT ( 'NONE',  ( 2.590395174287518643, -5.876774720514416295, 20.05492615153064762 ) ) ;
#87874 = ORIENTED_EDGE ( 'NONE', *, *, #55166, .F. ) ;
#87875 = ORIENTED_EDGE ( 'NONE', *, *, #38789, .F. ) ;
#87876 = ORIENTED_EDGE ( 'NONE', *, *, #41886, .F. ) ;
#87877 = CARTESIAN_POINT ( 'NONE',  ( 23.50000000000000000, 0.000000000000000000, 1.103411337323757735 ) ) ;
#87878 = B_SPLINE_CURVE_WITH_KNOTS ( 'NONE', 3,
 ( #88738, #87224, #26827, #3504, #19205, #17720 ),
 .UNSPECIFIED., .F., .F.,
 ( 4, 2, 4 ),
 ( 0.000000000000000000, 0.001380764517854763448, 0.002761529035709526896 ),
 .UNSPECIFIED. ) ;
#87879 = CARTESIAN_POINT ( 'NONE',  ( 7.166666666666668739, -5.876774720514419847, 20.78665865384614975 ) ) ;
#87880 = CARTESIAN_POINT ( 'NONE',  ( 6.259688558337090036, -6.376774720514413630, 19.73360741988579292 ) ) ;
#87881 = CARTESIAN_POINT ( 'NONE',  ( 12.06641648444584369, 16.80774221200798735, -1.500000000000002220 ) ) ;
#87882 = CARTESIAN_POINT ( 'NONE',  ( 21.13687465659472409, 4.681744431724916389, 11.49999999999999645 ) ) ;
#87883 = VERTEX_POINT ( 'NONE', #68793 ) ;
#87884 = FACE_BOUND ( 'NONE', #49197, .T. ) ;
#87885 = CARTESIAN_POINT ( 'NONE',  ( 2.598318274922708060, -5.876774720514413630, 19.68966562063331693 ) ) ;
#87886 = CARTESIAN_POINT ( 'NONE',  ( -8.193370562272118462, -20.86776251599019361, -1.500000000000002220 ) ) ;
#87887 = CARTESIAN_POINT ( 'NONE',  ( -124.5895376238167245, -23.48783264082479505, -1.443836473390058828 ) ) ;
#87888 = CARTESIAN_POINT ( 'NONE',  ( -102.5228709571501042, -24.66019654487200441, 8.947790411086119278 ) ) ;
#87889 = ORIENTED_EDGE ( 'NONE', *, *, #92413, .F. ) ;
#87890 = DIRECTION ( 'NONE',  ( -3.773278334453079618E-23, 0.9999999999976377785, 2.173523156925979975E-06 ) ) ;
#87891 = CARTESIAN_POINT ( 'NONE',  ( -116.4728709548940628, -25.21112548385455554, 2.000950967214103038 ) ) ;
#87892 = B_SPLINE_SURFACE_WITH_KNOTS ( 'NONE', 3, 3, ( 
 ( #965, #93810, #24793, #77571 ),
 ( #92802, #30910, #71490, #7576 ),
 ( #86201, #63896, #23283, #8075 ),
 ( #78567, #458, #40029, #70988 ),
 ( #94304, #62371, #1477, #39022 ),
 ( #32417, #17184, #15685, #38524 ),
 ( #69479, #31414, #93300, #19178 ),
 ( #73977, #73478, #4475, #26305 ),
 ( #57765, #50638, #35424, #10076 ),
 ( #43035, #27796, #19673, #87706 ) ),
 .UNSPECIFIED., .F., .F., .F.,
 ( 4, 3, 3, 4 ),
 ( 4, 4 ),
 ( 0.7022005934544806038, 0.7765311282028795059, 0.8508616629512784080, 0.9995227324480763231 ),
 ( 0.7495844612969405629, 0.7510439278013898434 ),
 .UNSPECIFIED. ) ;
#87893 = ORIENTED_EDGE ( 'NONE', *, *, #49216, .F. ) ;
#87894 = ORIENTED_EDGE ( 'NONE', *, *, #29862, .F. ) ;
#87895 = CARTESIAN_POINT ( 'NONE',  ( -46.62370101417344870, -24.66019654487199375, 8.947790411086122830 ) ) ;
#87896 = CC_DESIGN_DATE_AND_TIME_ASSIGNMENT ( #74338, #13923, ( #30849 ) ) ;
#87897 = EDGE_LOOP ( 'NONE', ( #50316, #22550, #58813, #76983 ) ) ;
#87898 = B_SPLINE_CURVE_WITH_KNOTS ( 'NONE', 3,
 ( #4544, #72553, #17759, #57837 ),
 .UNSPECIFIED., .F., .F.,
 ( 4, 4 ),
 ( 2.226473276209221022E-11, 0.003119410830149253137 ),
 .UNSPECIFIED. ) ;
#87899 = CIRCLE ( 'NONE', #68487, 6.119803529381341534 ) ;
#87900 = CARTESIAN_POINT ( 'NONE',  ( -24.90875734969025501, 5.965225279485572685, 26.43402280011862615 ) ) ;
#87901 = CARTESIAN_POINT ( 'NONE',  ( -19.34623641613454836, -8.721557147202650739, -1.500000000000002220 ) ) ;
#87902 = ORIENTED_EDGE ( 'NONE', *, *, #83463, .T. ) ;
#87903 = CARTESIAN_POINT ( 'NONE',  ( -88.63862431805245023, -23.73766607897670511, -1.055555164236456678 ) ) ;
#87904 = PRODUCT_DEFINITION_SHAPE ( 'NONE', 'NONE',  #19046 ) ;
#87905 = CARTESIAN_POINT ( 'NONE',  ( 16.38291735060997567, -14.39268585342195905, 11.49999999999998934 ) ) ;
#87906 = CARTESIAN_POINT ( 'NONE',  ( -103.5098569560838371, -24.66019654487200086, 8.947790411086115725 ) ) ;
#87907 = CARTESIAN_POINT ( 'NONE',  ( 6.420673076923079314, -6.376774720514427841, 21.83974358974358765 ) ) ;
#87908 = CARTESIAN_POINT ( 'NONE',  ( -35.62287095715004170, -24.14321612903113845, -0.2833117244521695666 ) ) ;
#87909 = CARTESIAN_POINT ( 'NONE',  ( -6.606886629844116676, -20.84447163495035937, -1.500000000000002220 ) ) ;
#87910 = CARTESIAN_POINT ( 'NONE',  ( 6.555906488453394410, -5.876774720514425177, 21.46941147007026274 ) ) ;
#87911 = EDGE_LOOP ( 'NONE', ( #90269, #64566, #37693, #73317 ) ) ;
#87912 = CARTESIAN_POINT ( 'NONE',  ( 6.727764423076923350, -6.376774720514413630, 19.76442307692307665 ) ) ;
#87913 = CARTESIAN_POINT ( 'NONE',  ( -9.940598223437577374, -6.376774720514426953, 22.08128695274315945 ) ) ;
#87914 = EDGE_LOOP ( 'NONE', ( #60556, #38357, #18361, #58601, #43967, #61333, #15813, #59777, #20499, #56608, #77397 ) ) ;
#87915 = CARTESIAN_POINT ( 'NONE',  ( -30.57842286860461911, -25.26764614148072496, 6.117730354831462769 ) ) ;
#87916 = EDGE_LOOP ( 'NONE', ( #31351, #81777, #23321, #48185 ) ) ;
#87917 = AXIS2_PLACEMENT_3D ( 'NONE', #35048, #27925, #78813 ) ;
#87918 = DIRECTION ( 'NONE',  ( -3.773278334453079030E-23, 0.9999999999976377785, 2.173523156925979128E-06 ) ) ;
#87919 = CARTESIAN_POINT ( 'NONE',  ( -82.64079165572177033, -23.73766607897671221, -1.055555164236435362 ) ) ;
#87920 = B_SPLINE_CURVE_WITH_KNOTS ( 'NONE', 3,
 ( #90104, #20578, #52043, #51051 ),
 .UNSPECIFIED., .F., .F.,
 ( 4, 4 ),
 ( 0.000000000000000000, 9.999999999997510880E-05 ),
 .UNSPECIFIED. ) ;
#87921 = CARTESIAN_POINT ( 'NONE',  ( -19.98547761299008130, 7.154247560337752887, 11.49999999999998934 ) ) ;
#87922 = CARTESIAN_POINT ( 'NONE',  ( 5.550000000000006040, -14.50000000000000178, 24.00000000000000000 ) ) ;
#87923 = CARTESIAN_POINT ( 'NONE',  ( -130.5728709571500588, -24.37728322581796192, 9.960208392924581489 ) ) ;
#87924 = CARTESIAN_POINT ( 'NONE',  ( -92.62287095715005592, -24.64965695001469115, 8.947790433994180503 ) ) ;
#87925 = FACE_OUTER_BOUND ( 'NONE', #34601, .T. ) ;
#87926 = CARTESIAN_POINT ( 'NONE',  ( -11.04204518803028456, 15.98388583709530941, 11.49999999999998934 ) ) ;
#87927 = CARTESIAN_POINT ( 'NONE',  ( -45.64360056886428652, -24.40034930558990922, 0.3402023900116019073 ) ) ;
#87928 = VERTEX_POINT ( 'NONE', #99708 ) ;
#87929 = CARTESIAN_POINT ( 'NONE',  ( 1.133552453683672745, -19.47370032599940615, 11.49999999999999645 ) ) ;
#87930 = CARTESIAN_POINT ( 'NONE',  ( -5.154768636056045850, -6.376774720514413630, 19.48351902941045921 ) ) ;
#87931 = EDGE_CURVE ( 'NONE', #78861, #12744, #51077, .T. ) ;
#87932 = FACE_OUTER_BOUND ( 'NONE', #8619, .T. ) ;
#87933 = EDGE_LOOP ( 'NONE', ( #49241, #45883, #23088 ) ) ;
#87934 = CARTESIAN_POINT ( 'NONE',  ( 4.931367317174526477, -5.876774720514419847, 20.61012727089847019 ) ) ;
#87935 = CARTESIAN_POINT ( 'NONE',  ( 25.61870917940689552, 5.965225279485572685, 28.79814474876421926 ) ) ;
#87936 = CARTESIAN_POINT ( 'NONE',  ( -90.52287095715009002, -23.48783264082477373, -1.443836473390088582 ) ) ;
#87937 = AXIS2_PLACEMENT_3D ( 'NONE', #43149, #27911, #89810 ) ;
#87938 = CARTESIAN_POINT ( 'NONE',  ( -81.67724764284677974, -25.24813850574973628, 6.915643883124781510 ) ) ;
#87939 = CARTESIAN_POINT ( 'NONE',  ( 0.7877182283408599162, 19.66719298131377514, 11.49999999999998934 ) ) ;
#87940 = CARTESIAN_POINT ( 'NONE',  ( 0.1645010273463760886, -1.417169167140626573, 0.3687607960183696965 ) ) ;
#87941 = VERTEX_POINT ( 'NONE', #85500 ) ;
#87942 = EDGE_CURVE ( 'NONE', #45475, #23903, #8381, .T. ) ;
#87943 = CARTESIAN_POINT ( 'NONE',  ( -7.970484365542752414, -10.32263987662778248, 1.301654676760341856 ) ) ;
#87944 = DIRECTION ( 'NONE',  ( 0.000000000000000000, -2.173523156925979552E-06, 0.9999999999976378895 ) ) ;
#87945 = EDGE_CURVE ( 'NONE', #79911, #38639, #63699, .T. ) ;
#87946 = CIRCLE ( 'NONE', #44199, 12.65241003308276113 ) ;
#87947 = SHAPE_DEFINITION_REPRESENTATION ( #89572, #22430 ) ;
#87948 = ORIENTED_EDGE ( 'NONE', *, *, #83123, .T. ) ;
#87949 = CARTESIAN_POINT ( 'NONE',  ( -125.5228709571501184, -23.85229601348998330, 10.88205029486207920 ) ) ;
#87950 = CARTESIAN_POINT ( 'NONE',  ( -2.148731487934370410, -6.376774720514411854, 19.46295461892501422 ) ) ;
#87951 = CARTESIAN_POINT ( 'NONE',  ( -108.9960569403308313, -25.24778904441513916, 3.815199558290551796 ) ) ;
#87952 = CARTESIAN_POINT ( 'NONE',  ( -29.52287095715006515, -24.41935721893828415, 9.387660007492499403 ) ) ;
#87953 = DIRECTION ( 'NONE',  ( -3.773278334453080206E-23, 0.9999999999976377785, 2.173523156925979975E-06 ) ) ;
#87954 = CARTESIAN_POINT ( 'NONE',  ( -69.41551097411255000, -25.31201709968604874, 5.862899404653265201 ) ) ;
#87955 = AXIS2_PLACEMENT_3D ( 'NONE', #25757, #56727, #55724 ) ;
#87956 = CARTESIAN_POINT ( 'NONE',  ( -79.52287095715006160, -23.96127896941631974, -0.6493128931038034679 ) ) ;
#87957 = CARTESIAN_POINT ( 'NONE',  ( -14.97016004668225264, 13.15154794113874637, 11.49999999999998934 ) ) ;
#87958 = EDGE_CURVE ( 'NONE', #42138, #40572, #7375, .T. ) ;
#87959 = CARTESIAN_POINT ( 'NONE',  ( -75.65600689415964553, -23.48786465467241058, 11.44779295918254824 ) ) ;
#87960 = CARTESIAN_POINT ( 'NONE',  ( 11.24879072547334324, 16.40116332625411033, -1.500000000000002220 ) ) ;
#87961 = VERTEX_POINT ( 'NONE', #15981 ) ;
#87962 = LINE ( 'NONE', #9829, #5372 ) ;
#87963 = CARTESIAN_POINT ( 'NONE',  ( -125.5228709571500616, -24.82558206586144678, 1.605769216559449042 ) ) ;
#87964 = CARTESIAN_POINT ( 'NONE',  ( -117.6228709571500559, -23.72773821059535493, 11.05748984161097503 ) ) ;
#87965 = CARTESIAN_POINT ( 'NONE',  ( -80.62512084407954660, -24.92592662359561473, 8.075495903017996469 ) ) ;
#87966 = CARTESIAN_POINT ( 'NONE',  ( 11.01739540223112357, 17.63107602209319680, 11.49999999999999645 ) ) ;
#87967 = DIRECTION ( 'NONE',  ( -3.773278334453079030E-23, 0.9999999999976377785, 2.173523156925979128E-06 ) ) ;
#87968 = CARTESIAN_POINT ( 'NONE',  ( -59.62287095715004881, -23.47593901973091235, -1.443836447539007972 ) ) ;
#87969 = CARTESIAN_POINT ( 'NONE',  ( 13.94817355369617751, 18.09530419158152625, 11.49999999999999645 ) ) ;
#87970 = VECTOR ( 'NONE', #69584, 1000.000000000000114 ) ;
#87971 = ORIENTED_EDGE ( 'NONE', *, *, #77646, .T. ) ;
#87972 = B_SPLINE_SURFACE_WITH_KNOTS ( 'NONE', 3, 1, ( 
 ( #45556, #21687 ),
 ( #53170, #67394 ),
 ( #76476, #83593 ),
 ( #90721, #75977 ),
 ( #30309, #59274 ),
 ( #6486, #74979 ),
 ( #98317, #21194 ) ),
 .UNSPECIFIED., .F., .F., .F.,
 ( 4, 1, 1, 1, 4 ),
 ( 2, 2 ),
 ( 0.000000000000000000, 0.2538796003266583501, 0.5030089172783559492, 0.7502910806899644180, 1.000000000000000000 ),
 ( 0.000000000000000000, 1.000000000000000000 ),
 .UNSPECIFIED. ) ;
#87973 = CARTESIAN_POINT ( 'NONE',  ( -54.92287095715008860, -23.47593901973090880, -1.443836447538998202 ) ) ;
#87974 = CARTESIAN_POINT ( 'NONE',  ( -127.6245366232018057, -23.73766607897670511, -1.055555164236447130 ) ) ;
#87975 = ORIENTED_EDGE ( 'NONE', *, *, #86241, .F. ) ;
#87976 = CARTESIAN_POINT ( 'NONE',  ( -13.29518446780263119, -15.22762515321373478, 11.49999999999998934 ) ) ;
#87977 = EDGE_CURVE ( 'NONE', #11670, #76617, #22585, .T. ) ;
#87978 = CARTESIAN_POINT ( 'NONE',  ( -106.5228709571500758, -24.66019654487200441, 8.947790411086112172 ) ) ;
#87979 = CARTESIAN_POINT ( 'NONE',  ( 5.184553252003285984, 6.475225279485573360, -28.06387035751381731 ) ) ;
#87980 = CIRCLE ( 'NONE', #86378, 2.499999999999998668 ) ;
#87981 = PLANE ( 'NONE',  #44380 ) ;
#87982 = ORIENTED_EDGE ( 'NONE', *, *, #72932, .T. ) ;
#87983 = CARTESIAN_POINT ( 'NONE',  ( -97.62287095715005592, -23.48783264082478794, -1.443836473390061936 ) ) ;
#87984 = CARTESIAN_POINT ( 'NONE',  ( -104.6228709571500559, -23.47596703998600631, 11.44779298504227860 ) ) ;
#87985 = CARTESIAN_POINT ( 'NONE',  ( 6.038693664686949347, 19.05185810397003721, -1.500000000000002220 ) ) ;
#87986 = AXIS2_PLACEMENT_3D ( 'NONE', #90065, #82445, #36285 ) ;
#87987 = CARTESIAN_POINT ( 'NONE',  ( 2.438461900574103502, 20.79476225230834174, 11.49999999999999645 ) ) ;
#87988 = CARTESIAN_POINT ( 'NONE',  ( -29.80787223232210437, -25.25360408432739945, 5.314274568547425304 ) ) ;
#87989 = CARTESIAN_POINT ( 'NONE',  ( 5.202077965628057576, 2.038091937962834166, 2.869745073849996442E-16 ) ) ;
#87990 = CARTESIAN_POINT ( 'NONE',  ( 13.62230711432095553, -17.35066874027886286, 11.49999999999998934 ) ) ;
#87991 = CARTESIAN_POINT ( 'NONE',  ( -39.85544541354917669, -25.31589298330722571, 4.937102986595060194 ) ) ;
#87993 = ORIENTED_EDGE ( 'NONE', *, *, #35149, .T. ) ;
#87992 = ADVANCED_FACE ( 'NONE', ( #78379 ), #1777, .F. ) ;
#87994 = FACE_OUTER_BOUND ( 'NONE', #88026, .T. ) ;
#87995 = CARTESIAN_POINT ( 'NONE',  ( -37.62287095715005592, -29.50248528299804818, 1.056150453629031594 ) ) ;
#87996 = PLANE ( 'NONE',  #49461 ) ;
#87997 = ORIENTED_EDGE ( 'NONE', *, *, #73131, .F. ) ;
#87998 = DIRECTION ( 'NONE',  ( 0.000000000000000000, 0.9999999999976377785, 2.173523156925979975E-06 ) ) ;
#87999 = VERTEX_POINT ( 'NONE', #70290 ) ;
#88000 = ORIENTED_EDGE ( 'NONE', *, *, #98205, .F. ) ;
#88001 = DIRECTION ( 'NONE',  ( -0.000000000000000000, -1.000000000000000000, -0.000000000000000000 ) ) ;
#88002 = CARTESIAN_POINT ( 'NONE',  ( 8.499999999999989342, 18.74999999999999645, 0.000000000000000000 ) ) ;
#88003 = CARTESIAN_POINT ( 'NONE',  ( -51.52287095715006160, -24.50216790748204687, 0.6166512839542488411 ) ) ;
#88004 = CARTESIAN_POINT ( 'NONE',  ( 7.506095096478735407, 19.11734572241606145, -1.500000000000002220 ) ) ;
#88005 = VERTEX_POINT ( 'NONE', #77876 ) ;
#88006 = CARTESIAN_POINT ( 'NONE',  ( 29.80070917940689768, 3.316774720514426456, 27.39560796525317343 ) ) ;
#88007 = LINE ( 'NONE', #10880, #49945 ) ;
#88008 = CARTESIAN_POINT ( 'NONE',  ( -83.52287095715000476, -24.34917612406836795, 0.1852690917426532413 ) ) ;
#88009 = CARTESIAN_POINT ( 'NONE',  ( -15.13915969582853549, -16.40262476207453801, 11.49999999999998934 ) ) ;
#88011 = CARTESIAN_POINT ( 'NONE',  ( 32.48725517365867432, -4.170878844625590887, -0.8993273505261454304 ) ) ;
#88010 = AXIS2_PLACEMENT_3D ( 'NONE', #62885, #54760, #32916 ) ;
#88012 = LINE ( 'NONE', #100075, #93444 ) ;
#88013 = VERTEX_POINT ( 'NONE', #45960 ) ;
#88014 = DIRECTION ( 'NONE',  ( -0.000000000000000000, -1.000000000000000000, -0.000000000000000000 ) ) ;
#88015 = CARTESIAN_POINT ( 'NONE',  ( -65.52287095715006160, -24.99132157543083821, 2.256160258750667502 ) ) ;
#88016 = CC_DESIGN_SECURITY_CLASSIFICATION ( #31288, ( #100429 ) ) ;
#88017 = CARTESIAN_POINT ( 'NONE',  ( 19.25983760003161294, 7.974354923662064998, 11.49999999999998934 ) ) ;
#88018 = VERTEX_POINT ( 'NONE', #24099 ) ;
#88020 = VERTEX_POINT ( 'NONE', #32715 ) ;
#88019 = PLANE ( 'NONE',  #24708 ) ;
#88021 = EDGE_CURVE ( 'NONE', #49715, #15581, #9378, .T. ) ;
#88022 = ORIENTED_EDGE ( 'NONE', *, *, #7505, .F. ) ;
#88023 = VECTOR ( 'NONE', #96657, 1000.000000000000114 ) ;
#88024 = DIRECTION ( 'NONE',  ( -3.773278334453079618E-23, 0.9999999999976377785, 2.173523156925979975E-06 ) ) ;
#88025 = CARTESIAN_POINT ( 'NONE',  ( -17.44821286160079410, -11.81026508430653088, -1.500000000000002220 ) ) ;
#88026 = EDGE_LOOP ( 'NONE', ( #35576, #54840, #18808, #53654 ) ) ;
#88027 = DIRECTION ( 'NONE',  ( 0.000000000000000000, 1.000000000000000000, 1.084202172485504311E-16 ) ) ;
#88028 = FACE_OUTER_BOUND ( 'NONE', #51711, .T. ) ;
#88029 = DIRECTION ( 'NONE',  ( -0.000000000000000000, 0.000000000000000000, -1.000000000000000000 ) ) ;
#88030 = ADVANCED_FACE ( 'NONE', ( #77378, #62186 ), #54079, .F. ) ;
#88031 = VECTOR ( 'NONE', #82664, 1000.000000000000114 ) ;
#88032 = CARTESIAN_POINT ( 'NONE',  ( -100.7317701684513764, -25.03152445186833219, 7.544846145421804984 ) ) ;
#88033 = CARTESIAN_POINT ( 'NONE',  ( -59.61135775242147616, -23.48783264082476308, -1.443836473390097908 ) ) ;
#88034 = CARTESIAN_POINT ( 'NONE',  ( 17.51545567653809954, -12.82042131148251229, -1.500000000000002220 ) ) ;
#88035 = CARTESIAN_POINT ( 'NONE',  ( -80.60699767246597958, -25.12224391340353691, 7.098406057649814471 ) ) ;
#88037 = VERTEX_POINT ( 'NONE', #55068 ) ;
#88036 = CARTESIAN_POINT ( 'NONE',  ( -2.790049085472659396, -22.09070898310802633, 11.49999999999999645 ) ) ;
#88038 = DIRECTION ( 'NONE',  ( -1.000000000000000000, -0.000000000000000000, -0.000000000000000000 ) ) ;
#88039 = DIRECTION ( 'NONE',  ( 0.000000000000000000, -1.000000000000000000, 0.000000000000000000 ) ) ;
#88040 = CYLINDRICAL_SURFACE ( 'NONE', #5104, 129.7684398600581517 ) ;
#88041 = ORIENTED_EDGE ( 'NONE', *, *, #9570, .F. ) ;
#88042 = EDGE_CURVE ( 'NONE', #90447, #41368, #95660, .T. ) ;
#88043 = EDGE_CURVE ( 'NONE', #896, #72639, #92609, .T. ) ;
#88045 = VERTEX_POINT ( 'NONE', #94111 ) ;
#88044 = CARTESIAN_POINT ( 'NONE',  ( -5.988734693054777125, -6.376774720514415407, 19.95737465391042065 ) ) ;
#88046 = ORIENTED_EDGE ( 'NONE', *, *, #81891, .F. ) ;
#88047 = EDGE_CURVE ( 'NONE', #100004, #79632, #92162, .T. ) ;
#88048 = LINE ( 'NONE', #55603, #95094 ) ;
#88049 = CYLINDRICAL_SURFACE ( 'NONE', #9702, 1.150000000000003464 ) ;
#88050 = CARTESIAN_POINT ( 'NONE',  ( 23.50000000000000000, 0.000000000000000000, -1.103411337323757957 ) ) ;
#88051 = ORIENTED_EDGE ( 'NONE', *, *, #31811, .F. ) ;
#88052 = CARTESIAN_POINT ( 'NONE',  ( -130.5728709571500588, -24.30959152078064989, -0.1101050347254430017 ) ) ;
#88053 = CARTESIAN_POINT ( 'NONE',  ( -13.11617634606977489, 18.14055439154125438, -1.500000000000002220 ) ) ;
#88054 = EDGE_CURVE ( 'NONE', #15484, #62407, #67929, .T. ) ;
#88055 = ORIENTED_EDGE ( 'NONE', *, *, #74935, .F. ) ;
#88056 = CARTESIAN_POINT ( 'NONE',  ( -112.5526642601108165, -24.35071581493543391, 9.817618358456016381 ) ) ;
#88058 = DIRECTION ( 'NONE',  ( 0.000000000000000000, 0.000000000000000000, -1.000000000000000000 ) ) ;
#88057 = VECTOR ( 'NONE', #62841, 1000.000000000000000 ) ;
#88059 = LINE ( 'NONE', #18034, #34488 ) ;
#88060 = CARTESIAN_POINT ( 'NONE',  ( -125.5228709571500616, -25.00158670708909980, 2.256160236439166411 ) ) ;
#88061 = CARTESIAN_POINT ( 'NONE',  ( -63.92296805384962965, -24.66459861931856778, 1.095224832288508976 ) ) ;
#88062 = CARTESIAN_POINT ( 'NONE',  ( -4.924063254364682507, -18.92933890202812464, -1.500000000000002220 ) ) ;
#88063 = VECTOR ( 'NONE', #61640, 1000.000000000000114 ) ;
#88064 = FACE_OUTER_BOUND ( 'NONE', #13721, .T. ) ;
#88065 = ORIENTED_EDGE ( 'NONE', *, *, #72726, .F. ) ;
#88066 = CARTESIAN_POINT ( 'NONE',  ( -10.19830463584622571, -18.94658877215714909, -1.500000000000002220 ) ) ;
#88067 = CARTESIAN_POINT ( 'NONE',  ( -19.38764004357183524, -5.965225279485572685, -21.62823517627350611 ) ) ;
#88068 = CARTESIAN_POINT ( 'NONE',  ( -71.08634551208074015, -25.12219073911204248, 6.775733800420372432 ) ) ;
#88069 = FACE_OUTER_BOUND ( 'NONE', #65233, .T. ) ;
#88070 = CARTESIAN_POINT ( 'NONE',  ( -10.24059822343757808, -5.876774720514426953, 17.91871304725684766 ) ) ;
#88071 = CARTESIAN_POINT ( 'NONE',  ( -21.95939045666098366, -6.591442671832903777, -1.500000000000002220 ) ) ;
#88072 = EDGE_CURVE ( 'NONE', #54059, #12135, #25610, .T. ) ;
#88073 = B_SPLINE_CURVE_WITH_KNOTS ( 'NONE', 3,
 ( #9344, #2253, #17461, #25066, #42328, #80367 ),
 .UNSPECIFIED., .F., .F.,
 ( 4, 2, 4 ),
 ( 1.570755371634052715E-05, 0.001396183895866089705, 0.002776660238015838614 ),
 .UNSPECIFIED. ) ;
#88074 = EDGE_CURVE ( 'NONE', #55689, #14852, #9855, .T. ) ;
#88075 = DATE_TIME_ROLE ( 'creation_date' ) ;
#88076 = CARTESIAN_POINT ( 'NONE',  ( -102.9228709571500673, -23.47596703998600631, 11.44779298504227683 ) ) ;
#88077 = DIRECTION ( 'NONE',  ( -1.000000000000000000, 0.000000000000000000, 0.000000000000000000 ) ) ;
#88078 = CARTESIAN_POINT ( 'NONE',  ( -1.290058840521481454, 20.04182742388497473, 11.49999999999999645 ) ) ;
#88079 = CARTESIAN_POINT ( 'NONE',  ( -110.3139465455115129, -25.28814068893017719, 2.832404430835924636 ) ) ;
#88080 = CARTESIAN_POINT ( 'NONE',  ( -32.58046570376392026, -24.51419770103159834, 9.386484678747182286 ) ) ;
#88081 = CARTESIAN_POINT ( 'NONE',  ( -99.52287095715007581, -24.51283580621461766, 0.6167428607048592859 ) ) ;
#88082 = DIRECTION ( 'NONE',  ( 0.000000000000000000, 0.000000000000000000, 1.000000000000000000 ) ) ;
#88083 = B_SPLINE_CURVE_WITH_KNOTS ( 'NONE', 3,
 ( #28688, #67764, #21060, #98686, #37304, #29180 ),
 .UNSPECIFIED., .F., .F.,
 ( 4, 2, 4 ),
 ( 1.570887131794795405E-05, 0.001396322306279761940, 0.002776935741241575838 ),
 .UNSPECIFIED. ) ;
#88084 = CARTESIAN_POINT ( 'NONE',  ( -27.96875734969026084, -6.376774720514426953, 0.7300228001186309656 ) ) ;
#88085 = CARTESIAN_POINT ( 'NONE',  ( 17.59243620335545799, -9.192777620008959261, -1.500000000000002220 ) ) ;
#88086 = EDGE_CURVE ( 'NONE', #64103, #78888, #27903, .T. ) ;
#88087 = CARTESIAN_POINT ( 'NONE',  ( -40.52287095715007581, -25.00182538069145011, 7.747789668545104647 ) ) ;
#88088 = CARTESIAN_POINT ( 'NONE',  ( -6.756748142665309764, -18.51622224137248907, -1.500000000000002220 ) ) ;
#88089 = CARTESIAN_POINT ( 'NONE',  ( -42.65524057351728260, -23.73766607897670156, -1.055555164236442689 ) ) ;
#88090 = EDGE_CURVE ( 'NONE', #32327, #39562, #14593, .T. ) ;
#88091 = VECTOR ( 'NONE', #87918, 1000.000000000000114 ) ;
#88092 = EDGE_CURVE ( 'NONE', #41774, #24375, #73921, .T. ) ;
#88093 = DIRECTION ( 'NONE',  ( 0.000000000000000000, 0.000000000000000000, -1.000000000000000000 ) ) ;
#88094 = CALENDAR_DATE ( 2026, 9, 10 ) ;
#88095 = CARTESIAN_POINT ( 'NONE',  ( -3.749999999999999112, 25.69999999999999574, 2.100000000000000089 ) ) ;
#88096 = CARTESIAN_POINT ( 'NONE',  ( -111.5228709571500616, -24.51283580621365843, 0.6167428607019709297 ) ) ;
#88097 = CARTESIAN_POINT ( 'NONE',  ( -7.709890279958820258, -19.11728055126480186, 11.49999999999999645 ) ) ;
#88098 = CARTESIAN_POINT ( 'NONE',  ( -128.5228709571501042, -24.66019654487200441, 8.947790411086108620 ) ) ;
#88099 = CIRCLE ( 'NONE', #29776, 2.249999999999998668 ) ;
#88100 = CARTESIAN_POINT ( 'NONE',  ( 2.978076788109338402, -22.46882643481310282, 11.49999999999999645 ) ) ;
#88101 = ORIENTED_EDGE ( 'NONE', *, *, #2009, .F. ) ;
#88102 = CARTESIAN_POINT ( 'NONE',  ( -115.5895376238166961, -25.00182538069145721, 7.747789668545099317 ) ) ;
#88103 = CARTESIAN_POINT ( 'NONE',  ( -97.63001613934683576, -24.15543982623907837, -0.2315651400026600415 ) ) ;
#88104 = CARTESIAN_POINT ( 'NONE',  ( -26.13109729691315053, -24.94783878638828867, 4.221025441685607227 ) ) ;
#88105 = VECTOR ( 'NONE', #84909, 1000.000000000000227 ) ;
#88106 = CARTESIAN_POINT ( 'NONE',  ( -110.7941382621162631, -25.26164770502454715, 6.209434163990041888 ) ) ;
#88107 = PLANE ( 'NONE',  #93321 ) ;
#88108 = VERTEX_POINT ( 'NONE', #42850 ) ;
#88109 = CARTESIAN_POINT ( 'NONE',  ( -79.46066275308743343, -25.26749986018558403, 5.472043613161642561 ) ) ;
#88110 = CARTESIAN_POINT ( 'NONE',  ( -21.14637036216210575, 8.611126525438130841, -1.500000000000002220 ) ) ;
#88111 = LINE ( 'NONE', #49055, #68102 ) ;
#88112 = DIRECTION ( 'NONE',  ( 1.252131230780251742E-15, -6.886721769291384876E-15, 1.000000000000000000 ) ) ;
#88113 = LINE ( 'NONE', #32818, #74386 ) ;
#88114 = CARTESIAN_POINT ( 'NONE',  ( 22.09666729679958053, 4.251135690456572469, 11.49999999999999645 ) ) ;
#88115 = ORIENTED_EDGE ( 'NONE', *, *, #64627, .T. ) ;
#88116 = LINE ( 'NONE', #25702, #43276 ) ;
#88117 = CARTESIAN_POINT ( 'NONE',  ( -19.92591009635028243, 9.278653061003369729, -1.500000000000002220 ) ) ;
#88118 = CARTESIAN_POINT ( 'NONE',  ( -114.5228709571500758, -23.72773821059536914, 11.05748984161097326 ) ) ;
#88119 = B_SPLINE_CURVE_WITH_KNOTS ( 'NONE', 3,
 ( #66290, #91094, #91591, #82976 ),
 .UNSPECIFIED., .F., .F.,
 ( 4, 4 ),
 ( 0.5601859395450292656, 0.5691923708171451324 ),
 .UNSPECIFIED. ) ;
#88120 = CARTESIAN_POINT ( 'NONE',  ( -111.6272352480785770, -24.15543982623907482, -0.2315651400026575712 ) ) ;
#88121 = DIRECTION ( 'NONE',  ( -3.773278334453079618E-23, 0.9999999999976377785, 2.173523156925979975E-06 ) ) ;
#88122 = VERTEX_POINT ( 'NONE', #72293 ) ;
#88123 = CARTESIAN_POINT ( 'NONE',  ( -48.58197809690042135, -24.51419770103156637, 9.386484678747178734 ) ) ;
#88124 = CARTESIAN_POINT ( 'NONE',  ( -0.08860454909227881426, -6.376774720514410077, 19.21747685089457036 ) ) ;
#88125 = EDGE_LOOP ( 'NONE', ( #3196, #39909, #16650, #13098 ) ) ;
#88126 = CARTESIAN_POINT ( 'NONE',  ( -104.5228709571500758, -29.50248528299804818, 1.056150453629042030 ) ) ;
#88127 = CARTESIAN_POINT ( 'NONE',  ( 10.70087849588422380, -17.49211976490306597, -1.500000000000002220 ) ) ;
#88128 = ORIENTED_EDGE ( 'NONE', *, *, #53679, .T. ) ;
#88129 = VERTEX_POINT ( 'NONE', #80397 ) ;
#88130 = ORIENTED_EDGE ( 'NONE', *, *, #94370, .F. ) ;
#88131 = CARTESIAN_POINT ( 'NONE',  ( -50.04740315932213690, -25.31331832774112556, 5.238437981263384557 ) ) ;
#88132 = CARTESIAN_POINT ( 'NONE',  ( 23.08992502549420323, -0.8469403905869224980, 11.49999999999998934 ) ) ;
#88133 = LINE ( 'NONE', #64318, #26079 ) ;
#88134 = CARTESIAN_POINT ( 'NONE',  ( -15.63206872509828571, 12.99414084278249071, -1.500000000000002220 ) ) ;
#88135 = CIRCLE ( 'NONE', #5542, 19.30000000000000071 ) ;
#88136 = ORIENTED_EDGE ( 'NONE', *, *, #87507, .F. ) ;
#88137 = CYLINDRICAL_SURFACE ( 'NONE', #65548, 11.85241003308275864 ) ;
#88138 = CARTESIAN_POINT ( 'NONE',  ( -29.59427457724074984, -24.07687357297128727, 10.23563548314527338 ) ) ;
#88139 = CARTESIAN_POINT ( 'NONE',  ( -44.58953762381672448, -24.66019654487199375, 8.947790411086137041 ) ) ;
#88140 = CARTESIAN_POINT ( 'NONE',  ( -35.62287095715005592, -23.47593901973091235, -1.443836447539011525 ) ) ;
#88141 = ORIENTED_EDGE ( 'NONE', *, *, #95520, .F. ) ;
#88142 = CARTESIAN_POINT ( 'NONE',  ( -28.81395509834238311, -24.76880987794397626, 2.889656594307629334 ) ) ;
#88144 = VECTOR ( 'NONE', #14589, 1000.000000000000000 ) ;
#88143 = DIRECTION ( 'NONE',  ( 0.000000000000000000, -0.9999999999976377785, -2.173523156925979975E-06 ) ) ;
#88145 = ORIENTED_EDGE ( 'NONE', *, *, #17346, .F. ) ;
#88146 = CARTESIAN_POINT ( 'NONE',  ( -11.59579830748209517, 17.24510332420730663, 11.49999999999998934 ) ) ;
#88147 = EDGE_LOOP ( 'NONE', ( #16867, #70647, #74690, #61270 ) ) ;
#88149 = ORIENTED_EDGE ( 'NONE', *, *, #41585, .F. ) ;
#88148 = CARTESIAN_POINT ( 'NONE',  ( -125.5545359397194147, -24.73486907724918638, 1.287355809206972346 ) ) ;
#88150 = EDGE_CURVE ( 'NONE', #10013, #36340, #22577, .T. ) ;
#88151 = CARTESIAN_POINT ( 'NONE',  ( 32.06540688909006320, 1.682774720514426114, -12.44045471929205604 ) ) ;
#88152 = CARTESIAN_POINT ( 'NONE',  ( -102.6228709571500559, -23.72747288104442021, -1.053458166803661333 ) ) ;
#88153 = ORIENTED_EDGE ( 'NONE', *, *, #50462, .T. ) ;
#88154 = ORIENTED_EDGE ( 'NONE', *, *, #58026, .T. ) ;
#88155 = CARTESIAN_POINT ( 'NONE',  ( -114.6228709571500701, -23.96127896941633040, -0.6493128931037811524 ) ) ;
#88156 = CARTESIAN_POINT ( 'NONE',  ( -28.52287095715005805, -24.48903441264110015, 8.947790432046794251 ) ) ;
#88157 = PLANE ( 'NONE',  #48138 ) ;
#88159 = ORIENTED_EDGE ( 'NONE', *, *, #50757, .F. ) ;
#88158 = CARTESIAN_POINT ( 'NONE',  ( -12.21066354923914865, 18.40238043084326591, 11.49999999999999645 ) ) ;
#88160 = CARTESIAN_POINT ( 'NONE',  ( -49.11050743085840509, -25.16124551768960416, 6.935735280119078361 ) ) ;
#88161 = CARTESIAN_POINT ( 'NONE',  ( 5.419076944403256491, 21.93356404788375258, -1.500000000000002220 ) ) ;
#88162 = EDGE_CURVE ( 'NONE', #12021, #95021, #50449, .T. ) ;
#88163 = ADVANCED_FACE ( 'NONE', ( #26614 ), #2787, .T. ) ;
#88164 = ADVANCED_FACE ( 'NONE', ( #40830 ), #64707, .T. ) ;
#88166 = VERTEX_POINT ( 'NONE', #95622 ) ;
#88165 = CARTESIAN_POINT ( 'NONE',  ( -80.34687923781922336, -25.13069340115295702, 2.947789388436138136 ) ) ;
#88167 = EDGE_LOOP ( 'NONE', ( #6285, #47910, #18622, #17451, #13486, #89933, #39358, #63361, #56020, #69918, #4432, #49456 ) ) ;
#88168 = EDGE_CURVE ( 'NONE', #66710, #55229, #56072, .T. ) ;
#88169 = DIRECTION ( 'NONE',  ( 1.734723475976801178E-15, 1.000000000000000000, -0.000000000000000000 ) ) ;
#88170 = CARTESIAN_POINT ( 'NONE',  ( -36.62287095715005592, -24.64965695001467694, 8.947790433994187609 ) ) ;
#88171 = ORIENTED_EDGE ( 'NONE', *, *, #86998, .T. ) ;
#88172 = CARTESIAN_POINT ( 'NONE',  ( -21.15187133135857422, -0.9709546189074961253, -1.500000000000002220 ) ) ;
#88173 = CARTESIAN_POINT ( 'NONE',  ( 30.61752088227329693, -5.013017886559611114, 27.44065105897852419 ) ) ;
#88174 = CARTESIAN_POINT ( 'NONE',  ( -7.326923076923076650, -6.376774720514417183, 20.36318108974359831 ) ) ;
#88176 = B_SPLINE_CURVE_WITH_KNOTS ( 'NONE', 3,
 ( #14608, #69406, #60807, #54689, #85121, #15112 ),
 .UNSPECIFIED., .F., .F.,
 ( 4, 2, 4 ),
 ( 0.000000000000000000, 0.001381645800452327389, 0.002763291600904654779 ),
 .UNSPECIFIED. ) ;
#88175 = CARTESIAN_POINT ( 'NONE',  ( -126.5228709571500616, -29.50247984919015209, -1.443849546365044922 ) ) ;
#88177 = CARTESIAN_POINT ( 'NONE',  ( 19.86420646539740176, -9.926203236129387264, -1.500000000000002220 ) ) ;
#88178 = CARTESIAN_POINT ( 'NONE',  ( -114.5192691221986507, -23.96119346886881374, -0.6495511937831859317 ) ) ;
#88179 = EDGE_CURVE ( 'NONE', #21001, #37842, #6385, .T. ) ;
#88180 = ORIENTED_EDGE ( 'NONE', *, *, #82454, .T. ) ;
#88181 = CARTESIAN_POINT ( 'NONE',  ( -88.62287095715004170, -24.65952944569304606, 1.056160979905700570 ) ) ;
#88182 = CARTESIAN_POINT ( 'NONE',  ( -104.5562042904834072, -23.47593901973091235, -1.443836447539001089 ) ) ;
#88183 = CARTESIAN_POINT ( 'NONE',  ( -41.57990624374743760, -25.19387363311069805, 3.356451906250546457 ) ) ;
#88184 = CARTESIAN_POINT ( 'NONE',  ( 20.52151214508650057, 3.625915217019311583E-15, -1.700000000000000178 ) ) ;
#88185 = EDGE_CURVE ( 'NONE', #44058, #20835, #86055, .T. ) ;
#88186 = CARTESIAN_POINT ( 'NONE',  ( 4.731349760756693890, 18.90081699332259646, 11.49999999999998934 ) ) ;
#88187 = CARTESIAN_POINT ( 'NONE',  ( 20.52986552169224410, -6.224258026782483633, -1.500000000000002220 ) ) ;
#88188 = DIRECTION ( 'NONE',  ( -1.000000000000000000, 0.000000000000000000, 1.895872651340772790E-16 ) ) ;
#88189 = CARTESIAN_POINT ( 'NONE',  ( -1.267404104715736279, -6.376774720514413630, 19.66076420632889921 ) ) ;
#88190 = CARTESIAN_POINT ( 'NONE',  ( 19.72776355195876263, -5.965225279485572685, 28.39950002376592764 ) ) ;
#88191 = CARTESIAN_POINT ( 'NONE',  ( -77.60587273036531997, -23.48783264082476663, -1.443836473390097241 ) ) ;
#88193 = VECTOR ( 'NONE', #69093, 1000.000000000000114 ) ;
#88192 = CARTESIAN_POINT ( 'NONE',  ( 21.73672277138745201, -6.736064506363727666, -1.500000000000002220 ) ) ;
#88194 = EDGE_CURVE ( 'NONE', #7527, #53428, #81216, .T. ) ;
#88195 = CARTESIAN_POINT ( 'NONE',  ( -102.5490437353218880, -24.51314013834317151, 0.6176544820404245018 ) ) ;
#88196 = CARTESIAN_POINT ( 'NONE',  ( 8.971512145086503409, -1.000000000000001110, -3.746884140868835367 ) ) ;
#88197 = CARTESIAN_POINT ( 'NONE',  ( 18.24224480919323810, -7.949361806615760528, 11.49999999999999645 ) ) ;
#88198 = CARTESIAN_POINT ( 'NONE',  ( -104.5134582497340858, -24.34968618360934300, 0.1864209137778872205 ) ) ;
#88199 = B_SPLINE_CURVE_WITH_KNOTS ( 'NONE', 3,
 ( #75863, #13467, #51554, #98705, #29204, #89607 ),
 .UNSPECIFIED., .F., .F.,
 ( 4, 2, 4 ),
 ( 6.384118695040667903E-06, 0.001386860460836587166, 0.002767336802978133652 ),
 .UNSPECIFIED. ) ;
#88200 = CARTESIAN_POINT ( 'NONE',  ( -87.62287095715004170, -24.64965695001468404, 8.947790433994180503 ) ) ;
#88201 = CARTESIAN_POINT ( 'NONE',  ( -48.59960436616349710, -23.96119346886880663, -0.6495511937831938143 ) ) ;
#88202 = EDGE_LOOP ( 'NONE', ( #9252, #63318, #30240, #86800 ) ) ;
#88203 = DIRECTION ( 'NONE',  ( 0.000000000000000000, 2.173523156925980399E-06, -0.9999999999976378895 ) ) ;
#88204 = CARTESIAN_POINT ( 'NONE',  ( 29.80070917940689412, 0.6647747205144266536, 27.39560796525321607 ) ) ;
#88205 = EDGE_CURVE ( 'NONE', #67306, #58916, #42043, .T. ) ;
#88206 = AXIS2_PLACEMENT_3D ( 'NONE', #50189, #13100, #58307 ) ;
#88207 = CARTESIAN_POINT ( 'NONE',  ( 21.69746526873944958, -0.4026533170205861545, 11.49999999999998934 ) ) ;
#88208 = CARTESIAN_POINT ( 'NONE',  ( -56.65019691563739457, -23.73791477778912196, 11.05961554403170766 ) ) ;
#88209 = CARTESIAN_POINT ( 'NONE',  ( -13.24781383850973349, 14.34467480260970795, -1.500000000000002220 ) ) ;
#88210 = DIRECTION ( 'NONE',  ( -0.000000000000000000, -1.000000000000000000, -0.000000000000000000 ) ) ;
#88211 = EDGE_CURVE ( 'NONE', #96640, #25971, #51947, .T. ) ;
#88212 = VERTEX_POINT ( 'NONE', #19989 ) ;
#88213 = PERSON_AND_ORGANIZATION ( #70597, #27821 ) ;
#88214 = DIRECTION ( 'NONE',  ( 0.9796027006414893545, -4.367567496269849188E-07, 0.2009441437208608627 ) ) ;
#88215 = CARTESIAN_POINT ( 'NONE',  ( 19.37909195245082472, -6.530858791768283211, 11.49999999999999645 ) ) ;
#88216 = FACE_OUTER_BOUND ( 'NONE', #94880, .T. ) ;
#88217 = B_SPLINE_CURVE_WITH_KNOTS ( 'NONE', 3,
 ( #16501, #94637, #9900, #7898, #93625, #56093, #48483, #86025 ),
 .UNSPECIFIED., .F., .F.,
 ( 4, 2, 2, 4 ),
 ( 0.000000000000000000, 0.0002157442958532924937, 0.0004314885917065849875, 0.0008629771834131835274 ),
 .UNSPECIFIED. ) ;
#88218 = EDGE_CURVE ( 'NONE', #95881, #95239, #50956, .T. ) ;
#88219 = B_SPLINE_CURVE_WITH_KNOTS ( 'NONE', 3,
 ( #65882, #96804, #66375, #27788 ),
 .UNSPECIFIED., .F., .F.,
 ( 4, 4 ),
 ( 0.000000000000000000, 1.000000000000000000 ),
 .UNSPECIFIED. ) ;
#88220 = CARTESIAN_POINT ( 'NONE',  ( -118.6228709571500843, -24.34917612406838217, 0.1852690917426704775 ) ) ;
#88221 = ORIENTED_EDGE ( 'NONE', *, *, #29482, .F. ) ;
#88222 = LINE ( 'NONE', #35918, #2191 ) ;
#88223 = DIRECTION ( 'NONE',  ( 1.257682986112628661E-16, 0.000000000000000000, 1.000000000000000000 ) ) ;
#88224 = CARTESIAN_POINT ( 'NONE',  ( 0.9626393376689279524, 13.76638389358553916, 0.000000000000000000 ) ) ;
#88225 = CARTESIAN_POINT ( 'NONE',  ( -40.52195330627272796, -23.48786465467240347, 11.44779295918255180 ) ) ;
#88226 = CARTESIAN_POINT ( 'NONE',  ( -67.62287095715008434, -23.47596703998600276, 11.44779298504227505 ) ) ;
#88227 = VERTEX_POINT ( 'NONE', #13364 ) ;
#88228 = DIRECTION ( 'NONE',  ( -0.000000000000000000, 1.000000000000000000, -0.000000000000000000 ) ) ;
#88229 = CARTESIAN_POINT ( 'NONE',  ( -19.49525799874905729, 12.17417675796824561, 11.49999999999999645 ) ) ;
#88230 = CARTESIAN_POINT ( 'NONE',  ( 10.71911242904675987, 20.06137936439360203, -1.500000000000002220 ) ) ;
#88231 = CARTESIAN_POINT ( 'NONE',  ( -110.5486993749513687, -24.92592662359561473, 8.075495903018000021 ) ) ;
#88232 = DIRECTION ( 'NONE',  ( 0.000000000000000000, -1.000000000000000000, 0.000000000000000000 ) ) ;
#88233 = CARTESIAN_POINT ( 'NONE',  ( -90.59981940747849194, -23.85016227208580730, -0.8807180028928307536 ) ) ;
#88234 = AXIS2_PLACEMENT_3D ( 'NONE', #96307, #33910, #43028 ) ;
#88235 = LINE ( 'NONE', #18698, #23627 ) ;
#88236 = CARTESIAN_POINT ( 'NONE',  ( -89.52287095715010423, -23.96127896942128999, -0.6493128930940261778 ) ) ;
#88237 = CARTESIAN_POINT ( 'NONE',  ( -15.13543854793762300, 15.80457324685279374, 11.49999999999998934 ) ) ;
#88238 = CYLINDRICAL_SURFACE ( 'NONE', #23538, 18.50000000000000000 ) ;
#88239 = CARTESIAN_POINT ( 'NONE',  ( -49.62744005137184899, -25.31563369538250541, 5.001783013947322942 ) ) ;
#88240 = DIRECTION ( 'NONE',  ( -0.000000000000000000, -1.000000000000000000, 0.000000000000000000 ) ) ;
#88241 = CARTESIAN_POINT ( 'NONE',  ( -58.59295713816230489, -24.15543982623907127, -0.2315651400026660645 ) ) ;
#88242 = ORIENTED_EDGE ( 'NONE', *, *, #47543, .F. ) ;
#88243 = CARTESIAN_POINT ( 'NONE',  ( -20.33632446988539400, 1.880062042347348195, 11.49999999999998934 ) ) ;
#88244 = EDGE_LOOP ( 'NONE', ( #41590, #56077, #87206, #38685, #48065, #46322, #98211, #60076 ) ) ;
#88245 = ORIENTED_EDGE ( 'NONE', *, *, #51393, .F. ) ;
#88246 = CARTESIAN_POINT ( 'NONE',  ( 13.47786528765806580, -18.65256936556403744, 11.49999999999998934 ) ) ;
#88247 = CARTESIAN_POINT ( 'NONE',  ( 14.92791587776674334, -5.037605299509789525, -27.26084882802267373 ) ) ;
#88248 = ORIENTED_EDGE ( 'NONE', *, *, #7350, .T. ) ;
#88249 = B_SPLINE_CURVE_WITH_KNOTS ( 'NONE', 3,
 ( #15822, #68130, #76707, #45786, #68624, #31552, #62016 ),
 .UNSPECIFIED., .F., .F.,
 ( 4, 1, 1, 1, 4 ),
 ( 0.000000000000000000, 0.2835948081386937547, 0.5433948405759735367, 0.7806456291745620391, 1.000000000000000000 ),
 .UNSPECIFIED. ) ;
#88250 = LINE ( 'NONE', #11116, #70371 ) ;
#88251 = FACE_BOUND ( 'NONE', #60200, .T. ) ;
#88252 = CARTESIAN_POINT ( 'NONE',  ( -41.62287095715007013, -24.50321055353804311, 9.387540953477543582 ) ) ;
#88254 = ORIENTED_EDGE ( 'NONE', *, *, #30542, .T. ) ;
#88253 = CARTESIAN_POINT ( 'NONE',  ( -0.3244385709253747585, -21.36021439428519386, 11.49999999999999645 ) ) ;
#88255 = B_SPLINE_CURVE_WITH_KNOTS ( 'NONE', 3,
 ( #54526, #71757, #32680, #47416, #70751, #31682 ),
 .UNSPECIFIED., .F., .F.,
 ( 4, 2, 4 ),
 ( 0.000000000000000000, 0.001380901958385387894, 0.002761803916770775788 ),
 .UNSPECIFIED. ) ;
#88256 = ORIENTED_EDGE ( 'NONE', *, *, #79308, .T. ) ;
#88257 = CARTESIAN_POINT ( 'NONE',  ( -14.87450875942801254, -16.50811611944624602, 11.49999999999998934 ) ) ;
#88258 = CARTESIAN_POINT ( 'NONE',  ( 16.58470376584361361, 12.37529123428901556, 11.49999999999998934 ) ) ;
#88259 = ORIENTED_EDGE ( 'NONE', *, *, #65140, .T. ) ;
#88260 = CARTESIAN_POINT ( 'NONE',  ( -6.265203266387573855, -6.376774720514408301, 19.29154511076646017 ) ) ;
#88261 = CARTESIAN_POINT ( 'NONE',  ( -104.6228709571500559, -29.50247984919015209, -1.443849546365050029 ) ) ;
#88262 = ORIENTED_EDGE ( 'NONE', *, *, #98026, .F. ) ;
#88263 = ADVANCED_FACE ( 'NONE', ( #44340 ), #12370, .F. ) ;
#88264 = CARTESIAN_POINT ( 'NONE',  ( -56.52287095715006870, -24.64898659630367916, 1.056161002820822592 ) ) ;
#88265 = ORIENTED_EDGE ( 'NONE', *, *, #51968, .F. ) ;
#88267 = EDGE_CURVE ( 'NONE', #52090, #26199, #27466, .T. ) ;
#88266 = CARTESIAN_POINT ( 'NONE',  ( 12.90232279286373185, -3.316774720514426456, -28.14923833570356493 ) ) ;
#88268 = CARTESIAN_POINT ( 'NONE',  ( 7.003190781191628744, -19.75400906848480176, -1.500000000000002220 ) ) ;
#88269 = CARTESIAN_POINT ( 'NONE',  ( -17.52905966558703454, -13.16386835867055716, 11.49999999999999645 ) ) ;
#88270 = AXIS2_PLACEMENT_3D ( 'NONE', #16981, #46439, #69783 ) ;
#88271 = EDGE_CURVE ( 'NONE', #19622, #12687, #52948, .T. ) ;
#88272 = CARTESIAN_POINT ( 'NONE',  ( -26.71877946146332050, -24.89279912406997752, 7.184564487620880513 ) ) ;
#88273 = CARTESIAN_POINT ( 'NONE',  ( 5.095029512766671154, -3.302735871364486098, -27.56177443937556859 ) ) ;
#88274 = CARTESIAN_POINT ( 'NONE',  ( 20.52096793114426276, -9.243637136814692568, -1.500000000000002220 ) ) ;
#88275 = ADVANCED_FACE ( 'NONE', ( #90995 ), #12865, .T. ) ;
#88276 = CARTESIAN_POINT ( 'NONE',  ( -3.961239394588834895, 20.55660451852329018, -1.500000000000002220 ) ) ;
#88277 = CARTESIAN_POINT ( 'NONE',  ( -26.09636659181000695, -24.88148713818772961, 4.940287743360734396 ) ) ;
#88278 = CARTESIAN_POINT ( 'NONE',  ( -72.52287095715003318, -23.73934037231756022, 11.05740245334329153 ) ) ;
#88279 = CARTESIAN_POINT ( 'NONE',  ( -89.22287095715005023, -23.47593901973090169, -1.443836447538996870 ) ) ;
#88280 = ORIENTED_EDGE ( 'NONE', *, *, #79675, .T. ) ;
#88281 = ORIENTED_EDGE ( 'NONE', *, *, #38069, .T. ) ;
#88282 = ORIENTED_EDGE ( 'NONE', *, *, #37326, .F. ) ;
#88283 = CARTESIAN_POINT ( 'NONE',  ( 31.93426202889373400, -6.376774720514426953, 6.907000118922836940 ) ) ;
#88284 = ORIENTED_EDGE ( 'NONE', *, *, #52482, .T. ) ;
#88285 = CARTESIAN_POINT ( 'NONE',  ( 2.027878592902508270, 21.29203748114955985, -1.500000000000002220 ) ) ;
#88286 = EDGE_CURVE ( 'NONE', #80243, #68064, #21466, .T. ) ;
#88287 = ORIENTED_EDGE ( 'NONE', *, *, #41703, .T. ) ;
#88288 = CARTESIAN_POINT ( 'NONE',  ( -53.62287095715005592, -29.50248528299804818, 1.056150453629033370 ) ) ;
#88289 = CARTESIAN_POINT ( 'NONE',  ( -8.250207518706217158, 19.40231308534122689, 11.49999999999998934 ) ) ;
#88290 = LINE ( 'NONE', #18761, #56332 ) ;
#88291 = CARTESIAN_POINT ( 'NONE',  ( 3.632573734185411851, -6.376774720514429617, 21.82795992345630509 ) ) ;
#88292 = CARTESIAN_POINT ( 'NONE',  ( -43.62287095715003460, -23.47596703998600276, 11.44779298504227505 ) ) ;
#88293 = DIRECTION ( 'NONE',  ( -0.8264557562326033668, 6.845827386180409975E-16, -0.5630016722799281448 ) ) ;
#88294 = CARTESIAN_POINT ( 'NONE',  ( -110.2093792378192063, -25.30161501422653814, 5.585409209247975681 ) ) ;
#88295 = CARTESIAN_POINT ( 'NONE',  ( -19.13726171168348245, 10.91495894028074432, -1.500000000000002220 ) ) ;
#88296 = ORIENTED_EDGE ( 'NONE', *, *, #21336, .F. ) ;
#88297 = CARTESIAN_POINT ( 'NONE',  ( -65.54555213868854935, -24.40133493613049964, 9.663955038902802386 ) ) ;
#88298 = B_SPLINE_CURVE_WITH_KNOTS ( 'NONE', 3,
 ( #30999, #61966, #62978, #55358, #71079, #23369 ),
 .UNSPECIFIED., .F., .F.,
 ( 4, 2, 4 ),
 ( 1.570887131795109485E-05, 0.001396322306279764325, 0.002776935741241577573 ),
 .UNSPECIFIED. ) ;
#88299 = DIRECTION ( 'NONE',  ( -3.773278334453079030E-23, 0.9999999999976377785, 2.173523156925979128E-06 ) ) ;
#88300 = CARTESIAN_POINT ( 'NONE',  ( -78.62287095715009855, -23.96177878511308634, 10.65340807706329862 ) ) ;
#88301 = CARTESIAN_POINT ( 'NONE',  ( -28.39364267440558365, -25.14063740019444637, 3.798368663089754182 ) ) ;
#88302 = CARTESIAN_POINT ( 'NONE',  ( -84.52287095715007581, -23.48783264082477018, -1.443836473390090802 ) ) ;
#88303 = VECTOR ( 'NONE', #17561, 1000.000000000000114 ) ;
#88304 = CARTESIAN_POINT ( 'NONE',  ( -102.6228709571500559, -23.47593901973091235, -1.443836447539001089 ) ) ;
#88305 = CARTESIAN_POINT ( 'NONE',  ( 9.714863677370791706, 19.00186346016302608, 11.49999999999998934 ) ) ;
#88306 = CARTESIAN_POINT ( 'NONE',  ( -81.52287095715004739, -23.72747288104470087, -1.053458166803225904 ) ) ;
#88307 = LINE ( 'NONE', #19770, #31676 ) ;
#88308 = CARTESIAN_POINT ( 'NONE',  ( 21.57151214508649772, -0.8999999999999998002, -1.500000000000000666 ) ) ;
#88309 = PLANE ( 'NONE',  #13545 ) ;
#88310 = CARTESIAN_POINT ( 'NONE',  ( -22.20892344277460850, -4.061126821146308963, -1.500000000000002220 ) ) ;
#88311 = CARTESIAN_POINT ( 'NONE',  ( -123.5562042904833930, -24.64898659630529210, 1.056161002820830142 ) ) ;
#88312 = VERTEX_POINT ( 'NONE', #43833 ) ;
#88313 = FACE_OUTER_BOUND ( 'NONE', #43772, .T. ) ;
#88314 = CARTESIAN_POINT ( 'NONE',  ( -70.52287095715007581, -23.47593901973090524, -1.443836447538997092 ) ) ;
#88315 = CARTESIAN_POINT ( 'NONE',  ( 11.81298147481671279, -15.83112273922526470, 11.49999999999999645 ) ) ;
#88316 = DIRECTION ( 'NONE',  ( 0.000000000000000000, 0.9999999999976377785, 2.173523156925979975E-06 ) ) ;
#88317 = DIRECTION ( 'NONE',  ( -0.000000000000000000, -1.000000000000000000, -0.000000000000000000 ) ) ;
#88318 = ORIENTED_EDGE ( 'NONE', *, *, #47151, .F. ) ;
#88319 = DIRECTION ( 'NONE',  ( -0.000000000000000000, 1.000000000000000000, 0.000000000000000000 ) ) ;
#88320 = CARTESIAN_POINT ( 'NONE',  ( -29.77605907665351737, -24.60094425751508140, 4.091750246108072808 ) ) ;
#88321 = CARTESIAN_POINT ( 'NONE',  ( -61.52287095715006870, -23.96177878511308634, 10.65340807706330573 ) ) ;
#88322 = CARTESIAN_POINT ( 'NONE',  ( -16.60028029328060128, 13.79055755010687356, 11.49999999999998934 ) ) ;
#88323 = CARTESIAN_POINT ( 'NONE',  ( -71.58953762381672448, -23.47596703998600276, 11.44779298504227505 ) ) ;
#88324 = CARTESIAN_POINT ( 'NONE',  ( -2.899999999999996803, 31.80000000000000071, 0.000000000000000000 ) ) ;
#88325 = DIRECTION ( 'NONE',  ( -1.000000000000000000, -0.000000000000000000, -0.000000000000000000 ) ) ;
#88326 = CARTESIAN_POINT ( 'NONE',  ( -81.85706362847145101, -25.22784785830409149, 6.463371807680155179 ) ) ;
#88327 = EDGE_CURVE ( 'NONE', #12640, #92874, #27616, .T. ) ;
#88328 = CARTESIAN_POINT ( 'NONE',  ( -1.996473883165060581, 19.68112600131995293, -1.500000000000002220 ) ) ;
#88329 = VERTEX_POINT ( 'NONE', #89505 ) ;
#88330 = CARTESIAN_POINT ( 'NONE',  ( 11.01437679584920026, 17.03896688766576517, 11.49999999999999645 ) ) ;
#88331 = CARTESIAN_POINT ( 'NONE',  ( -7.586742644780859912, -5.876774720514413630, 19.78730719034165020 ) ) ;
#88332 = EDGE_CURVE ( 'NONE', #79545, #73404, #36222, .T. ) ;
#88333 = VECTOR ( 'NONE', #4989, 1000.000000000000114 ) ;
#88334 = ORIENTED_EDGE ( 'NONE', *, *, #35402, .F. ) ;
#88335 = CARTESIAN_POINT ( 'NONE',  ( -110.6228709571500559, -23.85196035786901803, -0.8779234886474867050 ) ) ;
#88336 = DIRECTION ( 'NONE',  ( 0.000000000000000000, -1.000000000000000000, 0.000000000000000000 ) ) ;
#88337 = DIRECTION ( 'NONE',  ( 0.000000000000000000, -1.000000000000000000, 0.000000000000000000 ) ) ;
#88338 = CARTESIAN_POINT ( 'NONE',  ( 12.53797248504841910, -0.3587747205144256601, -28.12591401903467059 ) ) ;
#88339 = CARTESIAN_POINT ( 'NONE',  ( 27.53860345374771867, 1.682774720514426114, -9.482392034746240483 ) ) ;
#88340 = CARTESIAN_POINT ( 'NONE',  ( -28.98875734969026041, 3.316774720514426456, -0.08597719988137648983 ) ) ;
#88341 = CARTESIAN_POINT ( 'NONE',  ( -10.14125802585430947, 17.27231531754821603, 11.49999999999998934 ) ) ;
#88342 = VECTOR ( 'NONE', #99234, 1000.000000000000000 ) ;
#88343 = FACE_OUTER_BOUND ( 'NONE', #26906, .T. ) ;
#88344 = EDGE_LOOP ( 'NONE', ( #40947, #34473, #57587, #37711 ) ) ;
#88345 = AXIS2_PLACEMENT_3D ( 'NONE', #48060, #63807, #94721 ) ;
#88346 = DIRECTION ( 'NONE',  ( -3.773278334453079030E-23, 0.9999999999976377785, 2.173523156925979128E-06 ) ) ;
#88347 = CARTESIAN_POINT ( 'NONE',  ( -35.58477060636910494, -24.63355581998387223, 0.9682620441943878831 ) ) ;
#88348 = CARTESIAN_POINT ( 'NONE',  ( -63.55620429048337883, -24.64965694238574301, 8.947790433994201820 ) ) ;
#88349 = CARTESIAN_POINT ( 'NONE',  ( -105.5228709571500758, -24.91544648472621759, 1.928969306349233914 ) ) ;
#88350 = CARTESIAN_POINT ( 'NONE',  ( -103.5228709571501184, -24.34917612406837151, 0.1852690917426557671 ) ) ;
#88351 = CARTESIAN_POINT ( 'NONE',  ( 15.88393883468562606, 3.596971506840126676, -28.01277999924193551 ) ) ;
#88352 = CARTESIAN_POINT ( 'NONE',  ( -98.87424918762685877, -25.30060005375480969, 6.009289253917325269 ) ) ;
#88353 = VERTEX_POINT ( 'NONE', #98100 ) ;
#88354 = CARTESIAN_POINT ( 'NONE',  ( 0.8761431260907562857, 20.31601184897261092, -1.500000000000002220 ) ) ;
#88355 = B_SPLINE_CURVE_WITH_KNOTS ( 'NONE', 3,
 ( #99249, #84527, #91142, #52587, #45981, #76898 ),
 .UNSPECIFIED., .F., .F.,
 ( 4, 2, 4 ),
 ( 6.384118696481608166E-06, 0.001386860460837311196, 0.002767336802978141025 ),
 .UNSPECIFIED. ) ;
#88356 = ORIENTED_EDGE ( 'NONE', *, *, #17465, .F. ) ;
#88357 = CARTESIAN_POINT ( 'NONE',  ( -8.048360580058307789, -21.46040670285860230, 11.49999999999998934 ) ) ;
#88358 = CARTESIAN_POINT ( 'NONE',  ( 29.59866736649642860, 4.678593451839772044, 28.90589631152484174 ) ) ;
#88359 = CARTESIAN_POINT ( 'NONE',  ( -127.5900868930851004, -23.96169478059713853, 10.65365249895716637 ) ) ;
#88360 = ORIENTED_EDGE ( 'NONE', *, *, #14540, .F. ) ;
#88361 = PLANE ( 'NONE',  #29804 ) ;
#88362 = CARTESIAN_POINT ( 'NONE',  ( -49.35312698006249832, -25.26264048826114816, 6.504948644732236218 ) ) ;
#88363 = CARTESIAN_POINT ( 'NONE',  ( -86.58953762381671027, -23.47593901973091235, -1.443836447539002865 ) ) ;
#88364 = CARTESIAN_POINT ( 'NONE',  ( 20.46717832272283033, -5.532298862796615424, 11.49999999999999645 ) ) ;
#88365 = VECTOR ( 'NONE', #83204, 1000.000000000000114 ) ;
#88366 = CARTESIAN_POINT ( 'NONE',  ( -20.57447749561850969, 8.151157241358404804, -1.500000000000002220 ) ) ;
#88367 = CARTESIAN_POINT ( 'NONE',  ( 14.30100545221680441, -14.83292283143518375, 11.49999999999998934 ) ) ;
#88368 = VERTEX_POINT ( 'NONE', #28605 ) ;
#88369 = CARTESIAN_POINT ( 'NONE',  ( -41.52885629564732284, -24.65952944569304606, 1.056160979905696351 ) ) ;
#88370 = ORIENTED_EDGE ( 'NONE', *, *, #89079, .T. ) ;
#88371 = CARTESIAN_POINT ( 'NONE',  ( 7.041152093163508319, -6.376774720514424288, 21.17127001373575368 ) ) ;
#88372 = FACE_OUTER_BOUND ( 'NONE', #68613, .T. ) ;
#88373 = ORIENTED_EDGE ( 'NONE', *, *, #29330, .F. ) ;
#88375 = ORIENTED_EDGE ( 'NONE', *, *, #45302, .F. ) ;
#88374 = EDGE_CURVE ( 'NONE', #76871, #91107, #2498, .T. ) ;
#88376 = VERTEX_POINT ( 'NONE', #75268 ) ;
#88377 = CARTESIAN_POINT ( 'NONE',  ( -111.7814946224345789, -25.29712067403330877, 4.332404411321261861 ) ) ;
#88378 = CARTESIAN_POINT ( 'NONE',  ( -28.47997080486860710, -24.34985781594834364, 9.386484685950517104 ) ) ;
#88379 = DIRECTION ( 'NONE',  ( -3.773278334453079030E-23, 0.9999999999976377785, 2.173523156925979128E-06 ) ) ;
#88380 = CARTESIAN_POINT ( 'NONE',  ( -6.500255983836059848, -19.66680810221124887, -1.500000000000002220 ) ) ;
#88381 = CARTESIAN_POINT ( 'NONE',  ( 19.26462925850498920, -9.998780574493274287, 11.49999999999999645 ) ) ;
#88382 = ORIENTED_EDGE ( 'NONE', *, *, #14028, .F. ) ;
#88383 = ADVANCED_FACE ( 'NONE', ( #6753 ), #4772, .T. ) ;
#88384 = CARTESIAN_POINT ( 'NONE',  ( -98.89485989515169706, -25.26150877536736772, 6.039289736180342594 ) ) ;
#88385 = CARTESIAN_POINT ( 'NONE',  ( -111.7693513301115900, -25.27516155285008992, 4.137661877063939286 ) ) ;
#88386 = CARTESIAN_POINT ( 'NONE',  ( -16.61153998044026991, -15.06042057022924929, -1.500000000000002220 ) ) ;
#88387 = EDGE_CURVE ( 'NONE', #44858, #50853, #35726, .T. ) ;
#88388 = CARTESIAN_POINT ( 'NONE',  ( -29.49875734969025842, -0.3587747205144265483, 25.61802280011862720 ) ) ;
#88389 = DIRECTION ( 'NONE',  ( 0.9913618264504693300, -5.365801633547217234E-16, -0.1311553622875920033 ) ) ;
#88390 = ORIENTED_EDGE ( 'NONE', *, *, #28408, .F. ) ;
#88391 = CARTESIAN_POINT ( 'NONE',  ( 27.53860345374771867, 4.132774720517318201, -9.482392034746240483 ) ) ;
#88392 = PLANE ( 'NONE',  #37781 ) ;
#88393 = EDGE_CURVE ( 'NONE', #51301, #58944, #60545, .T. ) ;
#88394 = VERTEX_POINT ( 'NONE', #36718 ) ;
#88395 = EDGE_CURVE ( 'NONE', #89454, #16487, #98603, .T. ) ;
#88396 = ORIENTED_EDGE ( 'NONE', *, *, #72578, .T. ) ;
#88397 = B_SPLINE_CURVE_WITH_KNOTS ( 'NONE', 3,
 ( #21775, #39017, #77566, #52749 ),
 .UNSPECIFIED., .F., .F.,
 ( 4, 4 ),
 ( 0.000000000000000000, 0.0001000000000000028644 ),
 .UNSPECIFIED. ) ;
#88398 = VECTOR ( 'NONE', #4343, 1000.000000000000000 ) ;
#88399 = CARTESIAN_POINT ( 'NONE',  ( -103.6228709571500985, -23.94994826722517089, -0.6494450866351687557 ) ) ;
#88400 = ORIENTED_EDGE ( 'NONE', *, *, #65875, .F. ) ;
#88401 = AXIS2_PLACEMENT_3D ( 'NONE', #37440, #38433, #45560 ) ;
#88402 = CARTESIAN_POINT ( 'NONE',  ( 6.411417644607832145, 20.24884965431308714, -1.500000000000002220 ) ) ;
#88403 = EDGE_LOOP ( 'NONE', ( #10685, #52304, #99958, #95389 ) ) ;
#88404 = CARTESIAN_POINT ( 'NONE',  ( -68.62287095715005592, -23.48783264082478439, -1.443836473390067265 ) ) ;
#88405 = CARTESIAN_POINT ( 'NONE',  ( 19.17057494584436839, 10.47865234463220396, -1.500000000000002220 ) ) ;
#88406 = CARTESIAN_POINT ( 'NONE',  ( -52.51445879613589796, -23.73791477778911840, 11.05961554403171476 ) ) ;
#88407 = CARTESIAN_POINT ( 'NONE',  ( -40.75388878839229534, -25.18430879041033421, 3.329423250322895100 ) ) ;
#88408 = VECTOR ( 'NONE', #83169, 1000.000000000000000 ) ;
#88409 = CARTESIAN_POINT ( 'NONE',  ( -44.52287095715006160, -29.50248528299804818, 1.056150453629031594 ) ) ;
#88410 = CARTESIAN_POINT ( 'NONE',  ( 21.88901064076550185, 0.7357440816682787599, -1.500000000000002220 ) ) ;
#88411 = CARTESIAN_POINT ( 'NONE',  ( 1.305682803664691249, 0.3587747205144265483, 29.57950906855421991 ) ) ;
#88412 = EDGE_LOOP ( 'NONE', ( #54560, #17524, #54676, #90599 ) ) ;
#88413 = EDGE_CURVE ( 'NONE', #14381, #53590, #78660, .T. ) ;
#88414 = CARTESIAN_POINT ( 'NONE',  ( -69.62287095715005592, -23.73907113216991149, -1.053371485793230811 ) ) ;
#88415 = CARTESIAN_POINT ( 'NONE',  ( -121.5562042904833504, -23.47593901973091235, -1.443836447538997536 ) ) ;
#88416 = AXIS2_PLACEMENT_3D ( 'NONE', #36857, #38342, #52084 ) ;
#88417 = AXIS2_PLACEMENT_3D ( 'NONE', #88464, #18939, #34677 ) ;
#88418 = ORIENTED_EDGE ( 'NONE', *, *, #55746, .T. ) ;
#88419 = CARTESIAN_POINT ( 'NONE',  ( -32.52287095715006160, -24.64965694238575011, 8.947790433994207149 ) ) ;
#88420 = ORIENTED_EDGE ( 'NONE', *, *, #80597, .F. ) ;
#88421 = LINE ( 'NONE', #11785, #88091 ) ;
#88422 = CARTESIAN_POINT ( 'NONE',  ( -10.22956868858724100, -23.25619435864494378, 1.633150109380534509 ) ) ;
#88423 = CARTESIAN_POINT ( 'NONE',  ( 17.84191302092929021, 11.53353326677314961, -1.500000000000002220 ) ) ;
#88424 = DIRECTION ( 'NONE',  ( -3.773278334444167608E-23, 1.000000000000000000, 0.000000000000000000 ) ) ;
#88425 = DIRECTION ( 'NONE',  ( 1.000000000000000000, -7.960204194457801640E-17, -0.000000000000000000 ) ) ;
#88426 = DIRECTION ( 'NONE',  ( 2.000709955812756815E-15, 0.000000000000000000, 1.000000000000000000 ) ) ;
#88427 = CARTESIAN_POINT ( 'NONE',  ( -68.62715718384154684, -24.51314013834315375, 0.6176544820404133995 ) ) ;
#88428 = CARTESIAN_POINT ( 'NONE',  ( -5.694372300836820777, 18.57635362771370424, -1.500000000000002220 ) ) ;
#88429 = CARTESIAN_POINT ( 'NONE',  ( -30.47287095715007510, -23.47593906522708451, -1.422904450652597852 ) ) ;
#88430 = VERTEX_POINT ( 'NONE', #68667 ) ;
#88431 = CARTESIAN_POINT ( 'NONE',  ( 19.03533760385612439, 4.641190475545474037, 11.49999999999999645 ) ) ;
#88432 = CARTESIAN_POINT ( 'NONE',  ( -0.02075734969026423599, 6.376774720514426953, -0.08597719988137648983 ) ) ;
#88433 = DIRECTION ( 'NONE',  ( 0.000000000000000000, -2.173523156925980399E-06, 0.9999999999976378895 ) ) ;
#88434 = ADVANCED_FACE ( 'NONE', ( #62558 ), #30396, .T. ) ;
#88435 = ORIENTED_EDGE ( 'NONE', *, *, #39819, .F. ) ;
#88436 = CARTESIAN_POINT ( 'NONE',  ( 4.038745349937860496, -6.376774720514429617, 21.81354843764681206 ) ) ;
#88437 = CARTESIAN_POINT ( 'NONE',  ( -89.56218751811385914, -23.48783264082478084, -1.443836473390068598 ) ) ;
#88438 = B_SPLINE_CURVE_WITH_KNOTS ( 'NONE', 3,
 ( #17320, #93432, #85833, #71621, #73991, #39654, #58276, #24429, #27313, #16317 ),
 .UNSPECIFIED., .F., .F.,
 ( 4, 2, 2, 2, 4 ),
 ( 1.734723475976807094E-18, 0.001417051740733931559, 0.002125577611100896037, 0.002479840546284378926, 0.002834103481467860949 ),
 .UNSPECIFIED. ) ;
#88439 = CARTESIAN_POINT ( 'NONE',  ( -83.52287095715006160, -24.65952944569304606, 1.056160979905698794 ) ) ;
#88440 = ADVANCED_FACE ( 'NONE', ( #31087 ), #84877, .T. ) ;
#88441 = CARTESIAN_POINT ( 'NONE',  ( -81.13115756185166560, -25.24813961791220862, 7.427330389041354231 ) ) ;
#88442 = CARTESIAN_POINT ( 'NONE',  ( 18.28535361393070957, 7.309334553982634652, 11.49999999999998934 ) ) ;
#88443 = VERTEX_POINT ( 'NONE', #76746 ) ;
#88444 = VECTOR ( 'NONE', #76216, 1000.000000000000000 ) ;
#88445 = CARTESIAN_POINT ( 'NONE',  ( -88.52287095715006160, -29.50250243563736774, 8.947779886222139822 ) ) ;
#88446 = CARTESIAN_POINT ( 'NONE',  ( 30.61004588589006659, -4.070814610512477394, 27.12580813198458785 ) ) ;
#88447 = DATE_TIME_ROLE ( 'classification_date' ) ;
#88448 = EDGE_CURVE ( 'NONE', #13615, #78754, #29071, .T. ) ;
#88449 = ORIENTED_EDGE ( 'NONE', *, *, #58171, .F. ) ;
#88450 = PLANE ( 'NONE',  #74245 ) ;
#88451 = CARTESIAN_POINT ( 'NONE',  ( -105.6228709571500133, -24.91570333823100469, 8.075032458375549282 ) ) ;
#88452 = CARTESIAN_POINT ( 'NONE',  ( -47.61501443379227538, -23.48783264082478084, -1.443836473390071928 ) ) ;
#88453 = CARTESIAN_POINT ( 'NONE',  ( -105.6228709571500701, -24.15516710230295772, 10.28746687063725496 ) ) ;
#88454 = CARTESIAN_POINT ( 'NONE',  ( -78.92465937840067625, -25.31249729222309242, 5.276660411446114196 ) ) ;
#88455 = CARTESIAN_POINT ( 'NONE',  ( 31.79364159983995464, -1.682774720514426114, -11.59305536555894278 ) ) ;
#88456 = PLANE ( 'NONE',  #76972 ) ;
#88457 = CARTESIAN_POINT ( 'NONE',  ( -2.986242917674419850, -19.73498743542299749, -1.500000000000002220 ) ) ;
#88458 = EDGE_CURVE ( 'NONE', #97387, #89410, #93236, .T. ) ;
#88459 = CARTESIAN_POINT ( 'NONE',  ( -101.0634058648739426, -25.22418476227237960, 3.513563706143655541 ) ) ;
#88460 = CARTESIAN_POINT ( 'NONE',  ( 7.211006999188390942, 18.53272205163514030, -1.500000000000002220 ) ) ;
#88461 = ORIENTED_EDGE ( 'NONE', *, *, #56177, .T. ) ;
#88462 = CARTESIAN_POINT ( 'NONE',  ( -91.15361000704896810, -25.27880950044357178, 5.947789066507965572 ) ) ;
#88463 = CARTESIAN_POINT ( 'NONE',  ( -51.35995362507909334, -25.19762389802447089, 6.693417099905952128 ) ) ;
#88464 = CARTESIAN_POINT ( 'NONE',  ( 8.160000000000000142, -9.123836073446797812, -2.666350264951732552 ) ) ;
#88465 = CARTESIAN_POINT ( 'NONE',  ( 13.25751441563444999, -6.376774720514426065, -25.10777837594209672 ) ) ;
#88466 = CARTESIAN_POINT ( 'NONE',  ( -17.75621389795859884, -10.86975384844714831, 11.49999999999999645 ) ) ;
#88467 = DIRECTION ( 'NONE',  ( 0.7071067811865507924, 0.000000000000000000, 0.7071067811865442421 ) ) ;
#88468 = APPROVAL ( #49899, 'UNSPECIFIED' ) ;
#88469 = DIRECTION ( 'NONE',  ( 0.000000000000000000, 0.000000000000000000, -1.000000000000000000 ) ) ;
#88470 = CARTESIAN_POINT ( 'NONE',  ( -7.631545101075025705, 21.52643039700453897, 11.49999999999999645 ) ) ;
#88471 = AXIS2_PLACEMENT_3D ( 'NONE', #59159, #74859, #5363 ) ;
#88472 = VERTEX_POINT ( 'NONE', #96001 ) ;
#88473 = CARTESIAN_POINT ( 'NONE',  ( 0.7051282051282083962, -6.376774720514427841, 21.75000000000000000 ) ) ;
#88475 = AXIS2_PLACEMENT_3D ( 'NONE', #77155, #93384, #30991 ) ;
#88474 = CARTESIAN_POINT ( 'NONE',  ( -89.55620429048339304, -23.47596703998600631, 11.44779298504227683 ) ) ;
#88476 = EDGE_LOOP ( 'NONE', ( #71538, #27951, #88789, #76605, #34617, #68179, #48968, #7251, #4125, #62819, #90114 ) ) ;
#88477 = VECTOR ( 'NONE', #6054, 1000.000000000000000 ) ;
#88478 = CARTESIAN_POINT ( 'NONE',  ( 8.147030896810244727, 18.52525024547675869, 11.49999999999998934 ) ) ;
#88479 = CARTESIAN_POINT ( 'NONE',  ( -49.27764846858840997, -25.25176233969420636, 6.145204990682164414 ) ) ;
#88480 = VECTOR ( 'NONE', #22257, 1000.000000000000000 ) ;
#88481 = DIRECTION ( 'NONE',  ( -0.000000000000000000, 1.000000000000000000, -0.000000000000000000 ) ) ;
#88482 = VECTOR ( 'NONE', #43547, 1000.000000000000114 ) ;
#88483 = CARTESIAN_POINT ( 'NONE',  ( 32.66876533700882845, 5.965225279485572685, -12.58926540598385557 ) ) ;
#88484 = VERTEX_POINT ( 'NONE', #48336 ) ;
#88485 = CARTESIAN_POINT ( 'NONE',  ( -79.39652874673353722, -25.30017758679730022, 5.617944653114273379 ) ) ;
#88486 = CARTESIAN_POINT ( 'NONE',  ( -10.17728017005432228, 5.183720752832764234, 29.88674535377839803 ) ) ;
#88487 = CARTESIAN_POINT ( 'NONE',  ( -13.93161493328335432, -14.37010051631055418, -1.500000000000002220 ) ) ;
#88488 = CARTESIAN_POINT ( 'NONE',  ( 2.700122536338566359, 20.86363338933649558, 11.49999999999999645 ) ) ;
#88489 = PLANE ( 'NONE',  #10 ) ;
#88490 = FACE_OUTER_BOUND ( 'NONE', #72158, .T. ) ;
#88491 = CARTESIAN_POINT ( 'NONE',  ( 16.78392297789021015, 14.29496084597832883, 11.49999999999998934 ) ) ;
#88492 = CARTESIAN_POINT ( 'NONE',  ( -39.65036112522632550, -25.27806035532287154, 4.754946624924129672 ) ) ;
#88493 = DIRECTION ( 'NONE',  ( 0.000000000000000000, -2.173523156925980399E-06, 0.9999999999976378895 ) ) ;
#88494 = CARTESIAN_POINT ( 'NONE',  ( -50.02027282914984596, -25.18440113274999703, 3.346181424171986496 ) ) ;
#88495 = CARTESIAN_POINT ( 'NONE',  ( -72.58426024455503978, -24.51314013834316796, 0.6176544820404145097 ) ) ;
#88496 = CARTESIAN_POINT ( 'NONE',  ( -31.57477479285322630, -24.65952944569304250, 1.056160979905695463 ) ) ;
#88497 = ORIENTED_EDGE ( 'NONE', *, *, #46349, .F. ) ;
#88498 = ORIENTED_EDGE ( 'NONE', *, *, #99358, .F. ) ;
#88499 = EDGE_CURVE ( 'NONE', #65316, #76238, #57958, .T. ) ;
#88500 = DIRECTION ( 'NONE',  ( 0.000000000000000000, 0.000000000000000000, 1.000000000000000000 ) ) ;
#88501 = CARTESIAN_POINT ( 'NONE',  ( -101.1026865405329147, -25.27404666790166132, 2.999872496792844512 ) ) ;
#88502 = CARTESIAN_POINT ( 'NONE',  ( -4.968349358974360364, -6.376774720514411854, 19.46153846153846700 ) ) ;
#88503 = CARTESIAN_POINT ( 'NONE',  ( -2.888065500968368227, -20.30684875360264741, -1.500000000000002220 ) ) ;
#88504 = ORIENTED_EDGE ( 'NONE', *, *, #56229, .F. ) ;
#88505 = DIRECTION ( 'NONE',  ( -2.338552693767719605E-15, 0.000000000000000000, 1.000000000000000000 ) ) ;
#88506 = CARTESIAN_POINT ( 'NONE',  ( -10.21384395349174490, 3.316774720514427344, 29.49402280011862487 ) ) ;
#88507 = AXIS2_PLACEMENT_3D ( 'NONE', #29402, #67985, #53759 ) ;
#88508 = DIRECTION ( 'NONE',  ( -3.773278334453079618E-23, 0.9999999999976377785, 2.173523156925979975E-06 ) ) ;
#88509 = CARTESIAN_POINT ( 'NONE',  ( -21.99995728619510516, 3.820703864638951952, -1.500000000000002220 ) ) ;
#88510 = CARTESIAN_POINT ( 'NONE',  ( 29.70906083364843653, -4.222256839740661682, 27.99786980188468277 ) ) ;
#88511 = FACE_OUTER_BOUND ( 'NONE', #21472, .T. ) ;
#88512 = ORIENTED_EDGE ( 'NONE', *, *, #42476, .T. ) ;
#88513 = CARTESIAN_POINT ( 'NONE',  ( -24.90875734969025501, -5.965225279485572685, 30.51402280011862089 ) ) ;
#88514 = CARTESIAN_POINT ( 'NONE',  ( 3.249631081431332280, -5.876774720514423400, 21.24682042713427776 ) ) ;
#88515 = EDGE_CURVE ( 'NONE', #5644, #50554, #56957, .T. ) ;
#88516 = CARTESIAN_POINT ( 'NONE',  ( 18.01467621842780176, -10.50282939286117667, -1.500000000000002220 ) ) ;
#88517 = EDGE_CURVE ( 'NONE', #85275, #68532, #7966, .T. ) ;
#88518 = VERTEX_POINT ( 'NONE', #80782 ) ;
#88520 = ORIENTED_EDGE ( 'NONE', *, *, #11217, .F. ) ;
#88519 = CARTESIAN_POINT ( 'NONE',  ( -0.02075734969026423599, 6.475225279485573360, -28.03397719988137382 ) ) ;
#88521 = VERTEX_POINT ( 'NONE', #41732 ) ;
#88522 = CARTESIAN_POINT ( 'NONE',  ( -104.5228709571500758, -23.47593901973090524, -1.443836447538996204 ) ) ;
#88523 = CARTESIAN_POINT ( 'NONE',  ( -14.90395405082875335, 14.90835605916499418, -1.500000000000002220 ) ) ;
#88524 = ORIENTED_EDGE ( 'NONE', *, *, #50704, .T. ) ;
#88525 = CARTESIAN_POINT ( 'NONE',  ( -114.6228709571500701, -24.50321055353806798, 9.387540953477525818 ) ) ;
#88526 = CARTESIAN_POINT ( 'NONE',  ( -98.62287095715005592, -23.48783264082478439, -1.443836473390061936 ) ) ;
#88527 = FACE_OUTER_BOUND ( 'NONE', #49579, .T. ) ;
#88528 = CARTESIAN_POINT ( 'NONE',  ( -101.8751956322788317, -25.03152227061655211, 6.541290337622787554 ) ) ;
#88529 = CARTESIAN_POINT ( 'NONE',  ( -129.6228709571500985, -24.50321055353806443, 9.387540953477522265 ) ) ;
#88530 = CARTESIAN_POINT ( 'NONE',  ( -12.04083774165243881, -18.01462592983040523, -1.500000000000002220 ) ) ;
#88531 = CARTESIAN_POINT ( 'NONE',  ( -63.52287095715003318, -23.96177878511308990, 10.65340807706330217 ) ) ;
#88533 = ORIENTED_EDGE ( 'NONE', *, *, #44741, .T. ) ;
#88532 = CARTESIAN_POINT ( 'NONE',  ( -21.75032768068154354, -4.810781854073628239, 11.49999999999999645 ) ) ;
#88534 = EDGE_CURVE ( 'NONE', #100208, #99331, #52099, .T. ) ;
#88535 = CARTESIAN_POINT ( 'NONE',  ( -51.34258402508250185, -25.31441820025300871, 5.647562909900377903 ) ) ;
#88536 = CARTESIAN_POINT ( 'NONE',  ( -11.64875734969026233, -0.3587747205144265483, 31.02402280011862246 ) ) ;
#88537 = CARTESIAN_POINT ( 'NONE',  ( 4.762431091568566366, -6.376774720514422512, 21.19858511215680608 ) ) ;
#88538 = ORIENTED_EDGE ( 'NONE', *, *, #63019, .T. ) ;
#88539 = VECTOR ( 'NONE', #15178, 1000.000000000000114 ) ;
#88541 = ORIENTED_EDGE ( 'NONE', *, *, #81264, .F. ) ;
#88540 = CARTESIAN_POINT ( 'NONE',  ( -54.22287095715005023, -23.47593901973090169, -1.443836447538997758 ) ) ;
#88542 = B_SPLINE_CURVE_WITH_KNOTS ( 'NONE', 3,
 ( #69703, #76783, #681, #92028, #53494, #61606, #62099, #15898, #30627, #15396, #31627, #77289, #85923, #16396 ),
 .UNSPECIFIED., .F., .F.,
 ( 4, 2, 2, 2, 2, 2, 4 ),
 ( 1.411962612463446054E-17, 0.0001878395792908931427, 0.0003756791585817721366, 0.0007513583171634909304, 0.001127037475745209941, 0.001314877055036069338, 0.001502716634326928735 ),
 .UNSPECIFIED. ) ;
#88543 = VERTEX_POINT ( 'NONE', #49344 ) ;
#88544 = CARTESIAN_POINT ( 'NONE',  ( 31.21773176006472283, -5.300046855345732943, 2.139914057118826651 ) ) ;
#88545 = CARTESIAN_POINT ( 'NONE',  ( -49.97401002309579354, -25.30055537004108857, 4.651112704816034338 ) ) ;
#88546 = VECTOR ( 'NONE', #23905, 1000.000000000000000 ) ;
#88547 = CARTESIAN_POINT ( 'NONE',  ( 13.91401389203221406, 5.965225279485572685, 28.26920385068457264 ) ) ;
#88548 = CARTESIAN_POINT ( 'NONE',  ( -105.5228709571501042, -24.52232992886361984, 0.6492154411906025935 ) ) ;
#88549 = VERTEX_POINT ( 'NONE', #18871 ) ;
#88550 = VECTOR ( 'NONE', #34963, 1000.000000000000000 ) ;
#88551 = CARTESIAN_POINT ( 'NONE',  ( -130.5728709571500303, -24.34523335840901126, -0.02865858326839056461 ) ) ;
#88552 = CARTESIAN_POINT ( 'NONE',  ( -14.39434090420295220, 17.20869321163716492, -1.500000000000002220 ) ) ;
#88553 = CIRCLE ( 'NONE', #43210, 2.899999999999999911 ) ;
#88554 = ORIENTED_EDGE ( 'NONE', *, *, #97665, .F. ) ;
#88555 = LINE ( 'NONE', #18531, #64440 ) ;
#88556 = DIRECTION ( 'NONE',  ( 0.000000000000000000, -0.9999999999976377785, -2.173523156925979975E-06 ) ) ;
#88557 = CARTESIAN_POINT ( 'NONE',  ( 11.32388168880214074, 5.356774720514423827, -25.00917421515942962 ) ) ;
#88558 = CARTESIAN_POINT ( 'NONE',  ( -4.495793269230770939, -5.876774720514410077, 19.27714342948718595 ) ) ;
#88559 = VECTOR ( 'NONE', #91686, 1000.000000000000000 ) ;
#88560 = CARTESIAN_POINT ( 'NONE',  ( -97.24175277348885515, -25.14064729901805606, 2.712351064733618422 ) ) ;
#88561 = ADVANCED_FACE ( 'NONE', ( #9759 ), #50334, .F. ) ;
#88562 = CARTESIAN_POINT ( 'NONE',  ( 8.161054176536994831, -17.82452852192863091, 11.49999999999998934 ) ) ;
#88563 = PLANE ( 'NONE',  #466 ) ;
#88564 = EDGE_LOOP ( 'NONE', ( #91769, #13407, #9299, #33710 ) ) ;
#88565 = CARTESIAN_POINT ( 'NONE',  ( -19.93307770644097232, -8.117153041090405807, -1.500000000000002220 ) ) ;
#88566 = CARTESIAN_POINT ( 'NONE',  ( 3.300000000000004263, 0.000000000000000000, 18.35000000000000142 ) ) ;
#88567 = CARTESIAN_POINT ( 'NONE',  ( -70.86754458488196917, -25.12219113017391336, 6.955654535003185757 ) ) ;
#88568 = CARTESIAN_POINT ( 'NONE',  ( -101.4426914514699121, -25.19143170071711779, 3.265421627976601293 ) ) ;
#88569 = CARTESIAN_POINT ( 'NONE',  ( -121.6228709571500275, -24.66019654487200441, 8.947790411086119278 ) ) ;
#88570 = CARTESIAN_POINT ( 'NONE',  ( 18.48385363477634513, -13.70420857335572506, -1.500000000000002220 ) ) ;
#88571 = EDGE_CURVE ( 'NONE', #45940, #17901, #68979, .T. ) ;
#88572 = ADVANCED_FACE ( 'NONE', ( #72175 ), #37160, .T. ) ;
#88573 = CALENDAR_DATE ( 2026, 9, 10 ) ;
#88574 = DIRECTION ( 'NONE',  ( 0.000000000000000000, 0.000000000000000000, -1.000000000000000000 ) ) ;
#88575 = FACE_OUTER_BOUND ( 'NONE', #52080, .T. ) ;
#88576 = CARTESIAN_POINT ( 'NONE',  ( 14.11618873683251252, 14.29484301466228047, 11.49999999999999645 ) ) ;
#88577 = DIRECTION ( 'NONE',  ( 0.000000000000000000, 1.000000000000000000, 0.000000000000000000 ) ) ;
#88578 = DIRECTION ( 'NONE',  ( -0.000000000000000000, 1.000000000000000000, -0.000000000000000000 ) ) ;
#88580 = B_SPLINE_CURVE_WITH_KNOTS ( 'NONE', 3,
 ( #53898, #76700, #23412, #7202, #38151 ),
 .UNSPECIFIED., .F., .F.,
 ( 4, 1, 4 ),
 ( 0.07540175290935291486, 0.07668996298668992462, 0.07797817306402693438 ),
 .UNSPECIFIED. ) ;
#88579 = DIRECTION ( 'NONE',  ( -0.9890158633619160478, -0.1478094111296162083, 0.000000000000000000 ) ) ;
#88581 = CARTESIAN_POINT ( 'NONE',  ( 13.02968616431334681, 5.152774720514426754, -26.31186222701397526 ) ) ;
#88582 = CARTESIAN_POINT ( 'NONE',  ( -82.52287095715006160, -24.64965694238407323, 8.947790433994198267 ) ) ;
#88583 = CARTESIAN_POINT ( 'NONE',  ( -18.79335158860655142, 6.462138572525057967, -1.500000000000002220 ) ) ;
#88584 = DIRECTION ( 'NONE',  ( 1.000000000000000000, 1.224646799147353207E-16, 0.000000000000000000 ) ) ;
#88585 = CARTESIAN_POINT ( 'NONE',  ( 19.47230031930329730, 2.946587627359682493, -1.500000000000002220 ) ) ;
#88586 = AXIS2_PLACEMENT_3D ( 'NONE', #52567, #6387, #60689 ) ;
#88587 = CARTESIAN_POINT ( 'NONE',  ( -60.62287095715004881, -23.48783264082478439, -1.443836473390068820 ) ) ;
#88588 = APPROVAL_STATUS ( 'not_yet_approved' ) ;
#88589 = CARTESIAN_POINT ( 'NONE',  ( -34.62287095715005592, -29.50248528299804818, 1.056150453629029817 ) ) ;
#88590 = CARTESIAN_POINT ( 'NONE',  ( 3.749014282529493869, -6.376774720514404748, 18.52125941707705792 ) ) ;
#88591 = CARTESIAN_POINT ( 'NONE',  ( 13.18972694569024640, 15.87703813876158598, 11.49999999999999645 ) ) ;
#88592 = VECTOR ( 'NONE', #95410, 1000.000000000000114 ) ;
#88593 = B_SPLINE_CURVE_WITH_KNOTS ( 'NONE', 3,
 ( #84544, #100245, #16026, #30760, #46000, #76919 ),
 .UNSPECIFIED., .F., .F.,
 ( 4, 2, 4 ),
 ( 6.391158118961561766E-06, 0.001387004593080780291, 0.002767618028042598960 ),
 .UNSPECIFIED. ) ;
#88594 = EDGE_CURVE ( 'NONE', #3153, #25992, #73172, .T. ) ;
#88595 = CARTESIAN_POINT ( 'NONE',  ( -120.5163177514428128, -25.00158670708911046, 2.256160236439219702 ) ) ;
#88596 = CARTESIAN_POINT ( 'NONE',  ( -18.33335541821337245, -13.34141728429830742, 11.49999999999999645 ) ) ;
#88597 = ORIENTED_EDGE ( 'NONE', *, *, #70924, .F. ) ;
#88598 = CARTESIAN_POINT ( 'NONE',  ( -53.52287095715006870, -24.65952944569304606, 1.056160979905693686 ) ) ;
#88599 = CARTESIAN_POINT ( 'NONE',  ( -97.62543170153185201, -24.51314013834315730, 0.6176544820404147318 ) ) ;
#88600 = CARTESIAN_POINT ( 'NONE',  ( -27.26363273317966573, -24.93063624427344038, 8.203482558825996307 ) ) ;
#88601 = CARTESIAN_POINT ( 'NONE',  ( -2.373828433815573735, -6.376774720514410077, 19.48240003225459915 ) ) ;
#88602 = EDGE_CURVE ( 'NONE', #94221, #27358, #84787, .T. ) ;
#88603 = AXIS2_PLACEMENT_3D ( 'NONE', #15793, #28658, #85816 ) ;
#88604 = ORIENTED_EDGE ( 'NONE', *, *, #66082, .F. ) ;
#88605 = CARTESIAN_POINT ( 'NONE',  ( -4.968349358974361252, -5.876774720514412742, 19.46153846153847056 ) ) ;
#88606 = CARTESIAN_POINT ( 'NONE',  ( 4.459850365305920938, 22.40387240153798487, -1.500000000000002220 ) ) ;
#88607 = DIRECTION ( 'NONE',  ( -3.773278334444167608E-23, 1.000000000000000000, 0.000000000000000000 ) ) ;
#88608 = CARTESIAN_POINT ( 'NONE',  ( -29.52287095715006160, -29.50248528299834305, 1.056150588822498460 ) ) ;
#88610 = ADVANCED_FACE ( 'NONE', ( #24977 ), #55951, .F. ) ;
#88609 = CARTESIAN_POINT ( 'NONE',  ( -82.64546651821306966, -23.48786465467241058, 11.44779295918254647 ) ) ;
#88611 = CARTESIAN_POINT ( 'NONE',  ( -22.07377061809603092, 4.253497373390751513, 11.49999999999999645 ) ) ;
#88612 = ORIENTED_EDGE ( 'NONE', *, *, #90005, .T. ) ;
#88613 = CARTESIAN_POINT ( 'NONE',  ( -33.62287095715005592, -23.48786465467240347, 11.44779295918255535 ) ) ;
#88614 = CARTESIAN_POINT ( 'NONE',  ( -15.43752342082821905, -15.63289427301443801, -1.500000000000002220 ) ) ;
#88615 = AXIS2_PLACEMENT_3D ( 'NONE', #6859, #1258, #53552 ) ;
#88616 = CYLINDRICAL_SURFACE ( 'NONE', #77077, 2.249999999999998668 ) ;
#88617 = CARTESIAN_POINT ( 'NONE',  ( 0.4325450954222598288, -2.349999999999997868, 0.000000000000000000 ) ) ;
#88618 = ORIENTED_EDGE ( 'NONE', *, *, #53572, .T. ) ;
#88619 = PLANE ( 'NONE',  #39532 ) ;
#88620 = LINE ( 'NONE', #11985, #30015 ) ;
#88621 = ORIENTED_EDGE ( 'NONE', *, *, #74726, .T. ) ;
#88622 = AXIS2_PLACEMENT_3D ( 'NONE', #22722, #38968, #14626 ) ;
#88623 = CARTESIAN_POINT ( 'NONE',  ( -108.5895376238167245, -23.47593901973091235, -1.443836447538999312 ) ) ;
#88624 = CARTESIAN_POINT ( 'NONE',  ( 20.49162120248849561, -0.4999214236376636200, 11.49999999999998934 ) ) ;
#88625 = ORIENTED_EDGE ( 'NONE', *, *, #42071, .F. ) ;
#88626 = AXIS2_PLACEMENT_3D ( 'NONE', #25750, #11516, #10519 ) ;
#88627 = ORIENTED_EDGE ( 'NONE', *, *, #55521, .T. ) ;
#88628 = VERTEX_POINT ( 'NONE', #48840 ) ;
#88629 = ADVANCED_FACE ( 'NONE', ( #79766 ), #10262, .T. ) ;
#88630 = CARTESIAN_POINT ( 'NONE',  ( 3.036358173076929123, -6.376774720514420736, 20.87990785256409865 ) ) ;
#88631 = CARTESIAN_POINT ( 'NONE',  ( -3.594920434497504758, 22.80983129501555950, 11.49999999999998934 ) ) ;
#88632 = CARTESIAN_POINT ( 'NONE',  ( -104.5908904681664637, -24.15620529776628800, 10.23563542870659759 ) ) ;
#88633 = CARTESIAN_POINT ( 'NONE',  ( -13.40315722217803973, 15.35114911505495172, -1.500000000000002220 ) ) ;
#88634 = ORIENTED_EDGE ( 'NONE', *, *, #48438, .T. ) ;
#88635 = CARTESIAN_POINT ( 'NONE',  ( -1.044792363895550302, -5.876774720514418071, 20.41272575174754422 ) ) ;
#88636 = CARTESIAN_POINT ( 'NONE',  ( -51.70072539166535108, -25.27314792116673203, 3.987152059579775809 ) ) ;
#88637 = VECTOR ( 'NONE', #98000, 1000.000000000000114 ) ;
#88638 = B_SPLINE_CURVE_WITH_KNOTS ( 'NONE', 3,
 ( #58721, #33888, #49132, #89673 ),
 .UNSPECIFIED., .F., .F.,
 ( 4, 4 ),
 ( 0.1989019938671915955, 0.1999027409079570106 ),
 .UNSPECIFIED. ) ;
#88639 = CARTESIAN_POINT ( 'NONE',  ( -105.5487342842852030, -24.73486907724918993, 1.287355809206962576 ) ) ;
#88640 = CARTESIAN_POINT ( 'NONE',  ( -111.6228709571500843, -23.47596703998600631, 11.44779298504227860 ) ) ;
#88641 = VERTEX_POINT ( 'NONE', #27497 ) ;
#88642 = CARTESIAN_POINT ( 'NONE',  ( -29.23473450784903704, -25.21532131873518878, 4.453842557699799976 ) ) ;
#88643 = CARTESIAN_POINT ( 'NONE',  ( -60.25625423781919210, -25.21083105912961742, 3.409327675794635581 ) ) ;
#88644 = VERTEX_POINT ( 'NONE', #67560 ) ;
#88645 = CARTESIAN_POINT ( 'NONE',  ( -20.76960556195881225, -0.3855258213679747525, 11.49999999999998934 ) ) ;
#88646 = ADVANCED_FACE ( 'NONE', ( #43226 ), #59951, .T. ) ;
#88647 = VERTEX_POINT ( 'NONE', #4157 ) ;
#88649 = VERTEX_POINT ( 'NONE', #98478 ) ;
#88648 = CARTESIAN_POINT ( 'NONE',  ( -109.5228709571500616, -23.48786465467242479, 11.44779295918253936 ) ) ;
#88650 = EDGE_CURVE ( 'NONE', #18719, #21744, #14517, .T. ) ;
#88651 = CARTESIAN_POINT ( 'NONE',  ( -129.6228709571500417, -24.64898659630367916, 1.056161002820834804 ) ) ;
#88652 = CARTESIAN_POINT ( 'NONE',  ( -51.28102184251170570, -25.30566280108310551, 5.070271677697943957 ) ) ;
#88653 = EDGE_LOOP ( 'NONE', ( #40466, #98104, #48196, #18143 ) ) ;
#88654 = ORIENTED_EDGE ( 'NONE', *, *, #30438, .F. ) ;
#88655 = CARTESIAN_POINT ( 'NONE',  ( -79.58953762381672448, -24.65952944569304250, 1.056160979905692354 ) ) ;
#88656 = CARTESIAN_POINT ( 'NONE',  ( 8.219458839706481612, 3.316774720514422015, -27.11006393991256758 ) ) ;
#88657 = CARTESIAN_POINT ( 'NONE',  ( -70.39323859381175907, -25.24515042351162819, 5.314174096928971913 ) ) ;
#88659 = ORIENTED_EDGE ( 'NONE', *, *, #78875, .T. ) ;
#88658 = CARTESIAN_POINT ( 'NONE',  ( -2.767897998228395551, 21.91458177938747909, 11.49999999999999645 ) ) ;
#88660 = EDGE_CURVE ( 'NONE', #99862, #6550, #82763, .T. ) ;
#88661 = CARTESIAN_POINT ( 'NONE',  ( -103.5221972675466731, -23.48783264082477018, -1.443836473390091246 ) ) ;
#88662 = CARTESIAN_POINT ( 'NONE',  ( 21.71239400539012721, -6.292901409244172406, 11.49999999999998934 ) ) ;
#88663 = VECTOR ( 'NONE', #15879, 1000.000000000000114 ) ;
#88664 = EDGE_CURVE ( 'NONE', #23202, #31248, #79943, .T. ) ;
#88666 = VERTEX_POINT ( 'NONE', #89885 ) ;
#88665 = CARTESIAN_POINT ( 'NONE',  ( 29.73860345376319358, 3.356774720514427379, 1.647607965253217621 ) ) ;
#88667 = ORIENTED_EDGE ( 'NONE', *, *, #68614, .F. ) ;
#88668 = AXIS2_PLACEMENT_3D ( 'NONE', #59972, #90907, #13764 ) ;
#88669 = DIRECTION ( 'NONE',  ( 0.000000000000000000, 0.9967269304714136968, 0.08084198211964954695 ) ) ;
#88670 = B_SPLINE_CURVE_WITH_KNOTS ( 'NONE', 3,
 ( #12514, #4913, #29738, #36359, #67315, #35858 ),
 .UNSPECIFIED., .F., .F.,
 ( 4, 2, 4 ),
 ( 6.391158118959990520E-06, 0.001387004593080782460, 0.002767618028042605031 ),
 .UNSPECIFIED. ) ;
#88671 = DIRECTION ( 'NONE',  ( 0.000000000000000000, -1.000000000000000000, 0.000000000000000000 ) ) ;
#88672 = ORIENTED_EDGE ( 'NONE', *, *, #3327, .F. ) ;
#88673 = CARTESIAN_POINT ( 'NONE',  ( -17.67215177357914513, -11.65580189297658897, -1.500000000000002220 ) ) ;
#88674 = CARTESIAN_POINT ( 'NONE',  ( -7.294102189209645815, -6.376774720514413630, 19.89644244529368677 ) ) ;
#88675 = DIRECTION ( 'NONE',  ( 1.000000000000000000, 0.000000000000000000, 0.000000000000000000 ) ) ;
#88676 = CARTESIAN_POINT ( 'NONE',  ( 10.93216147639808611, 19.43004700418156361, -1.500000000000002220 ) ) ;
#88677 = CARTESIAN_POINT ( 'NONE',  ( -88.88918693012689687, -29.50249591506787894, 5.947779886229223045 ) ) ;
#88678 = ORIENTED_EDGE ( 'NONE', *, *, #68009, .F. ) ;
#88679 = CARTESIAN_POINT ( 'NONE',  ( -5.563047341353722253, -6.376774720514413630, 20.06599527532950589 ) ) ;
#88680 = PLANE ( 'NONE',  #50836 ) ;
#88681 = VECTOR ( 'NONE', #56745, 1000.000000000000227 ) ;
#88682 = CARTESIAN_POINT ( 'NONE',  ( -36.55285608143805121, -23.96169478059712432, 10.65365249895718591 ) ) ;
#88683 = CARTESIAN_POINT ( 'NONE',  ( -126.5228709571500616, -24.64898659630368627, 1.056161002820834804 ) ) ;
#88684 = EDGE_CURVE ( 'NONE', #65705, #54440, #5641, .T. ) ;
#88685 = CARTESIAN_POINT ( 'NONE',  ( 2.628080361126900133, -19.32819128710564272, -1.500000000000002220 ) ) ;
#88686 = CARTESIAN_POINT ( 'NONE',  ( 21.15477495681221143, 3.540436534888726783, -1.500000000000002220 ) ) ;
#88687 = CARTESIAN_POINT ( 'NONE',  ( -26.15505896238250472, -24.92774839236926709, 2.424162040430986043 ) ) ;
#88688 = DIRECTION ( 'NONE',  ( -0.000000000000000000, 2.173523156925979552E-06, -0.9999999999976378895 ) ) ;
#88690 = B_SPLINE_CURVE_WITH_KNOTS ( 'NONE', 3,
 ( #24117, #55088, #33744, #25627, #56599, #8900 ),
 .UNSPECIFIED., .F., .F.,
 ( 4, 2, 4 ),
 ( 0.000000000000000000, 0.001380901958385389412, 0.002761803916770778824 ),
 .UNSPECIFIED. ) ;
#88689 = CARTESIAN_POINT ( 'NONE',  ( -77.64259777044621558, -23.73766607897670156, -1.055555164236459564 ) ) ;
#88691 = CARTESIAN_POINT ( 'NONE',  ( -12.51292883401962541, 18.98408452820241266, -1.500000000000002220 ) ) ;
#88692 = AXIS2_PLACEMENT_3D ( 'NONE', #88755, #3022, #87748 ) ;
#88693 = EDGE_CURVE ( 'NONE', #52065, #52789, #21849, .T. ) ;
#88694 = SHAPE_REPRESENTATION_RELATIONSHIP ( 'NONE' , 'NONE' ,  #9419, #54977 ) ;
#88695 = CARTESIAN_POINT ( 'NONE',  ( -98.50939101541317200, -24.51314013834315020, 0.6176544820404104019 ) ) ;
#88696 = CARTESIAN_POINT ( 'NONE',  ( 6.660000000000001030, -6.553980293839118509, 7.335060089566987962 ) ) ;
#88697 = CARTESIAN_POINT ( 'NONE',  ( -19.25010300378637851, 5.133817055790010464, 11.49999999999999645 ) ) ;
#88698 = CARTESIAN_POINT ( 'NONE',  ( -104.6353677949941954, -23.48783264082477373, -1.443836473390085917 ) ) ;
#88699 = AXIS2_PLACEMENT_3D ( 'NONE', #62851, #40496, #94770 ) ;
#88700 = LINE ( 'NONE', #72981, #68295 ) ;
#88701 = EDGE_LOOP ( 'NONE', ( #76126, #82140, #54955, #97512 ) ) ;
#88702 = DIRECTION ( 'NONE',  ( -0.000000000000000000, 1.000000000000000000, 0.000000000000000000 ) ) ;
#88703 = CARTESIAN_POINT ( 'NONE',  ( -89.81226385320383088, -29.50249917535260380, 7.447779886225679213 ) ) ;
#88704 = CARTESIAN_POINT ( 'NONE',  ( 21.66353188042378974, 1.267531592894010739, 11.49999999999998934 ) ) ;
#88705 = CARTESIAN_POINT ( 'NONE',  ( -84.52287095715011844, -23.96177878511309345, 10.65340807706330217 ) ) ;
#88706 = CARTESIAN_POINT ( 'NONE',  ( -18.49313839071750820, -6.238557295281221826, -1.500000000000002220 ) ) ;
#88707 = DIRECTION ( 'NONE',  ( 0.000000000000000000, -1.000000000000000000, 0.000000000000000000 ) ) ;
#88708 = ORIENTED_EDGE ( 'NONE', *, *, #63106, .T. ) ;
#88709 = PERSON_AND_ORGANIZATION ( #70597, #27821 ) ;
#88710 = DIRECTION ( 'NONE',  ( 0.000000000000000000, 1.000000000000000000, 1.155373159085149695E-17 ) ) ;
#88711 = CARTESIAN_POINT ( 'NONE',  ( -20.33632446988539400, 1.880062042347348195, 11.49999999999999645 ) ) ;
#88712 = CARTESIAN_POINT ( 'NONE',  ( 6.671786015990716301, -6.475225279485573360, -27.29955796265488033 ) ) ;
#88713 = DIRECTION ( 'NONE',  ( 0.000000000000000000, -1.000000000000000000, 0.000000000000000000 ) ) ;
#88714 = EDGE_CURVE ( 'NONE', #38179, #12874, #20354, .T. ) ;
#88715 = ORIENTED_EDGE ( 'NONE', *, *, #67775, .T. ) ;
#88716 = PLANE ( 'NONE',  #94518 ) ;
#88717 = CARTESIAN_POINT ( 'NONE',  ( -39.46304919600096639, -25.18431026911589754, 4.009749832163960193 ) ) ;
#88718 = LINE ( 'NONE', #94317, #94357 ) ;
#88719 = CARTESIAN_POINT ( 'NONE',  ( -32.07722060962684196, -24.87479601683932984, 8.247789944617052171 ) ) ;
#88720 = EDGE_LOOP ( 'NONE', ( #64315, #43192, #32243, #77952 ) ) ;
#88721 = ADVANCED_FACE ( 'NONE', ( #96998 ), #44713, .F. ) ;
#88722 = DIRECTION ( 'NONE',  ( 0.000000000000000000, 0.000000000000000000, 1.000000000000000000 ) ) ;
#88723 = VECTOR ( 'NONE', #42619, 1000.000000000000114 ) ;
#88724 = EDGE_CURVE ( 'NONE', #70078, #63086, #30714, .T. ) ;
#88725 = EDGE_CURVE ( 'NONE', #12246, #31523, #94499, .T. ) ;
#88726 = B_SPLINE_CURVE_WITH_KNOTS ( 'NONE', 3,
 ( #42394, #94650, #95658, #32749, #96648, #41884 ),
 .UNSPECIFIED., .F., .F.,
 ( 4, 2, 4 ),
 ( 0.000000000000000000, 0.001380901958385392448, 0.002761803916770784895 ),
 .UNSPECIFIED. ) ;
#88727 = CARTESIAN_POINT ( 'NONE',  ( 8.272623322502495213, 21.45567517505680044, 11.49999999999999645 ) ) ;
#88728 = CARTESIAN_POINT ( 'NONE',  ( 12.23086119556625206, 19.17791753167082192, -1.500000000000002220 ) ) ;
#88729 = CARTESIAN_POINT ( 'NONE',  ( 4.959846025536391423, -6.376774720514417183, 20.32314756232572250 ) ) ;
#88730 = B_SPLINE_SURFACE_WITH_KNOTS ( 'NONE', 3, 1, ( 
 ( #39494, #63353 ),
 ( #92763, #8541 ),
 ( #47614, #48623 ),
 ( #423, #25259 ),
 ( #17653, #78533 ),
 ( #38985, #62339 ),
 ( #40498, #8034 ),
 ( #9037, #39990 ),
 ( #15646, #71453 ),
 ( #86660, #70950 ),
 ( #93265, #70444 ),
 ( #69935, #79549 ),
 ( #54729, #1439 ),
 ( #85664, #56238 ),
 ( #16144, #47116 ),
 ( #17149, #87163 ),
 ( #32376, #94269 ),
 ( #24753, #10039 ),
 ( #40999, #931 ) ),
 .UNSPECIFIED., .F., .F., .F.,
 ( 4, 1, 1, 1, 1, 1, 1, 1, 1, 1, 1, 1, 1, 1, 1, 1, 4 ),
 ( 2, 2 ),
 ( 0.000000000000000000, 0.07855643335270047489, 0.1528628401420922822, 0.2235596934382872158, 0.2903749439782072894, 0.3554030728222035140, 0.4182911570440911442, 0.4803885637756447058, 0.5430726152062789192, 0.6049239444620954087, 0.6643983091132997787, 0.7219425547367019913, 0.7783748910546737232, 0.8338299406509398493, 0.8888612363188844734, 0.9440889395778866433, 1.000000000000000000 ),
 ( 0.000000000000000000, 1.000000000000000000 ),
 .UNSPECIFIED. ) ;
#88731 = CARTESIAN_POINT ( 'NONE',  ( -19.77875734969026311, 3.316774720514426456, 29.49402280011862487 ) ) ;
#88732 = CARTESIAN_POINT ( 'NONE',  ( -90.59507163750394909, -24.15503026093915651, -0.2815557561904460382 ) ) ;
#88733 = EDGE_CURVE ( 'NONE', #38686, #44615, #12187, .T. ) ;
#88734 = AXIS2_PLACEMENT_3D ( 'NONE', #39875, #15029, #30254 ) ;
#88735 = CARTESIAN_POINT ( 'NONE',  ( -124.9228709571500531, -23.47593901973090524, -1.443836447538996204 ) ) ;
#88736 = CARTESIAN_POINT ( 'NONE',  ( -44.62287095715004881, -23.48783264082478084, -1.443836473390072150 ) ) ;
#88737 = CARTESIAN_POINT ( 'NONE',  ( -19.96805355746080934, -8.928269573510897672, 11.49999999999998934 ) ) ;
#88738 = CARTESIAN_POINT ( 'NONE',  ( -74.52287095715007581, -24.64898659630528854, 1.056161002820824368 ) ) ;
#88739 = CARTESIAN_POINT ( 'NONE',  ( 11.05000000000000249, 0.000000000000000000, 0.000000000000000000 ) ) ;
#88740 = CARTESIAN_POINT ( 'NONE',  ( -120.6228709571500417, -24.99132157543166954, 2.256160258750667502 ) ) ;
#88741 = DIRECTION ( 'NONE',  ( 0.09824042138329625029, 0.9951627101165079203, 3.504396110891627214E-15 ) ) ;
#88742 = ORIENTED_EDGE ( 'NONE', *, *, #13451, .T. ) ;
#88743 = CARTESIAN_POINT ( 'NONE',  ( 12.15263457413992576, -16.39098610538439615, 11.49999999999998934 ) ) ;
#88744 = VERTEX_POINT ( 'NONE', #52823 ) ;
#88745 = ORIENTED_EDGE ( 'NONE', *, *, #26195, .F. ) ;
#88746 = VERTEX_POINT ( 'NONE', #68545 ) ;
#88747 = ORIENTED_EDGE ( 'NONE', *, *, #40823, .F. ) ;
#88748 = ADVANCED_FACE ( 'NONE', ( #54332 ), #92373, .F. ) ;
#88749 = ADVANCED_FACE ( 'NONE', ( #29973 ), #62440, .F. ) ;
#88750 = CARTESIAN_POINT ( 'NONE',  ( -20.90396053131702914, -9.656267258341529214, -1.500000000000002220 ) ) ;
#88751 = CARTESIAN_POINT ( 'NONE',  ( -60.62287095715004881, -29.50247984919015209, -1.443849546365056913 ) ) ;
#88752 = CARTESIAN_POINT ( 'NONE',  ( -19.56588111578679090, -4.897929960003377658, -1.500000000000002220 ) ) ;
#88753 = ORIENTED_EDGE ( 'NONE', *, *, #63727, .F. ) ;
#88754 = CARTESIAN_POINT ( 'NONE',  ( -67.62287095715002749, -24.35013146730203815, 9.818937971375108376 ) ) ;
#88755 = CARTESIAN_POINT ( 'NONE',  ( 282.9764569301858046, -5.965225279485572685, 20.79159422840526616 ) ) ;
#88756 = CARTESIAN_POINT ( 'NONE',  ( -101.5228709571500758, -23.48786465467241769, 11.44779295918254114 ) ) ;
#88757 = CARTESIAN_POINT ( 'NONE',  ( -53.60570705064769470, -23.73791477778911485, 11.05961554403170766 ) ) ;
#88759 = ORIENTED_EDGE ( 'NONE', *, *, #83495, .T. ) ;
#88758 = CARTESIAN_POINT ( 'NONE',  ( 21.01207135711032237, 3.775690236426352264, 11.49999999999999645 ) ) ;
#88760 = CARTESIAN_POINT ( 'NONE',  ( 6.887358010905132666, -5.876774720514425177, 21.32574817943157086 ) ) ;
#88761 = VERTEX_POINT ( 'NONE', #1034 ) ;
#88762 = CARTESIAN_POINT ( 'NONE',  ( 22.17158117043571863, -1.905908075979310334, 11.49999999999998934 ) ) ;
#88763 = CARTESIAN_POINT ( 'NONE',  ( -19.97286373971314433, -5.326668811655218327, 11.49999999999998934 ) ) ;
#88764 = EDGE_CURVE ( 'NONE', #83886, #93143, #61942, .T. ) ;
#88765 = PERSON ( 'NAUO-PER2', 'UNSPECIFIED', 'UNSPECIFIED', ('UNSPECIFIED'), ('UNSPECIFIED'), ('UNSPECIFIED') ) ;
#88766 = ORIENTED_EDGE ( 'NONE', *, *, #7647, .F. ) ;
#88767 = CARTESIAN_POINT ( 'NONE',  ( 3.202571139211427553, -5.876774720514407413, 18.81074098386681470 ) ) ;
#88768 = ORIENTED_EDGE ( 'NONE', *, *, #58101, .F. ) ;
#88769 = CARTESIAN_POINT ( 'NONE',  ( -78.62287095715005592, -23.47593901973091235, -1.443836447539004642 ) ) ;
#88770 = AXIS2_PLACEMENT_3D ( 'NONE', #69455, #84172, #45132 ) ;
#88771 = ORIENTED_EDGE ( 'NONE', *, *, #69014, .F. ) ;
#88772 = CARTESIAN_POINT ( 'NONE',  ( -50.21186637932700592, -25.10935128237196068, 2.837931291232954401 ) ) ;
#88773 = CARTESIAN_POINT ( 'NONE',  ( -18.75169668496848985, 9.291489096422434812, -1.500000000000002220 ) ) ;
#88774 = CARTESIAN_POINT ( 'NONE',  ( -21.18249553426131015, -5.656070447573528170, 11.49999999999999645 ) ) ;
#88775 = EDGE_CURVE ( 'NONE', #43186, #7527, #10939, .T. ) ;
#88776 = CARTESIAN_POINT ( 'NONE',  ( -73.62685146875698194, -24.51419770103157347, 9.386484678747175181 ) ) ;
#88777 = CARTESIAN_POINT ( 'NONE',  ( -21.69688529672534827, 6.072505851105969299, -1.500000000000002220 ) ) ;
#88778 = CARTESIAN_POINT ( 'NONE',  ( 5.463070048063013218, -20.23478146675526190, -1.500000000000002220 ) ) ;
#88779 = EDGE_CURVE ( 'NONE', #31830, #65938, #14484, .T. ) ;
#88780 = CARTESIAN_POINT ( 'NONE',  ( -26.33488822642538452, -24.97067133876658929, 6.524121684135936405 ) ) ;
#88781 = CARTESIAN_POINT ( 'NONE',  ( 6.059061188053544988, -5.876774720514417183, 20.16803580207560742 ) ) ;
#88782 = LINE ( 'NONE', #19248, #68026 ) ;
#88783 = CARTESIAN_POINT ( 'NONE',  ( -53.01255352321339842, -2.682774720514426559, 35.59556822165056644 ) ) ;
#88784 = ORIENTED_EDGE ( 'NONE', *, *, #15797, .T. ) ;
#88785 = EDGE_CURVE ( 'NONE', #23597, #79746, #6639, .T. ) ;
#88786 = ORIENTED_EDGE ( 'NONE', *, *, #27309, .F. ) ;
#88787 = ORIENTED_EDGE ( 'NONE', *, *, #24930, .T. ) ;
#88788 = CARTESIAN_POINT ( 'NONE',  ( -94.62287095715005592, -23.47593901973091235, -1.443836447539002865 ) ) ;
#88789 = ORIENTED_EDGE ( 'NONE', *, *, #4304, .F. ) ;
#88790 = CARTESIAN_POINT ( 'NONE',  ( 16.48747857468482891, 13.79107804547330929, -1.500000000000002220 ) ) ;
#88791 = EDGE_CURVE ( 'NONE', #26599, #13615, #48511, .T. ) ;
#88792 = ORIENTED_EDGE ( 'NONE', *, *, #95705, .F. ) ;
#88793 = FACE_OUTER_BOUND ( 'NONE', #50498, .T. ) ;
#88794 = CARTESIAN_POINT ( 'NONE',  ( 5.994809752082427501, 20.21905721239408393, 11.49999999999998934 ) ) ;
#88795 = DIRECTION ( 'NONE',  ( -0.000000000000000000, -1.000000000000000000, -0.000000000000000000 ) ) ;
#88796 = CARTESIAN_POINT ( 'NONE',  ( -64.65370588801016538, -23.48783264082477018, -1.443836473390096353 ) ) ;
#88797 = CARTESIAN_POINT ( 'NONE',  ( -50.67080941327229482, -23.48786465467240347, 11.44779295918255002 ) ) ;
#88798 = CARTESIAN_POINT ( 'NONE',  ( -101.5146404698777900, -24.15543982623907482, -0.2315651400026588758 ) ) ;
#88799 = DIRECTION ( 'NONE',  ( 1.000000000000000000, 0.000000000000000000, 0.000000000000000000 ) ) ;
#88800 = CARTESIAN_POINT ( 'NONE',  ( -10.28628152547328511, -19.52461415289770130, -1.500000000000002220 ) ) ;
#88801 = EDGE_LOOP ( 'NONE', ( #66911, #41983, #72742, #9270 ) ) ;
#88802 = CARTESIAN_POINT ( 'NONE',  ( -116.6243012131220240, -24.51314013834316086, 0.6176544820404278324 ) ) ;
#88803 = FACE_OUTER_BOUND ( 'NONE', #47623, .T. ) ;
#88804 = CARTESIAN_POINT ( 'NONE',  ( -40.49165087243459737, -25.27956071481186839, 5.543942911029563270 ) ) ;
#88805 = VECTOR ( 'NONE', #31750, 1000.000000000000000 ) ;
#88806 = CARTESIAN_POINT ( 'NONE',  ( -29.85657701416236520, -24.77034389998055985, 1.590605884330587916 ) ) ;
#88807 = DIRECTION ( 'NONE',  ( 1.000000000000000000, -0.000000000000000000, 0.000000000000000000 ) ) ;
#88808 = CARTESIAN_POINT ( 'NONE',  ( 18.61059577090848549, -10.47110149595715711, -1.500000000000002220 ) ) ;
#88809 = CARTESIAN_POINT ( 'NONE',  ( -70.35231919018949043, -25.31467665484316854, 4.853663865497455987 ) ) ;
#88810 = CARTESIAN_POINT ( 'NONE',  ( -89.80335865247931793, -25.31768024997816724, 4.634761245912266681 ) ) ;
#88811 = CARTESIAN_POINT ( 'NONE',  ( -64.58768515828387535, -24.35071581493543391, 9.817618358456023486 ) ) ;
#88812 = CARTESIAN_POINT ( 'NONE',  ( -80.77696901427715659, -25.12955870785331669, 7.063884950381287275 ) ) ;
#88813 = CARTESIAN_POINT ( 'NONE',  ( 21.16457415087624128, -7.944649954575952577, -1.500000000000002220 ) ) ;
#88814 = B_SPLINE_SURFACE_WITH_KNOTS ( 'NONE', 3, 3, ( 
 ( #51715, #75031, #76030, #36984 ),
 ( #91756, #84149, #82655, #66473 ),
 ( #98873, #97870, #83148, #13630 ),
 ( #44601, #6031, #67947, #97388 ),
 ( #43109, #6535, #82158, #37484 ),
 ( #68436, #29866, #60839, #22235 ),
 ( #27873, #12642, #43605, #15640 ) ),
 .UNSPECIFIED., .F., .F., .F.,
 ( 4, 3, 4 ),
 ( 4, 4 ),
 ( 0.0004766839783814535341, 0.1029713700210890953, 0.2054660560637967259 ),
 ( 0.6396567149882574910, 0.6409645759772608642 ),
 .UNSPECIFIED. ) ;
#88815 = PLANE ( 'NONE',  #97670 ) ;
#88816 = ORIENTED_EDGE ( 'NONE', *, *, #75741, .F. ) ;
#88817 = CARTESIAN_POINT ( 'NONE',  ( 0.000000000000000000, -1.473225279485573802, 0.000000000000000000 ) ) ;
#88818 = FACE_OUTER_BOUND ( 'NONE', #12754, .T. ) ;
#88819 = CARTESIAN_POINT ( 'NONE',  ( -16.30015253881794379, -11.17962500214296639, 11.49999999999999645 ) ) ;
#88820 = DIRECTION ( 'NONE',  ( 0.000000000000000000, 0.000000000000000000, 1.000000000000000000 ) ) ;
#88821 = CARTESIAN_POINT ( 'NONE',  ( -96.52287095715007581, -23.47593901973090524, -1.443836447538996648 ) ) ;
#88822 = B_SPLINE_CURVE_WITH_KNOTS ( 'NONE', 3,
 ( #5127, #82743, #13727, #76127, #13226, #43695, #36080 ),
 .UNSPECIFIED., .F., .F.,
 ( 4, 1, 1, 1, 4 ),
 ( 0.3452202732246780759, 0.4949101844912719983, 0.6446000957578658097, 0.7942900070244596211, 0.9439799182910535436 ),
 .UNSPECIFIED. ) ;
#88823 = ORIENTED_EDGE ( 'NONE', *, *, #55865, .T. ) ;
#88824 = CARTESIAN_POINT ( 'NONE',  ( -80.64675904551154417, -25.21083105912962807, 3.409327675794629808 ) ) ;
#88825 = CARTESIAN_POINT ( 'NONE',  ( -110.5895376238167245, -23.47593901973091235, -1.443836447538999312 ) ) ;
#88826 = CARTESIAN_POINT ( 'NONE',  ( -113.5228709571500616, -24.64898659630368627, 1.056161002820831474 ) ) ;
#88827 = CARTESIAN_POINT ( 'NONE',  ( -19.28869470675124731, 9.786980993800005635, 11.49999999999998934 ) ) ;
#88828 = DIRECTION ( 'NONE',  ( 0.000000000000000000, -2.173523156925980399E-06, 0.9999999999976378895 ) ) ;
#88829 = CIRCLE ( 'NONE', #77419, 3.349999999999998757 ) ;
#88830 = CARTESIAN_POINT ( 'NONE',  ( -66.52287095715006160, -23.96177878511308990, 10.65340807706329684 ) ) ;
#88831 = CARTESIAN_POINT ( 'NONE',  ( -92.58953762381671027, -23.48783264082479150, -1.443836473390063713 ) ) ;
#88832 = CARTESIAN_POINT ( 'NONE',  ( 26.37445894957760117, -1.682774720514426114, -11.69480419648520986 ) ) ;
#88833 = CARTESIAN_POINT ( 'NONE',  ( -10.52764212615999639, 16.74383705166681580, -1.500000000000002220 ) ) ;
#88834 = ORIENTED_EDGE ( 'NONE', *, *, #43721, .T. ) ;
#88835 = CARTESIAN_POINT ( 'NONE',  ( -8.208445925564873846, -18.52556626786687488, 11.49999999999999645 ) ) ;
#88836 = CARTESIAN_POINT ( 'NONE',  ( -112.6228709571501412, -24.35013146730204170, 9.818937971375106599 ) ) ;
#88837 = VECTOR ( 'NONE', #25865, 1000.000000000000114 ) ;
#88838 = EDGE_CURVE ( 'NONE', #89557, #87707, #53830, .T. ) ;
#88839 = VERTEX_POINT ( 'NONE', #45711 ) ;
#88840 = DIRECTION ( 'NONE',  ( 0.000000000000000000, -1.000000000000000000, 0.000000000000000000 ) ) ;
#88841 = CARTESIAN_POINT ( 'NONE',  ( 33.62089986283198328, 3.615790004618635312, -11.40738377976237672 ) ) ;
#88842 = CARTESIAN_POINT ( 'NONE',  ( -59.62287095715004881, -29.50250243563736774, 8.947779886222145151 ) ) ;
#88843 = ADVANCED_FACE ( 'NONE', ( #85258 ), #69552, .T. ) ;
#88844 = AXIS2_PLACEMENT_3D ( 'NONE', #1356, #92678, #31797 ) ;
#88845 = CARTESIAN_POINT ( 'NONE',  ( -47.62287095715004881, -29.50250243563736774, 8.947779886222146928 ) ) ;
#88846 = EDGE_CURVE ( 'NONE', #14525, #90882, #7137, .T. ) ;
#88847 = CARTESIAN_POINT ( 'NONE',  ( -5.366453405989236813, 0.000000000000000000, 4.450000000000000178 ) ) ;
#88848 = CARTESIAN_POINT ( 'NONE',  ( 17.53424486177994623, -9.724335930198575895, -1.500000000000002220 ) ) ;
#88849 = ADVANCED_FACE ( 'NONE', ( #92871 ), #23349, .F. ) ;
#88850 = CARTESIAN_POINT ( 'NONE',  ( -51.62287095715005592, -23.47596703998600631, 11.44779298504227505 ) ) ;
#88851 = ORIENTED_EDGE ( 'NONE', *, *, #13111, .T. ) ;
#88852 = ADVANCED_FACE ( 'NONE', ( #46206 ), #15751, .T. ) ;
#88853 = EDGE_CURVE ( 'NONE', #51364, #88644, #22930, .T. ) ;
#88854 = CARTESIAN_POINT ( 'NONE',  ( -73.62287095715009855, -23.95044443724992433, 10.65354141964649948 ) ) ;
#88855 = PLANE ( 'NONE',  #13702 ) ;
#88856 = CARTESIAN_POINT ( 'NONE',  ( 6.150000000000003908, 1.999999999999998224, 24.00000000000000000 ) ) ;
#88857 = PLANE ( 'NONE',  #82092 ) ;
#88858 = CARTESIAN_POINT ( 'NONE',  ( -73.56460343122959955, -23.48783264082477018, -1.443836473390094355 ) ) ;
#88859 = CARTESIAN_POINT ( 'NONE',  ( -24.90875734969025501, -3.316774720514426456, 30.51402280011862089 ) ) ;
#88860 = B_SPLINE_CURVE_WITH_KNOTS ( 'NONE', 3,
 ( #77184, #7690, #36643, #67610, #98528, #60000, #90929, #13792 ),
 .UNSPECIFIED., .F., .F.,
 ( 4, 2, 2, 4 ),
 ( -0.001224873891641426078, -0.0002244903592271097967, 0.0007758931731872064849, 0.002776660238015834711 ),
 .UNSPECIFIED. ) ;
#88861 = CARTESIAN_POINT ( 'NONE',  ( -93.52287095715006160, -24.64898659630368272, 1.056161002820827921 ) ) ;
#88862 = ORIENTED_EDGE ( 'NONE', *, *, #20552, .T. ) ;
#88863 = CARTESIAN_POINT ( 'NONE',  ( -18.82647582233506611, 7.659846263794035437, -1.500000000000002220 ) ) ;
#88864 = ORIENTED_EDGE ( 'NONE', *, *, #6148, .T. ) ;
#88865 = EDGE_CURVE ( 'NONE', #15988, #62185, #66677, .T. ) ;
#88866 = CARTESIAN_POINT ( 'NONE',  ( -0.4961427919413599064, 22.93664481792237453, 11.49999999999998934 ) ) ;
#88867 = CARTESIAN_POINT ( 'NONE',  ( -32.59412366074091949, -24.15543982623907127, -0.2315651400026567941 ) ) ;
#88868 = ORIENTED_EDGE ( 'NONE', *, *, #73374, .T. ) ;
#88869 = CARTESIAN_POINT ( 'NONE',  ( 6.499999999999993783, 2.999999999999999556, 4.499999999999999112 ) ) ;
#88870 = CARTESIAN_POINT ( 'NONE',  ( -76.52287095715007581, -24.64898659630528854, 1.056161002820826145 ) ) ;
#88871 = EDGE_CURVE ( 'NONE', #73153, #58829, #93367, .T. ) ;
#88872 = CYLINDRICAL_SURFACE ( 'NONE', #73990, 129.7684398600581517 ) ;
#88873 = CARTESIAN_POINT ( 'NONE',  ( -19.98373207111551508, 7.008865001458166155, 11.49999999999999645 ) ) ;
#88874 = CARTESIAN_POINT ( 'NONE',  ( 9.107982344273736430, -20.20341329189913537, 11.49999999999998934 ) ) ;
#88875 = CARTESIAN_POINT ( 'NONE',  ( 11.80677006232881254, 16.86875346446678137, -1.500000000000002220 ) ) ;
#88876 = ORIENTED_EDGE ( 'NONE', *, *, #34073, .F. ) ;
#88877 = CARTESIAN_POINT ( 'NONE',  ( -41.56077753939339203, -23.73766607897670866, -1.055555164236442023 ) ) ;
#88878 = ORIENTED_EDGE ( 'NONE', *, *, #27469, .F. ) ;
#88879 = CARTESIAN_POINT ( 'NONE',  ( -54.48738976181418536, -24.65952944569304606, 1.056160979905696573 ) ) ;
#88880 = DIRECTION ( 'NONE',  ( -0.000000000000000000, 1.000000000000000000, -0.000000000000000000 ) ) ;
#88881 = VERTEX_POINT ( 'NONE', #48219 ) ;
#88882 = EDGE_LOOP ( 'NONE', ( #6993, #96615, #67403, #50631 ) ) ;
#88883 = ORIENTED_EDGE ( 'NONE', *, *, #80705, .F. ) ;
#88884 = CARTESIAN_POINT ( 'NONE',  ( 2.230654205607476293, -6.505213034913026604E-16, -0.1647943925233646134 ) ) ;
#88885 = CARTESIAN_POINT ( 'NONE',  ( -28.54452471549034698, -23.99578543409190701, 10.23563545308467226 ) ) ;
#88886 = CARTESIAN_POINT ( 'NONE',  ( -64.52287095715006160, -23.48786465467241769, 11.44779295918254824 ) ) ;
#88887 = CARTESIAN_POINT ( 'NONE',  ( 2.040502595053849788, 20.68626321094233944, -1.500000000000002220 ) ) ;
#88888 = CARTESIAN_POINT ( 'NONE',  ( -16.45766974254678061, 14.19212061201335473, 11.49999999999999645 ) ) ;
#88889 = ORIENTED_EDGE ( 'NONE', *, *, #49549, .F. ) ;
#88890 = CARTESIAN_POINT ( 'NONE',  ( -69.65500149314945588, -25.14915147881072244, 2.995210818656448115 ) ) ;
#88891 = CARTESIAN_POINT ( 'NONE',  ( -115.5133559575585451, -25.00158670708910691, 2.256160236439219258 ) ) ;
#88892 = CARTESIAN_POINT ( 'NONE',  ( 21.53444271425275858, 6.169869319618734416, -1.500000000000002220 ) ) ;
#88893 = AXIS2_PLACEMENT_3D ( 'NONE', #95318, #87708, #80091 ) ;
#88894 = EDGE_CURVE ( 'NONE', #1657, #14465, #53397, .T. ) ;
#88895 = CARTESIAN_POINT ( 'NONE',  ( -124.5228709571500900, -23.48783264082477373, -1.443836473390085029 ) ) ;
#88896 = CARTESIAN_POINT ( 'NONE',  ( -71.62287095715005592, -24.34917612406837861, 0.1852690917426617345 ) ) ;
#88897 = ORIENTED_EDGE ( 'NONE', *, *, #40497, .F. ) ;
#88898 = CARTESIAN_POINT ( 'NONE',  ( -45.52287095715006160, -24.99132157543083821, 2.256160258750667502 ) ) ;
#88899 = CARTESIAN_POINT ( 'NONE',  ( -77.55620429048339304, -23.47596703998600276, 11.44779298504227683 ) ) ;
#88900 = ORIENTED_EDGE ( 'NONE', *, *, #5208, .F. ) ;
#88901 = ORIENTED_EDGE ( 'NONE', *, *, #20794, .F. ) ;
#88902 = EDGE_CURVE ( 'NONE', #79246, #76974, #38745, .T. ) ;
#88903 = CARTESIAN_POINT ( 'NONE',  ( -103.6228709571500559, -23.47593901973091235, -1.443836447539001089 ) ) ;
#88904 = ORIENTED_EDGE ( 'NONE', *, *, #46979, .F. ) ;
#88905 = CARTESIAN_POINT ( 'NONE',  ( -13.59518820711925358, -16.35513075224449864, -1.500000000000002220 ) ) ;
#88906 = ORIENTED_EDGE ( 'NONE', *, *, #1812, .F. ) ;
#88907 = CARTESIAN_POINT ( 'NONE',  ( 22.81105451610979173, -4.772774720514425972, -18.46691820600746681 ) ) ;
#88908 = CARTESIAN_POINT ( 'NONE',  ( -9.754611696910345131, 19.53525426502628548, 11.49999999999998934 ) ) ;
#88909 = CARTESIAN_POINT ( 'NONE',  ( -52.65922807883639223, -23.48786465467240703, 11.44779295918255180 ) ) ;
#88910 = CARTESIAN_POINT ( 'NONE',  ( 2.978076788109338402, -22.46882643481310282, -1.500000000000002220 ) ) ;
#88911 = FACE_OUTER_BOUND ( 'NONE', #3547, .T. ) ;
#88912 = CARTESIAN_POINT ( 'NONE',  ( -49.52287095715005449, -24.51387760970724727, 9.387446482453427166 ) ) ;
#88913 = CARTESIAN_POINT ( 'NONE',  ( -21.85961425739535358, 0.8689724601130633941, -1.500000000000002220 ) ) ;
#88914 = CARTESIAN_POINT ( 'NONE',  ( 7.166666666666669627, -5.876774720514419847, 20.78665865384615330 ) ) ;
#88915 = ORIENTED_EDGE ( 'NONE', *, *, #71874, .F. ) ;
#88916 = CARTESIAN_POINT ( 'NONE',  ( -65.62287095715005592, -23.48783264082478084, -1.443836473390067265 ) ) ;
#88917 = CARTESIAN_POINT ( 'NONE',  ( -49.21454750704995007, -25.26337504824086722, 7.069183330828471057 ) ) ;
#88918 = ORIENTED_EDGE ( 'NONE', *, *, #39711, .F. ) ;
#88919 = CARTESIAN_POINT ( 'NONE',  ( -32.52287095715006160, -24.33927499327854349, 9.819080762295817166 ) ) ;
#88920 = VECTOR ( 'NONE', #94954, 1000.000000000000000 ) ;
#88921 = ORIENTED_EDGE ( 'NONE', *, *, #68881, .F. ) ;
#88922 = CARTESIAN_POINT ( 'NONE',  ( -128.5562042904834357, -23.47596703998600631, 11.44779298504227683 ) ) ;
#88923 = LINE ( 'NONE', #29001, #18964 ) ;
#88924 = CARTESIAN_POINT ( 'NONE',  ( -19.44786352930952233, -8.617208915446557427, -1.500000000000002220 ) ) ;
#88925 = DIRECTION ( 'NONE',  ( 1.000000000000000000, 0.000000000000000000, 0.000000000000000000 ) ) ;
#88926 = CARTESIAN_POINT ( 'NONE',  ( -26.30595710371889950, -24.75186218799666804, 3.418819366253220693 ) ) ;
#88927 = CARTESIAN_POINT ( 'NONE',  ( -85.60108179270328321, -23.85016227208579664, -0.8807180028928370819 ) ) ;
#88928 = CARTESIAN_POINT ( 'NONE',  ( -68.55393007522499715, -23.96119346886880663, -0.6495511937832112448 ) ) ;
#88929 = CARTESIAN_POINT ( 'NONE',  ( -117.5579608062422921, -23.48786465467241769, 11.44779295918253581 ) ) ;
#88930 = ORIENTED_EDGE ( 'NONE', *, *, #35373, .F. ) ;
#88931 = CARTESIAN_POINT ( 'NONE',  ( 8.254404603115069960, -17.72612730319335839, 11.49999999999999645 ) ) ;
#88932 = DIRECTION ( 'NONE',  ( -0.000000000000000000, -1.000000000000000000, -0.000000000000000000 ) ) ;
#88933 = CARTESIAN_POINT ( 'NONE',  ( -79.34687923781920915, -25.26778825442007559, 5.960409282772108241 ) ) ;
#88934 = ORIENTED_EDGE ( 'NONE', *, *, #44459, .T. ) ;
#88935 = CARTESIAN_POINT ( 'NONE',  ( -104.5228709571500758, -24.64898659630529565, 1.056161002820829697 ) ) ;
#88936 = CARTESIAN_POINT ( 'NONE',  ( -99.63322708413970474, -25.25095836864358745, 5.473920322365175117 ) ) ;
#88937 = CARTESIAN_POINT ( 'NONE',  ( -90.62287095715004170, -23.47593901973091235, -1.443836447539002865 ) ) ;
#88938 = CARTESIAN_POINT ( 'NONE',  ( -60.52287095715009002, -24.15431212366390312, -0.2830839119429246487 ) ) ;
#88939 = CARTESIAN_POINT ( 'NONE',  ( 3.778003860535555702, 19.31821889988591323, -1.500000000000002220 ) ) ;
#88940 = ORIENTED_EDGE ( 'NONE', *, *, #26241, .F. ) ;
#88941 = LINE ( 'NONE', #96545, #66742 ) ;
#88942 = CARTESIAN_POINT ( 'NONE',  ( -15.82668884360736961, 6.475225279485576024, 42.07822029717483758 ) ) ;
#88943 = EDGE_CURVE ( 'NONE', #51332, #55726, #71556, .T. ) ;
#88944 = APPLICATION_PROTOCOL_DEFINITION ( 'international standard', 'config_control_design', 1994, #89372 ) ;
#88945 = ORIENTED_EDGE ( 'NONE', *, *, #88327, .T. ) ;
#88946 = CARTESIAN_POINT ( 'NONE',  ( -99.52764846858842418, -25.26416398485831749, 3.999772271414141489 ) ) ;
#88947 = DIRECTION ( 'NONE',  ( -5.238131417152343399E-15, 0.000000000000000000, -1.000000000000000000 ) ) ;
#88948 = CARTESIAN_POINT ( 'NONE',  ( -84.62287095715005592, -24.66019654487199730, 8.947790411086128159 ) ) ;
#88949 = CARTESIAN_POINT ( 'NONE',  ( -97.50710338837967583, -24.66019654487199730, 8.947790411086115725 ) ) ;
#88950 = CARTESIAN_POINT ( 'NONE',  ( -47.62287095715004881, -23.48786465467240703, 11.44779295918255180 ) ) ;
#88951 = VECTOR ( 'NONE', #12591, 1000.000000000000000 ) ;
#88952 = ADVANCED_FACE ( 'NONE', ( #94376 ), #17252, .T. ) ;
#88953 = AXIS2_PLACEMENT_3D ( 'NONE', #96592, #88993, #25585 ) ;
#88954 = DIRECTION ( 'NONE',  ( 0.000000000000000000, 1.000000000000000000, 0.000000000000000000 ) ) ;
#88955 = B_SPLINE_CURVE_WITH_KNOTS ( 'NONE', 3,
 ( #94548, #65138, #18925, #10822, #26554, #88453, #18433, #27050 ),
 .UNSPECIFIED., .F., .F.,
 ( 4, 2, 2, 4 ),
 ( -0.001224554619866345413, -0.0002241820295893650998, 0.0007761905606876152129, 0.002776935741241572369 ),
 .UNSPECIFIED. ) ;
#88956 = CARTESIAN_POINT ( 'NONE',  ( -73.52287095715010423, -23.94994826722564696, -0.6494450866342716955 ) ) ;
#88957 = CARTESIAN_POINT ( 'NONE',  ( 10.26108024787556516, -17.11367029881254709, -1.500000000000002220 ) ) ;
#88958 = EDGE_CURVE ( 'NONE', #82876, #60813, #43654, .T. ) ;
#88959 = CARTESIAN_POINT ( 'NONE',  ( 13.91401389203221406, -5.965225279485572685, 158.0376437107427137 ) ) ;
#88960 = CARTESIAN_POINT ( 'NONE',  ( 12.81631318294326505, -15.22695477405695996, -1.500000000000002220 ) ) ;
#88961 = ORIENTED_EDGE ( 'NONE', *, *, #84601, .T. ) ;
#88962 = VECTOR ( 'NONE', #31161, 1000.000000000000114 ) ;
#88963 = CARTESIAN_POINT ( 'NONE',  ( -93.62287095715005592, -29.50250786944525672, 11.44777988621623344 ) ) ;
#88964 = EDGE_CURVE ( 'NONE', #21001, #10246, #10649, .T. ) ;
#88965 = ADVANCED_FACE ( 'NONE', ( #2048 ), #95381, .F. ) ;
#88966 = CARTESIAN_POINT ( 'NONE',  ( 0.03625801282051022839, -6.376774720514410077, 19.27714342948718240 ) ) ;
#88967 = CARTESIAN_POINT ( 'NONE',  ( 8.159923944583882260, -6.376774720514430506, -28.14238247108524149 ) ) ;
#88968 = CARTESIAN_POINT ( 'NONE',  ( -14.80784184970232431, -14.63167926507950689, 11.49999999999999645 ) ) ;
#88969 = PLANE ( 'NONE',  #33794 ) ;
#88970 = AXIS2_PLACEMENT_3D ( 'NONE', #60769, #29302, #91199 ) ;
#88971 = EDGE_CURVE ( 'NONE', #69148, #90732, #35017, .T. ) ;
#88972 = CARTESIAN_POINT ( 'NONE',  ( -51.29687923781917647, -25.26364009307625125, 3.993462176398971497 ) ) ;
#88973 = B_SPLINE_CURVE_WITH_KNOTS ( 'NONE', 3,
 ( #54845, #38605, #542, #47227, #69565, #43, #77654, #30989, #85786, #39605, #8663, #93892 ),
 .UNSPECIFIED., .F., .F.,
 ( 4, 2, 2, 2, 2, 4 ),
 ( 0.000000000000000000, 0.0003366851721765631335, 0.0006733703443531262670, 0.001010055516529689400, 0.001178398102617971618, 0.001346740688706254052 ),
 .UNSPECIFIED. ) ;
#88974 = VERTEX_POINT ( 'NONE', #65464 ) ;
#88975 = LINE ( 'NONE', #64664, #36562 ) ;
#88976 = CARTESIAN_POINT ( 'NONE',  ( -127.6240570866291080, -24.15543982623907837, -0.2315651400026538520 ) ) ;
#88977 = ORIENTED_EDGE ( 'NONE', *, *, #56102, .F. ) ;
#88978 = VECTOR ( 'NONE', #53677, 1000.000000000000114 ) ;
#88979 = CARTESIAN_POINT ( 'NONE',  ( 18.82617747125253871, -7.458514806974097411, 11.49999999999998934 ) ) ;
#88980 = DIRECTION ( 'NONE',  ( 0.000000000000000000, -1.000000000000000000, 0.000000000000000000 ) ) ;
#88981 = DIRECTION ( 'NONE',  ( 3.773278334444166432E-23, -1.000000000000000000, 0.000000000000000000 ) ) ;
#88982 = FACE_OUTER_BOUND ( 'NONE', #59404, .T. ) ;
#88983 = ORIENTED_EDGE ( 'NONE', *, *, #18898, .F. ) ;
#88984 = LINE ( 'NONE', #73261, #61433 ) ;
#88985 = DIRECTION ( 'NONE',  ( -0.000000000000000000, 1.000000000000000000, -0.000000000000000000 ) ) ;
#88986 = CARTESIAN_POINT ( 'NONE',  ( -16.95507112718987486, -10.73317591066004084, -1.500000000000002220 ) ) ;
#88987 = CARTESIAN_POINT ( 'NONE',  ( -7.324709186033012465, -19.69651249574825513, 11.49999999999999645 ) ) ;
#88988 = CARTESIAN_POINT ( 'NONE',  ( 6.303825520940272042, 5.965225279485572685, -28.39893233836329856 ) ) ;
#88989 = CARTESIAN_POINT ( 'NONE',  ( 27.53860345374771867, -1.477225279485574028, -9.482392034746240483 ) ) ;
#88990 = CARTESIAN_POINT ( 'NONE',  ( -4.445301477617020325, 21.63612927058290936, 11.49999999999998934 ) ) ;
#88991 = CARTESIAN_POINT ( 'NONE',  ( -39.71177198204633640, -25.27806050189757059, 4.822383089495585473 ) ) ;
#88992 = AXIS2_PLACEMENT_3D ( 'NONE', #17557, #9438, #17051 ) ;
#88993 = DIRECTION ( 'NONE',  ( -1.000000000000000000, -0.000000000000000000, -0.000000000000000000 ) ) ;
#88994 = CARTESIAN_POINT ( 'NONE',  ( -2.794871794871791604, -6.376774720514427841, 21.75000000000001066 ) ) ;
#88995 = CARTESIAN_POINT ( 'NONE',  ( -2.701720430790311767, 5.965225279485594001, -28.90526747363640681 ) ) ;
#88996 = CARTESIAN_POINT ( 'NONE',  ( -10.54059822343757702, -5.876774720514426953, 17.17691942396159988 ) ) ;
#88997 = EDGE_LOOP ( 'NONE', ( #39572, #50888, #78885, #48095 ) ) ;
#88998 = ORIENTED_EDGE ( 'NONE', *, *, #15628, .F. ) ;
#88999 = CARTESIAN_POINT ( 'NONE',  ( -41.55620429048340014, -23.48786465467240347, 11.44779295918254824 ) ) ;
#89000 = CARTESIAN_POINT ( 'NONE',  ( -72.55620429048340725, -23.48786465467240703, 11.44779295918254647 ) ) ;
#89001 = DIRECTION ( 'NONE',  ( 0.000000000000000000, 0.000000000000000000, -1.000000000000000000 ) ) ;
#89002 = CARTESIAN_POINT ( 'NONE',  ( 20.46650637700042097, -2.330123182410055893, -1.500000000000002220 ) ) ;
#89003 = CARTESIAN_POINT ( 'NONE',  ( 15.50980990363467882, 14.95361599516425244, 11.49999999999999645 ) ) ;
#89004 = VERTEX_POINT ( 'NONE', #55335 ) ;
#89005 = CARTESIAN_POINT ( 'NONE',  ( 32.33217928425145971, 1.682774720514426114, -12.20610769812826923 ) ) ;
#89006 = DIRECTION ( 'NONE',  ( -1.000000000000000000, 0.000000000000000000, -0.000000000000000000 ) ) ;
#89007 = DIRECTION ( 'NONE',  ( -0.000000000000000000, 1.000000000000000000, -0.000000000000000000 ) ) ;
#89008 = CARTESIAN_POINT ( 'NONE',  ( 7.190675130926929448, -21.12231643677837312, -1.500000000000002220 ) ) ;
#89009 = B_SPLINE_CURVE_WITH_KNOTS ( 'NONE', 3,
 ( #31668, #62638, #93557, #70741, #81850, #4732 ),
 .UNSPECIFIED., .F., .F.,
 ( 4, 2, 4 ),
 ( 0.000000000000000000, 0.001380764517853252720, 0.002761529035706505441 ),
 .UNSPECIFIED. ) ;
#89010 = CARTESIAN_POINT ( 'NONE',  ( -59.62287095715004881, -24.66019654487199020, 8.947790411086131712 ) ) ;
#89011 = CARTESIAN_POINT ( 'NONE',  ( -52.62287095715005592, -29.50248528299804818, 1.056150453629033370 ) ) ;
#89012 = ORIENTED_EDGE ( 'NONE', *, *, #57798, .T. ) ;
#89013 = DIRECTION ( 'NONE',  ( 0.000000000000000000, -0.9999999999976377785, -2.173523156925979975E-06 ) ) ;
#89014 = CARTESIAN_POINT ( 'NONE',  ( -83.62287095715007013, -24.65952944569304606, 1.056160979905700792 ) ) ;
#89015 = CARTESIAN_POINT ( 'NONE',  ( 16.20321855003292555, -13.12800272717607619, -1.500000000000002220 ) ) ;
#89016 = ORIENTED_EDGE ( 'NONE', *, *, #30425, .F. ) ;
#89017 = EDGE_CURVE ( 'NONE', #8499, #66329, #25938, .T. ) ;
#89019 = ORIENTED_EDGE ( 'NONE', *, *, #94899, .T. ) ;
#89018 = CARTESIAN_POINT ( 'NONE',  ( 15.10352928271630724, -2.682774720514426559, -27.29968155418892195 ) ) ;
#89020 = VERTEX_POINT ( 'NONE', #56844 ) ;
#89021 = CARTESIAN_POINT ( 'NONE',  ( -51.23552013759741897, -25.28256784800020895, 4.253308875550592560 ) ) ;
#89022 = CARTESIAN_POINT ( 'NONE',  ( -6.845587600281468177, 19.88882266644084496, -1.500000000000002220 ) ) ;
#89023 = ADVANCED_FACE ( 'NONE', ( #32482 ), #79149, .F. ) ;
#89024 = ORIENTED_EDGE ( 'NONE', *, *, #49348, .F. ) ;
#89025 = CARTESIAN_POINT ( 'NONE',  ( -114.5895376238167245, -23.48783264082478794, -1.443836473390060382 ) ) ;
#89026 = CARTESIAN_POINT ( 'NONE',  ( 13.57151214508650305, -9.529487854913506695, 0.000000000000000000 ) ) ;
#89027 = CARTESIAN_POINT ( 'NONE',  ( -120.5901044843091938, -24.40133493613049964, 9.663955038902800609 ) ) ;
#89028 = VECTOR ( 'NONE', #20945, 1000.000000000000000 ) ;
#89029 = CARTESIAN_POINT ( 'NONE',  ( -81.11504936654542064, -25.25841645967507887, 3.692618488369098895 ) ) ;
#89030 = CARTESIAN_POINT ( 'NONE',  ( -49.75955460286667176, -25.13461921803880728, 2.970022368781424671 ) ) ;
#89031 = CARTESIAN_POINT ( 'NONE',  ( -13.51661872714272405, -17.00040112538478709, -1.500000000000002220 ) ) ;
#89032 = CARTESIAN_POINT ( 'NONE',  ( -81.47155790579010670, -25.24759638701540254, 6.336855562226338279 ) ) ;
#89034 = VERTEX_POINT ( 'NONE', #41107 ) ;
#89033 = CARTESIAN_POINT ( 'NONE',  ( 19.22371909900314435, 11.20011194808016342, 11.49999999999999645 ) ) ;
#89035 = DIRECTION ( 'NONE',  ( -1.000000000000000000, 0.000000000000000000, 0.000000000000000000 ) ) ;
#89036 = CARTESIAN_POINT ( 'NONE',  ( 19.24418710706453339, -0.5000000000000000000, -2.153101996372891236 ) ) ;
#89037 = ORIENTED_EDGE ( 'NONE', *, *, #39707, .F. ) ;
#89038 = VECTOR ( 'NONE', #39086, 1000.000000000000114 ) ;
#89040 = ORIENTED_EDGE ( 'NONE', *, *, #81373, .T. ) ;
#89039 = CARTESIAN_POINT ( 'NONE',  ( -35.92287095715006018, -23.47596703998600276, 11.44779298504227683 ) ) ;
#89041 = CIRCLE ( 'NONE', #81143, 1.000000000000000888 ) ;
#89042 = ORIENTED_EDGE ( 'NONE', *, *, #34067, .T. ) ;
#89043 = CARTESIAN_POINT ( 'NONE',  ( -75.52287095715007581, -24.63287334234179227, 0.9662140553045428515 ) ) ;
#89045 = EDGE_CURVE ( 'NONE', #20987, #92149, #49588, .T. ) ;
#89044 = CC_DESIGN_DATE_AND_TIME_ASSIGNMENT ( #54380, #84310, ( #21497 ) ) ;
#89046 = CARTESIAN_POINT ( 'NONE',  ( -43.62287095715006302, -24.50321055353804311, 9.387540953477532923 ) ) ;
#89047 = VECTOR ( 'NONE', #16496, 1000.000000000000000 ) ;
#89048 = FACE_OUTER_BOUND ( 'NONE', #77007, .T. ) ;
#89049 = B_SPLINE_CURVE_WITH_KNOTS ( 'NONE', 3,
 ( #25657, #27166, #73343, #35284, #11932, #42897, #65746 ),
 .UNSPECIFIED., .F., .F.,
 ( 4, 1, 1, 1, 4 ),
 ( 0.3452202732246780759, 0.4949101844912719983, 0.6446000957578658097, 0.7942900070244596211, 0.9439799182910535436 ),
 .UNSPECIFIED. ) ;
#89050 = CARTESIAN_POINT ( 'NONE',  ( -83.92287095715009571, -23.47596703998600631, 11.44779298504227860 ) ) ;
#89051 = ORIENTED_EDGE ( 'NONE', *, *, #89279, .F. ) ;
#89052 = CARTESIAN_POINT ( 'NONE',  ( -130.5728709571500588, -24.33102551592700991, -0.06126342234013575083 ) ) ;
#89053 = CARTESIAN_POINT ( 'NONE',  ( -22.33494257564923302, 2.542849975942539587, -1.500000000000002220 ) ) ;
#89054 = ORIENTED_EDGE ( 'NONE', *, *, #89465, .T. ) ;
#89055 = PLANE ( 'NONE',  #67678 ) ;
#89056 = CARTESIAN_POINT ( 'NONE',  ( -94.63996189396370085, -23.48786465467241413, 11.44779295918254469 ) ) ;
#89057 = CARTESIAN_POINT ( 'NONE',  ( 5.659515148182856947, 5.356774720518939326, -27.47062408582486270 ) ) ;
#89058 = CARTESIAN_POINT ( 'NONE',  ( 32.16024265030974050, 0.3587747205144265483, 16.27760796525321751 ) ) ;
#89059 = CARTESIAN_POINT ( 'NONE',  ( -63.92295340422755601, -24.66513809378596278, 8.909134979017297340 ) ) ;
#89060 = CARTESIAN_POINT ( 'NONE',  ( -9.247272915838292917, -17.29429475886123768, -1.500000000000002220 ) ) ;
#89061 = LINE ( 'NONE', #11430, #26408 ) ;
#89062 = ORIENTED_EDGE ( 'NONE', *, *, #79840, .F. ) ;
#89063 = CARTESIAN_POINT ( 'NONE',  ( -20.49900048275977227, -6.559984590058941301, -1.500000000000002220 ) ) ;
#89064 = CARTESIAN_POINT ( 'NONE',  ( 15.98182857103851795, -3.492575169077971609, -27.92678846288758976 ) ) ;
#89065 = CARTESIAN_POINT ( 'NONE',  ( -42.52287095715005449, -24.66019654487199020, 8.947790411086133489 ) ) ;
#89066 = CARTESIAN_POINT ( 'NONE',  ( -101.7776484685884100, -25.27307239909451653, 3.986250617436227550 ) ) ;
#89067 = CARTESIAN_POINT ( 'NONE',  ( -70.62287095715005592, -29.50248789122583659, 2.256150453626215580 ) ) ;
#89068 = CARTESIAN_POINT ( 'NONE',  ( -16.20615075098634961, 16.30094363606528418, -1.500000000000002220 ) ) ;
#89069 = PERSON_AND_ORGANIZATION_ROLE ( 'classification_officer' ) ;
#89070 = DIRECTION ( 'NONE',  ( 0.9685340172660599212, 0.000000000000000000, -0.2488812114211667037 ) ) ;
#89071 = PLANE ( 'NONE',  #63666 ) ;
#89072 = CARTESIAN_POINT ( 'NONE',  ( -19.96166555454951208, -2.086822695551191043, 11.49999999999999645 ) ) ;
#89073 = CARTESIAN_POINT ( 'NONE',  ( -68.52287095715006160, -23.47596703998600631, 11.44779298504228748 ) ) ;
#89074 = CARTESIAN_POINT ( 'NONE',  ( -9.940598223437573822, -6.376774720514426953, 21.78128695274315874 ) ) ;
#89075 = DIRECTION ( 'NONE',  ( 0.06975647374412546897, 0.9975640502598241977, 4.700301109882543835E-17 ) ) ;
#89076 = DIRECTION ( 'NONE',  ( 0.7512896232465891000, -0.000000000000000000, 0.6599726524652351767 ) ) ;
#89077 = CARTESIAN_POINT ( 'NONE',  ( -82.52287095715003318, -24.33927499327855770, 9.819080762295817166 ) ) ;
#89078 = CARTESIAN_POINT ( 'NONE',  ( -1.214729172165279092, -19.82145330704504360, -1.500000000000002220 ) ) ;
#89079 = EDGE_CURVE ( 'NONE', #12723, #47977, #58330, .T. ) ;
#89080 = CARTESIAN_POINT ( 'NONE',  ( -113.6281192877314368, -23.96119346886881374, -0.6495511937832029181 ) ) ;
#89081 = CARTESIAN_POINT ( 'NONE',  ( -0.8432318219891272726, -19.69000482574202238, -1.500000000000002220 ) ) ;
#89082 = CARTESIAN_POINT ( 'NONE',  ( -91.94687923781918926, -25.23397913219354649, 6.409327625488847602 ) ) ;
#89083 = SECURITY_CLASSIFICATION_LEVEL ( 'unclassified' ) ;
#89084 = EDGE_CURVE ( 'NONE', #39801, #62532, #90720, .T. ) ;
#89085 = CARTESIAN_POINT ( 'NONE',  ( -123.5228709571500616, -24.64965694238408034, 8.947790433994191162 ) ) ;
#89086 = PLANE ( 'NONE',  #23218 ) ;
#89087 = CARTESIAN_POINT ( 'NONE',  ( 0.06016934085327452914, 20.63536315578604174, 11.49999999999999645 ) ) ;
#89088 = EDGE_CURVE ( 'NONE', #28802, #149, #14558, .T. ) ;
#89089 = CIRCLE ( 'NONE', #16139, 1.399999999999999911 ) ;
#89090 = CARTESIAN_POINT ( 'NONE',  ( -33.52287095715006160, -23.47596703998600631, 11.44779298504229459 ) ) ;
#89091 = CARTESIAN_POINT ( 'NONE',  ( 14.05383982582471170, -17.77673030755399708, 11.49999999999999645 ) ) ;
#89092 = EDGE_LOOP ( 'NONE', ( #90845, #96088 ) ) ;
#89093 = DIRECTION ( 'NONE',  ( 3.773278334444166432E-23, -1.000000000000000000, 0.000000000000000000 ) ) ;
#89094 = CARTESIAN_POINT ( 'NONE',  ( -39.52287095715006870, -29.50250243563736774, 8.947779886222148704 ) ) ;
#89095 = CIRCLE ( 'NONE', #22569, 28.96799999999999287 ) ;
#89096 = EDGE_CURVE ( 'NONE', #3302, #24683, #21003, .T. ) ;
#89097 = CARTESIAN_POINT ( 'NONE',  ( -127.5228709571500616, -24.64965694238408034, 8.947790433994189385 ) ) ;
#89098 = CARTESIAN_POINT ( 'NONE',  ( -2.532641601674031850, -6.376774720514410077, 19.55266968305501507 ) ) ;
#89099 = AXIS2_PLACEMENT_3D ( 'NONE', #63592, #7777, #85903 ) ;
#89100 = ORIENTED_EDGE ( 'NONE', *, *, #3857, .T. ) ;
#89101 = B_SPLINE_CURVE_WITH_KNOTS ( 'NONE', 3,
 ( #1281, #56576, #24595, #86004 ),
 .UNSPECIFIED., .F., .F.,
 ( 4, 4 ),
 ( 0.000000000000000000, 9.999999999998897304E-05 ),
 .UNSPECIFIED. ) ;
#89102 = EDGE_LOOP ( 'NONE', ( #98786, #18104, #26803, #59097 ) ) ;
#89103 = CYLINDRICAL_SURFACE ( 'NONE', #20917, 1.249999999999997558 ) ;
#89104 = CARTESIAN_POINT ( 'NONE',  ( -11.09240565882118368, -20.00103931635436538, 11.49999999999998934 ) ) ;
#89105 = LINE ( 'NONE', #41944, #45441 ) ;
#89106 = CIRCLE ( 'NONE', #17831, 6.594667762285749468 ) ;
#89107 = CARTESIAN_POINT ( 'NONE',  ( -18.50814150397365410, 11.09706937414969374, -1.500000000000002220 ) ) ;
#89108 = DIRECTION ( 'NONE',  ( -0.000000000000000000, -1.000000000000000000, 0.000000000000000000 ) ) ;
#89109 = PLANE ( 'NONE',  #35505 ) ;
#89110 = CARTESIAN_POINT ( 'NONE',  ( 22.42242567092132433, 2.420433022335332751, 11.49999999999999645 ) ) ;
#89111 = VERTEX_POINT ( 'NONE', #19739 ) ;
#89112 = VECTOR ( 'NONE', #12345, 1000.000000000000114 ) ;
#89113 = PLANE ( 'NONE',  #70796 ) ;
#89114 = CARTESIAN_POINT ( 'NONE',  ( 20.57779966680088890, -7.652443150423321683, 11.49999999999998934 ) ) ;
#89116 = CARTESIAN_POINT ( 'NONE',  ( -10.54059822343757702, -5.876774720514426953, 17.17691942396159988 ) ) ;
#89115 = VECTOR ( 'NONE', #81432, 1000.000000000000000 ) ;
#89117 = DIRECTION ( 'NONE',  ( -3.773278334453079030E-23, 0.9999999999976377785, 2.173523156925979128E-06 ) ) ;
#89118 = ORIENTED_EDGE ( 'NONE', *, *, #23300, .T. ) ;
#89119 = CARTESIAN_POINT ( 'NONE',  ( -112.6228709571500559, -29.50250243563736774, 8.947779886222136270 ) ) ;
#89120 = CARTESIAN_POINT ( 'NONE',  ( -47.58953762381673158, -23.47596703998600276, 11.44779298504227505 ) ) ;
#89121 = VERTEX_POINT ( 'NONE', #74539 ) ;
#89122 = CARTESIAN_POINT ( 'NONE',  ( -77.62287095715005592, -23.47593901973091235, -1.443836447539004642 ) ) ;
#89123 = EDGE_LOOP ( 'NONE', ( #60667, #48713, #24253, #85229 ) ) ;
#89124 = VERTEX_POINT ( 'NONE', #66465 ) ;
#89125 = ORIENTED_EDGE ( 'NONE', *, *, #60213, .T. ) ;
#89126 = CARTESIAN_POINT ( 'NONE',  ( -126.5228709571500616, -23.47593901973090524, -1.443836447538996204 ) ) ;
#89127 = PLANE ( 'NONE',  #27592 ) ;
#89128 = FACE_OUTER_BOUND ( 'NONE', #39186, .T. ) ;
#89129 = CARTESIAN_POINT ( 'NONE',  ( 19.36038471569032993, -6.267470172042458820, -1.500000000000002220 ) ) ;
#89130 = VERTEX_POINT ( 'NONE', #97865 ) ;
#89131 = CARTESIAN_POINT ( 'NONE',  ( -70.70154144008259323, -25.04161745251516180, 7.522173495007288047 ) ) ;
#89132 = CARTESIAN_POINT ( 'NONE',  ( -29.64366785207624488, -24.08068896706512163, 10.23563548314527338 ) ) ;
#89133 = ADVANCED_FACE ( 'NONE', ( #75524 ), #29917, .T. ) ;
#89134 = CARTESIAN_POINT ( 'NONE',  ( -89.40841769935767047, -25.11033443737731474, 2.832404817301930056 ) ) ;
#89135 = CARTESIAN_POINT ( 'NONE',  ( -71.43409008949743111, -25.03149735735439307, 7.038381313596293154 ) ) ;
#89136 = ORIENTED_EDGE ( 'NONE', *, *, #64222, .F. ) ;
#89137 = CARTESIAN_POINT ( 'NONE',  ( -28.29914910988898669, -24.76880887354685612, 2.427551041383773978 ) ) ;
#89138 = B_SPLINE_CURVE_WITH_KNOTS ( 'NONE', 3,
 ( #17630, #33347, #80029, #49597, #81539, #35366 ),
 .UNSPECIFIED., .F., .F.,
 ( 4, 2, 4 ),
 ( 6.391158118969316353E-06, 0.001387004593080787881, 0.002767618028042606766 ),
 .UNSPECIFIED. ) ;
#89139 = DIRECTION ( 'NONE',  ( 3.773278334444166432E-23, -1.000000000000000000, 0.000000000000000000 ) ) ;
#89140 = EDGE_LOOP ( 'NONE', ( #56126, #73935, #100061, #59153, #84766 ) ) ;
#89141 = CARTESIAN_POINT ( 'NONE',  ( 1.212613378922696050, -20.72488358683818888, -1.500000000000002220 ) ) ;
#89143 = EDGE_CURVE ( 'NONE', #64045, #42245, #88782, .T. ) ;
#89142 = ORIENTED_EDGE ( 'NONE', *, *, #92375, .F. ) ;
#89145 = EDGE_LOOP ( 'NONE', ( #21772, #89467, #16855, #93841 ) ) ;
#89144 = FACE_OUTER_BOUND ( 'NONE', #57704, .T. ) ;
#89146 = CARTESIAN_POINT ( 'NONE',  ( -86.62287095715004170, -24.51283580621364067, 0.6167428607019888043 ) ) ;
#89147 = DIRECTION ( 'NONE',  ( 0.000000000000000000, 0.000000000000000000, -1.000000000000000000 ) ) ;
#89148 = VERTEX_POINT ( 'NONE', #12637 ) ;
#89149 = ORIENTED_EDGE ( 'NONE', *, *, #15234, .F. ) ;
#89150 = DIRECTION ( 'NONE',  ( -0.000000000000000000, 1.000000000000000000, -0.000000000000000000 ) ) ;
#89151 = LINE ( 'NONE', #12017, #12490 ) ;
#89152 = CARTESIAN_POINT ( 'NONE',  ( -52.62287095715005592, -23.48786465467240703, 11.44779295918255002 ) ) ;
#89153 = CARTESIAN_POINT ( 'NONE',  ( -43.61624872165830880, -23.48786465467240347, 11.44779295918255180 ) ) ;
#89155 = ORIENTED_EDGE ( 'NONE', *, *, #84338, .F. ) ;
#89154 = CARTESIAN_POINT ( 'NONE',  ( 18.22792733936863030, -12.41963300964812156, 11.49999999999999645 ) ) ;
#89156 = CARTESIAN_POINT ( 'NONE',  ( -108.6294904440730136, -23.96119346886881374, -0.6495511937831862648 ) ) ;
#89157 = CARTESIAN_POINT ( 'NONE',  ( 19.70651319644445465, -11.07993823016455792, 11.49999999999998934 ) ) ;
#89159 = ORIENTED_EDGE ( 'NONE', *, *, #98689, .T. ) ;
#89158 = CARTESIAN_POINT ( 'NONE',  ( -115.5516328901577197, -24.73531770709096023, 8.716586749053508498 ) ) ;
#89160 = EDGE_LOOP ( 'NONE', ( #49995, #14730, #48440, #86052 ) ) ;
#89161 = LINE ( 'NONE', #58221, #27234 ) ;
#89162 = AXIS2_PLACEMENT_3D ( 'NONE', #13979, #75879, #73897 ) ;
#89163 = CC_DESIGN_PERSON_AND_ORGANIZATION_ASSIGNMENT ( #5320, #97178, ( #63584 ) ) ;
#89164 = B_SPLINE_CURVE_WITH_KNOTS ( 'NONE', 3,
 ( #18883, #80290, #87908, #72688, #19875, #19383, #80796, #81789 ),
 .UNSPECIFIED., .F., .F.,
 ( 4, 2, 2, 4 ),
 ( 0.000000000000000000, 0.002001098010032688421, 0.003001647015049031114, 0.004002196020065373373 ),
 .UNSPECIFIED. ) ;
#89165 = CARTESIAN_POINT ( 'NONE',  ( -57.58282881803972231, -24.51419770103157347, 9.386484678747176957 ) ) ;
#89166 = ORIENTED_EDGE ( 'NONE', *, *, #769, .T. ) ;
#89167 = CARTESIAN_POINT ( 'NONE',  ( 12.09327641706010326, 17.40255341615222306, -1.500000000000002220 ) ) ;
#89168 = AXIS2_PLACEMENT_3D ( 'NONE', #80884, #36208, #98082 ) ;
#89169 = CARTESIAN_POINT ( 'NONE',  ( 32.98210467718394767, 3.587965230352024193, -12.99284425914657604 ) ) ;
#89170 = CARTESIAN_POINT ( 'NONE',  ( -41.86766821746776657, -25.28562906917319353, 4.300397852270189780 ) ) ;
#89171 = CARTESIAN_POINT ( 'NONE',  ( -13.70410651198969809, -17.55484038775568933, -1.500000000000002220 ) ) ;
#89172 = LINE ( 'NONE', #50117, #41963 ) ;
#89173 = B_SPLINE_CURVE_WITH_KNOTS ( 'NONE', 3,
 ( #1486, #79085, #77579, #32425, #62897, #63397, #8589, #33417, #39033, #1986, #71499, #39538, #9587, #79594, #69982, #94818 ),
 .UNSPECIFIED., .F., .F.,
 ( 4, 2, 2, 2, 2, 2, 2, 4 ),
 ( 0.000000000000000000, 0.0003118384806944565074, 0.0006236769613889130148, 0.001247353922777823428, 0.001559192403472278851, 0.001871030884166734057, 0.002182869364861189480, 0.002494707845555644687 ),
 .UNSPECIFIED. ) ;
#89174 = ORIENTED_EDGE ( 'NONE', *, *, #67886, .T. ) ;
#89175 = CARTESIAN_POINT ( 'NONE',  ( -54.52287095715006870, -24.65952944569304606, 1.056160979905693686 ) ) ;
#89176 = CARTESIAN_POINT ( 'NONE',  ( 28.30015606816038698, 2.682774720514426559, -13.13501953239208575 ) ) ;
#89177 = EDGE_CURVE ( 'NONE', #17220, #77901, #8411, .T. ) ;
#89178 = CARTESIAN_POINT ( 'NONE',  ( -10.34999999999997833, 27.69999999999999929, 2.100000000000000089 ) ) ;
#89179 = CARTESIAN_POINT ( 'NONE',  ( 5.202077965628057576, -2.038091937962834166, -2.869745073849994963E-16 ) ) ;
#89180 = VECTOR ( 'NONE', #50115, 1000.000000000000114 ) ;
#89181 = CARTESIAN_POINT ( 'NONE',  ( -17.64752530894654470, 8.349842952099315596, -1.500000000000002220 ) ) ;
#89182 = VECTOR ( 'NONE', #17588, 1000.000000000000000 ) ;
#89183 = CARTESIAN_POINT ( 'NONE',  ( 18.29419249859179786, 11.19154738541161365, 11.49999999999998934 ) ) ;
#89184 = CARTESIAN_POINT ( 'NONE',  ( -27.40838375831408058, -24.92774670570336326, 1.648156544774445731 ) ) ;
#89185 = B_SPLINE_CURVE_WITH_KNOTS ( 'NONE', 3,
 ( #38434, #45561, #21199, #83599, #37441, #99807 ),
 .UNSPECIFIED., .F., .F.,
 ( 4, 2, 4 ),
 ( 1.570755371633875854E-05, 0.001396183895866086452, 0.002776660238015833844 ),
 .UNSPECIFIED. ) ;
#89186 = CARTESIAN_POINT ( 'NONE',  ( -24.90875734969025501, -6.475225279485573360, 26.43402280011862615 ) ) ;
#89187 = CARTESIAN_POINT ( 'NONE',  ( -77.52212617553594498, -23.48783264082476663, -1.443836473390097241 ) ) ;
#89188 = CARTESIAN_POINT ( 'NONE',  ( -22.76716317511769461, -1.676022972194794791, -1.500000000000002220 ) ) ;
#89189 = VECTOR ( 'NONE', #70071, 1000.000000000000000 ) ;
#89190 =( NAMED_UNIT ( * ) SI_UNIT ( $, .STERADIAN. ) SOLID_ANGLE_UNIT ( ) );
#89191 = DIRECTION ( 'NONE',  ( -0.000000000000000000, -0.000000000000000000, -1.000000000000000000 ) ) ;
#89192 = DIRECTION ( 'NONE',  ( -0.000000000000000000, -1.000000000000000000, 0.000000000000000000 ) ) ;
#89193 = CARTESIAN_POINT ( 'NONE',  ( 19.80199147212610811, 2.383747631481649254, 11.49999999999999645 ) ) ;
#89194 = CARTESIAN_POINT ( 'NONE',  ( -31.52287095715006160, -24.64898659630367206, 1.056161002820817485 ) ) ;
#89195 = CARTESIAN_POINT ( 'NONE',  ( -7.160000000000000142, 8.793627758918228565, -2.994553991265763049 ) ) ;
#89196 = CARTESIAN_POINT ( 'NONE',  ( -48.48463779374034743, -24.65952944569304606, 1.056160979905697461 ) ) ;
#89197 = EDGE_CURVE ( 'NONE', #62610, #38959, #48308, .T. ) ;
#89198 = ORIENTED_EDGE ( 'NONE', *, *, #47058, .T. ) ;
#89199 = DIRECTION ( 'NONE',  ( 0.000000000000000000, 0.9999999999976377785, 2.173523156925979975E-06 ) ) ;
#89200 = CARTESIAN_POINT ( 'NONE',  ( -33.00286163603178125, -25.16202561908117730, 2.791798636425737445 ) ) ;
#89201 = CARTESIAN_POINT ( 'NONE',  ( 21.21565077533257337, 4.556159429511043690, 11.49999999999998934 ) ) ;
#89202 = CARTESIAN_POINT ( 'NONE',  ( -84.52287095715010423, -24.35013146730203815, 9.818937971375104823 ) ) ;
#89203 = CARTESIAN_POINT ( 'NONE',  ( 19.26631176993168282, 3.279242639417544236, -1.500000000000002220 ) ) ;
#89204 = LINE ( 'NONE', #80088, #39336 ) ;
#89205 = B_SPLINE_CURVE_WITH_KNOTS ( 'NONE', 3,
 ( #49293, #19311, #17824, #80726, #58399, #48280 ),
 .UNSPECIFIED., .F., .F.,
 ( 4, 2, 4 ),
 ( 0.000000000000000000, 0.001380901958385389195, 0.002761803916770778390 ),
 .UNSPECIFIED. ) ;
#89206 = PERSON_AND_ORGANIZATION_ROLE ( 'classification_officer' ) ;
#89207 = ADVANCED_FACE ( 'NONE', ( #73550 ), #4042, .F. ) ;
#89208 = CARTESIAN_POINT ( 'NONE',  ( -51.58953762381672448, -24.66019654487199020, 8.947790411086131712 ) ) ;
#89209 = CARTESIAN_POINT ( 'NONE',  ( -18.16121111207539940, 9.348575961806686152, 11.49999999999999645 ) ) ;
#89210 = CARTESIAN_POINT ( 'NONE',  ( -50.31093898778911466, -25.30399390996193532, 5.199283961936068899 ) ) ;
#89211 = EDGE_CURVE ( 'NONE', #61226, #74791, #81027, .T. ) ;
#89212 = CARTESIAN_POINT ( 'NONE',  ( -89.52287095715007581, -24.50216790748204687, 0.6166512839542543922 ) ) ;
#89213 = ORIENTED_EDGE ( 'NONE', *, *, #89894, .F. ) ;
#89214 = DIRECTION ( 'NONE',  ( -1.000000000000000000, -0.000000000000000000, -0.000000000000000000 ) ) ;
#89215 = CARTESIAN_POINT ( 'NONE',  ( -49.21454750704995007, -29.50249835244419927, 7.069174116995804447 ) ) ;
#89216 = LINE ( 'NONE', #32046, #35519 ) ;
#89217 = EDGE_CURVE ( 'NONE', #99833, #89034, #9398, .T. ) ;
#89218 = CARTESIAN_POINT ( 'NONE',  ( -56.22287095715006444, -23.47593901973090169, -1.443836447538997536 ) ) ;
#89219 = ORIENTED_EDGE ( 'NONE', *, *, #9811, .F. ) ;
#89220 = CARTESIAN_POINT ( 'NONE',  ( 5.697397333356354565, -6.376774720514418959, 20.51730809691671809 ) ) ;
#89221 = CARTESIAN_POINT ( 'NONE',  ( 22.99805582222048272, -0.5679727363130141482, 11.49999999999999645 ) ) ;
#89222 = CARTESIAN_POINT ( 'NONE',  ( -22.77908990650604792, -0.06651829912971220227, 11.49999999999998934 ) ) ;
#89223 = CARTESIAN_POINT ( 'NONE',  ( 4.261846905714947731, -6.376774720514427841, 21.73176331363731251 ) ) ;
#89224 = CARTESIAN_POINT ( 'NONE',  ( -40.52287095715005449, -24.99132157543166244, 2.256160258750667502 ) ) ;
#89225 = CARTESIAN_POINT ( 'NONE',  ( 32.66876533700883556, 6.475225279485573360, -12.58926540598386445 ) ) ;
#89226 = CARTESIAN_POINT ( 'NONE',  ( -70.52287095715007581, -23.48783264082477018, -1.443836473390089914 ) ) ;
#89227 = CARTESIAN_POINT ( 'NONE',  ( -110.5598941975710119, -23.48783264082476308, -1.443836473390091468 ) ) ;
#89228 = AXIS2_PLACEMENT_3D ( 'NONE', #24601, #1287, #16486 ) ;
#89229 = CARTESIAN_POINT ( 'NONE',  ( 1.740910633133015972, 21.82039641801506846, -1.500000000000002220 ) ) ;
#89230 = DIRECTION ( 'NONE',  ( -1.000000000000000000, -0.000000000000000000, -0.000000000000000000 ) ) ;
#89231 = DIRECTION ( 'NONE',  ( -3.773278334453080206E-23, 0.9999999999976377785, 2.173523156925979975E-06 ) ) ;
#89232 = FACE_OUTER_BOUND ( 'NONE', #66645, .T. ) ;
#89233 = CARTESIAN_POINT ( 'NONE',  ( 8.971512145086501633, -0.9738200612200850204, 3.736985260579223755 ) ) ;
#89234 = ORIENTED_EDGE ( 'NONE', *, *, #83229, .T. ) ;
#89235 = CARTESIAN_POINT ( 'NONE',  ( -4.163110563111144913, -19.98234244090558320, -1.500000000000002220 ) ) ;
#89236 = ORIENTED_EDGE ( 'NONE', *, *, #60888, .F. ) ;
#89237 = ORIENTED_EDGE ( 'NONE', *, *, #12443, .T. ) ;
#89238 = ORIENTED_EDGE ( 'NONE', *, *, #65954, .T. ) ;
#89239 = ORIENTED_EDGE ( 'NONE', *, *, #2617, .F. ) ;
#89240 = CARTESIAN_POINT ( 'NONE',  ( 22.99805582222048272, -0.5679727363130141482, -1.500000000000002220 ) ) ;
#89241 = LINE ( 'NONE', #74506, #19489 ) ;
#89242 = CARTESIAN_POINT ( 'NONE',  ( 13.23653054071972512, 15.24542462990338088, -1.500000000000002220 ) ) ;
#89243 = ORIENTED_EDGE ( 'NONE', *, *, #3775, .T. ) ;
#89244 = CARTESIAN_POINT ( 'NONE',  ( -113.5228709571501327, -24.66019654487200441, 8.947790411086112172 ) ) ;
#89245 = DIRECTION ( 'NONE',  ( 0.000000000000000000, 0.000000000000000000, 1.000000000000000000 ) ) ;
#89247 = CARTESIAN_POINT ( 'NONE',  ( -73.62287095715005592, -29.50248528299804818, 1.056150453629036701 ) ) ;
#89246 = VECTOR ( 'NONE', #85298, 999.9999999999998863 ) ;
#89248 = DIRECTION ( 'NONE',  ( -1.000000000000000000, -3.491481338843133355E-15, -2.352173255807796056E-16 ) ) ;
#89250 = ORIENTED_EDGE ( 'NONE', *, *, #85761, .F. ) ;
#89249 = CARTESIAN_POINT ( 'NONE',  ( 20.90283063341239966, -4.354886778353011856, 11.49999999999999645 ) ) ;
#89251 = LINE ( 'NONE', #50692, #56524 ) ;
#89252 = AXIS2_PLACEMENT_3D ( 'NONE', #11372, #25086, #64694 ) ;
#89253 = EDGE_LOOP ( 'NONE', ( #13491, #47983, #48255, #33773 ) ) ;
#89254 = CARTESIAN_POINT ( 'NONE',  ( 7.309977242446557888, -21.02818303981469583, -1.500000000000002220 ) ) ;
#89255 = CARTESIAN_POINT ( 'NONE',  ( 9.361532043782798240, 18.45020211870636118, 11.49999999999998934 ) ) ;
#89256 = ORIENTED_EDGE ( 'NONE', *, *, #93522, .T. ) ;
#89257 = EDGE_CURVE ( 'NONE', #60099, #67166, #64794, .T. ) ;
#89258 = LINE ( 'NONE', #88261, #46953 ) ;
#89259 = ORIENTED_EDGE ( 'NONE', *, *, #76160, .T. ) ;
#89260 = CARTESIAN_POINT ( 'NONE',  ( 13.10664265030973930, -1.324225279485583551, -28.18129937516353678 ) ) ;
#89261 = ORIENTED_EDGE ( 'NONE', *, *, #60826, .F. ) ;
#89262 = CARTESIAN_POINT ( 'NONE',  ( 9.422519371942208011, -3.316774720514425567, -27.03574706870085720 ) ) ;
#89263 = CARTESIAN_POINT ( 'NONE',  ( -16.13976855045889636, 13.32451261336467496, -1.500000000000002220 ) ) ;
#89264 = CARTESIAN_POINT ( 'NONE',  ( -8.129759772327192380, 20.32010563749377141, 11.49999999999999645 ) ) ;
#89265 = CARTESIAN_POINT ( 'NONE',  ( -26.33488822642538452, -24.77993562733889732, 6.524122098704422612 ) ) ;
#89266 = CARTESIAN_POINT ( 'NONE',  ( -21.16606679798846358, 7.723709098063864076, -1.500000000000002220 ) ) ;
#89267 = CARTESIAN_POINT ( 'NONE',  ( 20.69369447470243628, -3.267675865747468489, 11.49999999999998934 ) ) ;
#89268 = DIRECTION ( 'NONE',  ( -3.773278334453080206E-23, 0.9999999999976377785, 2.173523156925979552E-06 ) ) ;
#89269 = CARTESIAN_POINT ( 'NONE',  ( 5.817949855437939632, -5.876774720514417183, 20.34349022145623209 ) ) ;
#89270 = CARTESIAN_POINT ( 'NONE',  ( -29.62287095715004881, -24.58457514626677209, 8.947790440257529454 ) ) ;
#89271 = DIRECTION ( 'NONE',  ( -0.06486421869277853025, 0.000000000000000000, 0.9978940991575084851 ) ) ;
#89272 = ORIENTED_EDGE ( 'NONE', *, *, #77697, .T. ) ;
#89273 = EDGE_LOOP ( 'NONE', ( #48820, #46683, #13558, #67996 ) ) ;
#89274 = ORIENTED_EDGE ( 'NONE', *, *, #86421, .T. ) ;
#89275 = B_SPLINE_CURVE_WITH_KNOTS ( 'NONE', 3,
 ( #21867, #43737, #44733, #74670, #36118, #90899, #20879, #82783, #13265, #36611 ),
 .UNSPECIFIED., .F., .F.,
 ( 4, 3, 3, 4 ),
 ( 3.074392035520069841E-15, 0.0001187729392939394833, 0.0002375726806888468626, 0.0004748969025384985692 ),
 .UNSPECIFIED. ) ;
#89276 = B_SPLINE_CURVE_WITH_KNOTS ( 'NONE', 3,
 ( #70105, #53886, #94436, #55900 ),
 .UNSPECIFIED., .F., .F.,
 ( 4, 4 ),
 ( 0.9304503362875529149, 0.9394567675596684486 ),
 .UNSPECIFIED. ) ;
#89277 = CARTESIAN_POINT ( 'NONE',  ( -99.31542661674430406, -25.12215508542761810, 6.334584756663662830 ) ) ;
#89278 = VERTEX_POINT ( 'NONE', #31237 ) ;
#89279 = EDGE_CURVE ( 'NONE', #733, #77757, #78901, .T. ) ;
#89280 = CARTESIAN_POINT ( 'NONE',  ( 12.90647603486358364, 17.18646895862681134, -1.500000000000002220 ) ) ;
#89281 = CARTESIAN_POINT ( 'NONE',  ( -95.62287095715005592, -23.47593901973091235, -1.443836447539001089 ) ) ;
#89282 = VERTEX_POINT ( 'NONE', #39351 ) ;
#89283 = CARTESIAN_POINT ( 'NONE',  ( 14.35337761433406811, 15.45585641580067104, 11.49999999999998934 ) ) ;
#89284 = CARTESIAN_POINT ( 'NONE',  ( 7.160000000000000142, -6.446506136384785535, 8.876977486517731109 ) ) ;
#89285 = CARTESIAN_POINT ( 'NONE',  ( -52.62287095715009144, -24.34917612406838217, 0.1852690917426617345 ) ) ;
#89286 = EDGE_CURVE ( 'NONE', #81354, #97718, #20428, .T. ) ;
#89287 = FACE_OUTER_BOUND ( 'NONE', #88403, .T. ) ;
#89288 = CARTESIAN_POINT ( 'NONE',  ( -101.6270331350176548, -24.34968618360934300, 0.1864209137778871650 ) ) ;
#89289 = DIRECTION ( 'NONE',  ( -1.000000000000000000, 0.000000000000000000, 0.000000000000000000 ) ) ;
#89290 = CARTESIAN_POINT ( 'NONE',  ( 15.76968270297436625, 15.47746201419723100, -1.500000000000002220 ) ) ;
#89291 = ORIENTED_EDGE ( 'NONE', *, *, #66534, .F. ) ;
#89292 = CARTESIAN_POINT ( 'NONE',  ( -81.59191989886164720, -24.15620529776628445, 10.23563542870661180 ) ) ;
#89293 = FACE_OUTER_BOUND ( 'NONE', #57318, .T. ) ;
#89294 = CARTESIAN_POINT ( 'NONE',  ( -41.81544514806834201, -25.31624538345576170, 4.607988139056270249 ) ) ;
#89295 = EDGE_CURVE ( 'NONE', #69268, #74882, #88217, .T. ) ;
#89296 = EDGE_CURVE ( 'NONE', #34878, #40829, #70310, .T. ) ;
#89297 = CARTESIAN_POINT ( 'NONE',  ( -47.52287095715006160, -24.50216790748205042, 0.6166512839542448443 ) ) ;
#89298 = EDGE_CURVE ( 'NONE', #3028, #87115, #24615, .T. ) ;
#89299 = DIRECTION ( 'NONE',  ( -0.06975647374412549673, -0.9975640502598241977, 0.000000000000000000 ) ) ;
#89300 = CARTESIAN_POINT ( 'NONE',  ( 12.49974722350246736, 17.29906535522423638, -1.500000000000002220 ) ) ;
#89301 = CARTESIAN_POINT ( 'NONE',  ( -26.11716922332098534, -24.96254238629463984, 5.477951238729472649 ) ) ;
#89302 = CARTESIAN_POINT ( 'NONE',  ( -49.89395067847572562, -25.03707831087709579, 7.590867751134624974 ) ) ;
#89303 = CIRCLE ( 'NONE', #45557, 28.96799999999999642 ) ;
#89304 = CARTESIAN_POINT ( 'NONE',  ( -64.63157754250315179, -24.35071581493543391, 9.817618358456023486 ) ) ;
#89305 = DIRECTION ( 'NONE',  ( 0.000000000000000000, 0.9999999999976377785, 2.173523156925979128E-06 ) ) ;
#89306 = CARTESIAN_POINT ( 'NONE',  ( -4.753580043990282888, 22.13494492317406070, -1.500000000000002220 ) ) ;
#89307 = CARTESIAN_POINT ( 'NONE',  ( -33.52287095715006160, -23.47596703998600631, 11.44779298504229459 ) ) ;
#89308 = VERTEX_POINT ( 'NONE', #67942 ) ;
#89309 = CARTESIAN_POINT ( 'NONE',  ( -50.72885261542558055, -25.31331831088759188, 5.238457455606527091 ) ) ;
#89310 = PLANE ( 'NONE',  #78357 ) ;
#89311 = CARTESIAN_POINT ( 'NONE',  ( -8.281543130087330340, -17.94227898472161797, 11.49999999999999645 ) ) ;
#89312 = CARTESIAN_POINT ( 'NONE',  ( -82.62287095715004170, -23.47596703998600631, 11.44779298504227860 ) ) ;
#89313 = PLANE ( 'NONE',  #35034 ) ;
#89314 = EDGE_CURVE ( 'NONE', #72281, #68666, #24121, .T. ) ;
#89315 = VERTEX_POINT ( 'NONE', #32234 ) ;
#89316 = DIRECTION ( 'NONE',  ( -1.000000000000000000, -0.000000000000000000, -0.000000000000000000 ) ) ;
#89317 = CARTESIAN_POINT ( 'NONE',  ( -70.52287095715009002, -24.15516710230294350, 10.28746687063725673 ) ) ;
#89318 = CARTESIAN_POINT ( 'NONE',  ( -10.34999999999999254, 3.000000000000000000, 4.499999999999999112 ) ) ;
#89319 = CARTESIAN_POINT ( 'NONE',  ( -13.25059585359799108, -17.08168364658555305, 11.49999999999998934 ) ) ;
#89320 = CARTESIAN_POINT ( 'NONE',  ( 7.160000000000000142, 7.891155995661685019, 5.788828319098143993 ) ) ;
#89321 = CARTESIAN_POINT ( 'NONE',  ( -13.43510958081001050, -13.94331287200543024, -1.500000000000002220 ) ) ;
#89322 = DIRECTION ( 'NONE',  ( -3.773278334444167608E-23, 1.000000000000000000, 0.000000000000000000 ) ) ;
#89323 = LINE ( 'NONE', #95932, #37744 ) ;
#89324 = CARTESIAN_POINT ( 'NONE',  ( -13.31955177964949755, -14.60123061082138385, -1.500000000000002220 ) ) ;
#89325 = VECTOR ( 'NONE', #78434, 1000.000000000000000 ) ;
#89326 = ORIENTED_EDGE ( 'NONE', *, *, #7174, .F. ) ;
#89327 = AXIS2_PLACEMENT_3D ( 'NONE', #72472, #57264, #57751 ) ;
#89328 = CARTESIAN_POINT ( 'NONE',  ( -9.609455416251792670, -17.83980533922896683, 11.49999999999999645 ) ) ;
#89329 = CARTESIAN_POINT ( 'NONE',  ( -54.55620429048340014, -24.66019654487198309, 8.947790411086135265 ) ) ;
#89330 = EDGE_CURVE ( 'NONE', #7606, #16795, #83645, .T. ) ;
#89331 = CARTESIAN_POINT ( 'NONE',  ( -44.52287095715007581, -24.34917612406836795, 0.1852690917426490502 ) ) ;
#89332 = ADVANCED_FACE ( 'NONE', ( #38849 ), #55092, .F. ) ;
#89333 = VERTEX_POINT ( 'NONE', #1301 ) ;
#89334 = CARTESIAN_POINT ( 'NONE',  ( -5.366453405989236813, -14.50000000000000178, 12.73734666247252711 ) ) ;
#89335 = LINE ( 'NONE', #5588, #41251 ) ;
#89336 = CARTESIAN_POINT ( 'NONE',  ( -44.62287095715004881, -24.65952944569303895, 1.056160979905693686 ) ) ;
#89337 = CARTESIAN_POINT ( 'NONE',  ( -32.52287095715006160, -24.64965694238575011, 8.947790433994207149 ) ) ;
#89338 = CARTESIAN_POINT ( 'NONE',  ( -86.62287095715001328, -23.47596703998600631, 11.44779298504227683 ) ) ;
#89339 = CARTESIAN_POINT ( 'NONE',  ( 20.02521558760690112, -0.9251608499524575091, -1.500000000000002220 ) ) ;
#89340 = B_SPLINE_CURVE_WITH_KNOTS ( 'NONE', 3,
 ( #68002, #35557, #44161, #75093, #98932, #27933, #29420, #60402, #91323, #76090, #37543, #68493, #12195, #58890, #21796, #58400 ),
 .UNSPECIFIED., .F., .F.,
 ( 4, 2, 2, 2, 2, 2, 2, 4 ),
 ( 8.673617379884035472E-19, 0.0002012182839424428243, 0.0004024365678848847811, 0.0006036548518273267923, 0.0008048731357697686949, 0.001207309703654670281, 0.001408527987597120749, 0.001609746271539571651 ),
 .UNSPECIFIED. ) ;
#89341 = ADVANCED_FACE ( 'NONE', ( #29359, #76025 ), #54584, .F. ) ;
#89342 = DIRECTION ( 'NONE',  ( 1.000000000000000000, 0.000000000000000000, -0.000000000000000000 ) ) ;
#89343 = ORIENTED_EDGE ( 'NONE', *, *, #58045, .T. ) ;
#89344 = EDGE_CURVE ( 'NONE', #17471, #7644, #60369, .T. ) ;
#89345 = EDGE_CURVE ( 'NONE', #72609, #99097, #8903, .T. ) ;
#89346 = CARTESIAN_POINT ( 'NONE',  ( -103.5228709571501184, -23.96177878511309345, 10.65340807706329507 ) ) ;
#89347 = CARTESIAN_POINT ( 'NONE',  ( -29.62287095715004881, -24.58457514626677209, 8.947790440257529454 ) ) ;
#89348 = CARTESIAN_POINT ( 'NONE',  ( -79.56153920765868293, -25.30148319546968239, 5.323200279246012023 ) ) ;
#89349 = DIRECTION ( 'NONE',  ( 0.000000000000000000, 0.000000000000000000, 1.000000000000000000 ) ) ;
#89350 = CARTESIAN_POINT ( 'NONE',  ( -89.40841769935767047, -25.05712065398430966, 7.447789548358837663 ) ) ;
#89351 = CARTESIAN_POINT ( 'NONE',  ( -50.62287095715005592, -29.50247984919015209, -1.443849546365058689 ) ) ;
#89352 = ORIENTED_EDGE ( 'NONE', *, *, #87000, .F. ) ;
#89353 = CARTESIAN_POINT ( 'NONE',  ( -3.780122020211411193, 19.97858748211865532, 11.49999999999998934 ) ) ;
#89354 = EDGE_LOOP ( 'NONE', ( #75643, #43937, #17626, #76623 ) ) ;
#89355 = CARTESIAN_POINT ( 'NONE',  ( -19.87571804785047647, -11.42512898079034400, -1.500000000000002220 ) ) ;
#89356 = CARTESIAN_POINT ( 'NONE',  ( 29.67519708478274865, 5.974976214603829661, 27.68766025429119537 ) ) ;
#89357 = ORIENTED_EDGE ( 'NONE', *, *, #3861, .F. ) ;
#89358 = DIRECTION ( 'NONE',  ( -1.000000000000000000, -3.773278334444167608E-23, -8.201307833595939069E-29 ) ) ;
#89359 = CARTESIAN_POINT ( 'NONE',  ( -49.27764846858840997, -25.26263970634994749, 6.145204967039955335 ) ) ;
#89360 = CARTESIAN_POINT ( 'NONE',  ( -72.52287095715007581, -23.47593901973090169, -1.443836447538996870 ) ) ;
#89361 = CARTESIAN_POINT ( 'NONE',  ( 18.56724428474754518, 10.22298014144217859, 11.49999999999999645 ) ) ;
#89362 = CARTESIAN_POINT ( 'NONE',  ( 2.574831182292884435, -22.01391258260016315, 11.49999999999998934 ) ) ;
#89363 = AXIS2_PLACEMENT_3D ( 'NONE', #94678, #69851, #1845 ) ;
#89364 = CARTESIAN_POINT ( 'NONE',  ( 11.80677006232881254, 16.86875346446678137, 11.49999999999998934 ) ) ;
#89365 = EDGE_LOOP ( 'NONE', ( #63953, #64732, #82020, #57035, #95105, #84761 ) ) ;
#89366 = PLANE ( 'NONE',  #89577 ) ;
#89367 = ORIENTED_EDGE ( 'NONE', *, *, #32936, .F. ) ;
#89368 = PLANE ( 'NONE',  #23555 ) ;
#89369 = CARTESIAN_POINT ( 'NONE',  ( -50.52287095715007581, -23.84081130425355965, 10.88220057483161263 ) ) ;
#89370 = ORIENTED_EDGE ( 'NONE', *, *, #69473, .F. ) ;
#89371 = ORIENTED_EDGE ( 'NONE', *, *, #88395, .F. ) ;
#89372 = APPLICATION_CONTEXT ( 'configuration controlled 3d designs of mechanical parts and assemblies' ) ;
#89373 = ORIENTED_EDGE ( 'NONE', *, *, #62637, .T. ) ;
#89374 = CARTESIAN_POINT ( 'NONE',  ( -83.62287095715005592, -23.48783264082478794, -1.443836473390065711 ) ) ;
#89375 = CARTESIAN_POINT ( 'NONE',  ( -126.6228709571500559, -29.50248528299804818, 1.056150453629047137 ) ) ;
#89376 = CARTESIAN_POINT ( 'NONE',  ( 14.43441819133292370, -3.316774720514429120, -28.36222020317234183 ) ) ;
#89377 = CARTESIAN_POINT ( 'NONE',  ( 17.70469293622815243, 10.90570606759641592, -1.500000000000002220 ) ) ;
#89378 = CARTESIAN_POINT ( 'NONE',  ( -3.653784360050144286, 21.42803128968991544, 11.49999999999999645 ) ) ;
#89379 = ORIENTED_EDGE ( 'NONE', *, *, #3051, .F. ) ;
#89380 = LINE ( 'NONE', #11748, #77429 ) ;
#89381 = CARTESIAN_POINT ( 'NONE',  ( -119.6228709571501128, -24.51387760970725083, 9.387446482453411178 ) ) ;
#89382 = CARTESIAN_POINT ( 'NONE',  ( 18.78116726530667080, 12.29669497462397842, -1.500000000000002220 ) ) ;
#89383 = DIRECTION ( 'NONE',  ( 0.9980236263794188822, 0.000000000000000000, -0.06283980576413537855 ) ) ;
#89384 = CARTESIAN_POINT ( 'NONE',  ( -65.60613133360229199, -23.85016227208580730, -0.8807180028928343063 ) ) ;
#89385 = ORIENTED_EDGE ( 'NONE', *, *, #49146, .T. ) ;
#89386 = CARTESIAN_POINT ( 'NONE',  ( -75.52287095715007581, -24.51163499207174823, 0.6490370598554360271 ) ) ;
#89387 = CIRCLE ( 'NONE', #87799, 1.306876713926001354 ) ;
#89388 = CARTESIAN_POINT ( 'NONE',  ( -85.55620429048340725, -24.99132157543166954, 2.256160258750668834 ) ) ;
#89389 = LOCAL_TIME ( 0, 54, 15.00000000000000000, #57138 ) ;
#89390 = ORIENTED_EDGE ( 'NONE', *, *, #86593, .F. ) ;
#89391 = ORIENTED_EDGE ( 'NONE', *, *, #23347, .T. ) ;
#89392 = CARTESIAN_POINT ( 'NONE',  ( -46.57703336374709124, -24.66019654487199375, 8.947790411086122830 ) ) ;
#89393 = ORIENTED_EDGE ( 'NONE', *, *, #49918, .T. ) ;
#89394 = EDGE_CURVE ( 'NONE', #31972, #4780, #70812, .T. ) ;
#89395 = CARTESIAN_POINT ( 'NONE',  ( 6.557060941508195739, 20.25493142521265355, -1.500000000000002220 ) ) ;
#89396 = ORIENTED_EDGE ( 'NONE', *, *, #39910, .F. ) ;
#89397 = CARTESIAN_POINT ( 'NONE',  ( -88.58576889810002797, -24.51314013834316086, 0.6176544820404141767 ) ) ;
#89398 = EDGE_CURVE ( 'NONE', #31070, #7198, #84228, .T. ) ;
#89399 = CARTESIAN_POINT ( 'NONE',  ( 21.83365961380331655, 0.8745889840297637052, 11.49999999999998934 ) ) ;
#89400 = CARTESIAN_POINT ( 'NONE',  ( 0.7051282051282083962, -6.376774720514427841, 21.75000000000000000 ) ) ;
#89401 = CARTESIAN_POINT ( 'NONE',  ( 12.08046422559826816, 19.21373320108137861, 11.49999999999998934 ) ) ;
#89402 = CARTESIAN_POINT ( 'NONE',  ( 7.478911390063968767, -6.376774720514422512, 20.82112274756839199 ) ) ;
#89403 = CARTESIAN_POINT ( 'NONE',  ( 5.443272695963705665, -5.876774720514418071, 20.27301970143225418 ) ) ;
#89404 = CARTESIAN_POINT ( 'NONE',  ( -9.857428550561325054, -19.57614489166009264, -1.500000000000002220 ) ) ;
#89405 = CARTESIAN_POINT ( 'NONE',  ( 6.627987042499408510, -5.876774720514423400, 21.45334999081212146 ) ) ;
#89406 = ORIENTED_EDGE ( 'NONE', *, *, #19906, .T. ) ;
#89407 = CARTESIAN_POINT ( 'NONE',  ( -122.5535487218200217, -24.66019654487200086, 8.947790411086110396 ) ) ;
#89408 = CARTESIAN_POINT ( 'NONE',  ( -73.58953762381673869, -24.64898659630367916, 1.056161002820384054 ) ) ;
#89409 = EDGE_CURVE ( 'NONE', #98585, #58202, #45104, .T. ) ;
#89410 = VERTEX_POINT ( 'NONE', #64728 ) ;
#89411 = EDGE_CURVE ( 'NONE', #94830, #57483, #10402, .T. ) ;
#89412 = CARTESIAN_POINT ( 'NONE',  ( -90.62287095715004170, -24.15431212366389957, -0.2830839119429071626 ) ) ;
#89413 = ORIENTED_EDGE ( 'NONE', *, *, #12278, .F. ) ;
#89414 = LINE ( 'NONE', #50861, #18397 ) ;
#89415 = EDGE_CURVE ( 'NONE', #98443, #73818, #57101, .T. ) ;
#89416 = CARTESIAN_POINT ( 'NONE',  ( 14.61581676223891613, 3.316774720514426900, -27.35847991879931485 ) ) ;
#89417 = CARTESIAN_POINT ( 'NONE',  ( 1.567330217057175901, -21.20382687294985047, -1.500000000000002220 ) ) ;
#89418 = CARTESIAN_POINT ( 'NONE',  ( -98.62536759172499501, -24.51419770103156992, 9.386484678747175181 ) ) ;
#89419 = DIRECTION ( 'NONE',  ( 0.000000000000000000, 0.000000000000000000, -1.000000000000000000 ) ) ;
#89420 = CARTESIAN_POINT ( 'NONE',  ( -85.50202734187257647, -24.63355581998384736, 0.9682620441943965428 ) ) ;
#89421 = DIRECTION ( 'NONE',  ( 0.000000000000000000, 0.000000000000000000, 1.000000000000000000 ) ) ;
#89422 = VECTOR ( 'NONE', #22239, 1000.000000000000000 ) ;
#89424 = CARTESIAN_POINT ( 'NONE',  ( -44.62287095715005592, -24.50321055353805733, 9.387540953477532923 ) ) ;
#89423 = B_SPLINE_CURVE_WITH_KNOTS ( 'NONE', 3,
 ( #50156, #26313, #88220, #80094, #81094, #10578 ),
 .UNSPECIFIED., .F., .F.,
 ( 4, 2, 4 ),
 ( 1.570755371634415583E-05, 0.001396183895866092740, 0.002776660238015841217 ),
 .UNSPECIFIED. ) ;
#89425 = EDGE_LOOP ( 'NONE', ( #4692, #69603, #73673, #31462 ) ) ;
#89426 = CARTESIAN_POINT ( 'NONE',  ( -18.73025074496528219, 5.678645368852136777, 11.49999999999999645 ) ) ;
#89427 = CARTESIAN_POINT ( 'NONE',  ( -99.21417444527331497, -25.30351579687176411, 4.454760979438658453 ) ) ;
#89428 = CARTESIAN_POINT ( 'NONE',  ( -29.68470166834870838, -25.15597160735836368, 6.410310830211703781 ) ) ;
#89429 = ADVANCED_FACE ( 'NONE', ( #50978 ), #53430, .T. ) ;
#89430 = ORIENTED_EDGE ( 'NONE', *, *, #10652, .F. ) ;
#89431 = CARTESIAN_POINT ( 'NONE',  ( 4.115044103975469270, -5.876774720514426953, 21.79213183355573946 ) ) ;
#89432 = CARTESIAN_POINT ( 'NONE',  ( -40.52287095715006870, -23.47596703998600631, 11.44779298504229281 ) ) ;
#89433 = PLANE ( 'NONE',  #32569 ) ;
#89434 = CARTESIAN_POINT ( 'NONE',  ( -62.58953762381672448, -23.48783264082478794, -1.443836473390068820 ) ) ;
#89436 = EDGE_CURVE ( 'NONE', #40482, #16731, #56779, .T. ) ;
#89435 = CARTESIAN_POINT ( 'NONE',  ( 19.16472379399037251, -4.548241762842377689, 11.49999999999998934 ) ) ;
#89437 = ORIENTED_EDGE ( 'NONE', *, *, #68747, .T. ) ;
#89438 = VECTOR ( 'NONE', #50396, 1000.000000000000114 ) ;
#89439 = CARTESIAN_POINT ( 'NONE',  ( -103.5228709571500758, -29.50247984919015209, -1.443849546365050029 ) ) ;
#89440 = DIRECTION ( 'NONE',  ( 1.000000000000000000, -0.000000000000000000, 0.000000000000000000 ) ) ;
#89441 = EDGE_CURVE ( 'NONE', #38032, #59306, #80916, .T. ) ;
#89442 = PERSON_AND_ORGANIZATION ( #70597, #27821 ) ;
#89443 = ORIENTED_EDGE ( 'NONE', *, *, #6468, .F. ) ;
#89444 = CARTESIAN_POINT ( 'NONE',  ( -74.52287095715007581, -23.48783264082476308, -1.443836473390090802 ) ) ;
#89445 = CARTESIAN_POINT ( 'NONE',  ( -59.62287095715007723, -23.47596703998600276, 11.44779298504227683 ) ) ;
#89446 = CARTESIAN_POINT ( 'NONE',  ( -47.62369814497165521, -24.65952944569304606, 1.056160979905696129 ) ) ;
#89447 = CARTESIAN_POINT ( 'NONE',  ( -118.5174284418064872, -24.51314013834317151, 0.6176544820404247238 ) ) ;
#89448 = CARTESIAN_POINT ( 'NONE',  ( -7.064692883725313344, -6.376774720514411854, 19.55266968305501862 ) ) ;
#89449 = CARTESIAN_POINT ( 'NONE',  ( -75.92287095715006728, -23.47596703998600631, 11.44779298504227860 ) ) ;
#89450 = DIRECTION ( 'NONE',  ( -3.773278334444167608E-23, 1.000000000000000000, 0.000000000000000000 ) ) ;
#89451 = CARTESIAN_POINT ( 'NONE',  ( 16.68016870136555596, 10.92824754362290385, -1.500000000000002220 ) ) ;
#89452 = CARTESIAN_POINT ( 'NONE',  ( -0.08873648434230119175, -21.90123647746391455, 10.22788351244709482 ) ) ;
#89453 = CARTESIAN_POINT ( 'NONE',  ( 19.12242951303546334, 5.485007674754557527, -1.500000000000002220 ) ) ;
#89454 = VERTEX_POINT ( 'NONE', #97139 ) ;
#89455 = PLANE ( 'NONE',  #84810 ) ;
#89456 = CARTESIAN_POINT ( 'NONE',  ( 4.329581153495547063, -5.876774720514421624, 21.24220543808225869 ) ) ;
#89457 = EDGE_CURVE ( 'NONE', #50718, #29681, #27136, .T. ) ;
#89458 = TOROIDAL_SURFACE ( 'NONE', #32744, 132.8284398600581540, 3.060000000000000053 ) ;
#89459 = B_SPLINE_CURVE_WITH_KNOTS ( 'NONE', 3,
 ( #84823, #68118, #38651, #100028 ),
 .UNSPECIFIED., .F., .F.,
 ( 4, 4 ),
 ( 0.000000000000000000, 1.000000000000000000 ),
 .UNSPECIFIED. ) ;
#89461 =( NAMED_UNIT ( * ) SI_UNIT ( $, .STERADIAN. ) SOLID_ANGLE_UNIT ( ) );
#89460 = LOCAL_TIME ( 0, 54, 15.00000000000000000, #30147 ) ;
#89462 = CARTESIAN_POINT ( 'NONE',  ( 10.16119454606143435, -6.376774720514430506, -28.04611093484508899 ) ) ;
#89463 = CARTESIAN_POINT ( 'NONE',  ( -49.62287095715005592, -23.48786465467241058, 11.44779295918254824 ) ) ;
#89464 = CARTESIAN_POINT ( 'NONE',  ( -7.024122139145243082, -5.876774720514408301, 19.17707164986947532 ) ) ;
#89465 = EDGE_CURVE ( 'NONE', #87638, #98717, #84602, .T. ) ;
#89466 = DIRECTION ( 'NONE',  ( 1.000000000000000000, 8.673617379884028076E-17, 6.938893903907222461E-16 ) ) ;
#89467 = ORIENTED_EDGE ( 'NONE', *, *, #95946, .F. ) ;
#89468 = CARTESIAN_POINT ( 'NONE',  ( 33.13288845015618023, 5.965225279485572685, -0.1650522222209214185 ) ) ;
#89469 = DIRECTION ( 'NONE',  ( 1.226388327005079762E-16, 0.000000000000000000, -1.000000000000000000 ) ) ;
#89470 = VERTEX_POINT ( 'NONE', #42870 ) ;
#89471 = CARTESIAN_POINT ( 'NONE',  ( 20.02926185082240451, -2.967945350358753398, 11.49999999999998934 ) ) ;
#89472 = CARTESIAN_POINT ( 'NONE',  ( -43.62287095715004881, -23.48783264082477729, -1.443836473390071928 ) ) ;
#89473 = DIRECTION ( 'NONE',  ( 0.000000000000000000, -2.173523156925980399E-06, 0.9999999999976378895 ) ) ;
#89474 = DIRECTION ( 'NONE',  ( 0.000000000000000000, -2.173523156925980399E-06, 0.9999999999976378895 ) ) ;
#89475 = ORIENTED_EDGE ( 'NONE', *, *, #2595, .T. ) ;
#89476 = CARTESIAN_POINT ( 'NONE',  ( -79.39668153920749205, -25.31497848055487765, 4.862330694693304700 ) ) ;
#89477 = CARTESIAN_POINT ( 'NONE',  ( -1.653359744423585465, -6.376774720514413630, 19.34586827028017098 ) ) ;
#89478 = CARTESIAN_POINT ( 'NONE',  ( -5.826506878040391690, 19.21762618028343184, -1.500000000000002220 ) ) ;
#89479 = CARTESIAN_POINT ( 'NONE',  ( 20.41947327098772647, -5.118016103960565388, 11.49999999999999645 ) ) ;
#89480 = CARTESIAN_POINT ( 'NONE',  ( -109.5228709571500616, -29.50250786944525672, 11.44777988621622988 ) ) ;
#89481 = LINE ( 'NONE', #19958, #82224 ) ;
#89482 = CARTESIAN_POINT ( 'NONE',  ( 5.627179592841175193, 21.36305014179116668, 11.49999999999998934 ) ) ;
#89483 = CARTESIAN_POINT ( 'NONE',  ( -39.46140038746126777, -25.31589174274902376, 4.366343845060879580 ) ) ;
#89484 = CARTESIAN_POINT ( 'NONE',  ( -47.62287095715004881, -23.47593901973091235, -1.443836447539009749 ) ) ;
#89485 = DIRECTION ( 'NONE',  ( 0.000000000000000000, -2.173523156925979552E-06, 0.9999999999976378895 ) ) ;
#89486 = VERTEX_POINT ( 'NONE', #91017 ) ;
#89487 = CARTESIAN_POINT ( 'NONE',  ( -72.54967600462832422, -24.15543982623907127, -0.2315651400026662310 ) ) ;
#89488 = CARTESIAN_POINT ( 'NONE',  ( -31.55269859854478653, -23.96119346886880663, -0.6495511937832003646 ) ) ;
#89489 = ORIENTED_EDGE ( 'NONE', *, *, #12893, .F. ) ;
#89490 = EDGE_LOOP ( 'NONE', ( #83727, #24347, #90510, #30783 ) ) ;
#89491 = CARTESIAN_POINT ( 'NONE',  ( -41.58953762381673158, -23.48786465467240703, 11.44779295918255180 ) ) ;
#89492 = CARTESIAN_POINT ( 'NONE',  ( -89.52287095715006160, -23.48786465467241769, 11.44779295918254292 ) ) ;
#89493 = DIRECTION ( 'NONE',  ( 0.000000000000000000, 0.000000000000000000, 1.000000000000000000 ) ) ;
#89494 = CARTESIAN_POINT ( 'NONE',  ( -17.31529204923715071, 11.11782870402162260, -1.500000000000002220 ) ) ;
#89495 = CARTESIAN_POINT ( 'NONE',  ( -16.67190562677319932, -13.68652177170558204, 11.49999999999999645 ) ) ;
#89496 = VERTEX_POINT ( 'NONE', #75782 ) ;
#89497 = LINE ( 'NONE', #80390, #75292 ) ;
#89498 = B_SPLINE_CURVE_WITH_KNOTS ( 'NONE', 3,
 ( #65044, #49808, #78707, #64044 ),
 .UNSPECIFIED., .F., .F.,
 ( 4, 4 ),
 ( 1.387778780781445521E-17, 0.0001000000000000028779 ),
 .UNSPECIFIED. ) ;
#89499 = CARTESIAN_POINT ( 'NONE',  ( 8.376690734369038438, 12.50000000000004974, 2.100000000000000089 ) ) ;
#89500 = CARTESIAN_POINT ( 'NONE',  ( -35.62287095715004881, -23.48783264082477729, -1.443836473390072372 ) ) ;
#89501 = CARTESIAN_POINT ( 'NONE',  ( 16.41691039316204481, 15.16158741987741365, 11.49999999999998934 ) ) ;
#89502 = CARTESIAN_POINT ( 'NONE',  ( 9.278253834636469577, -5.876774720514426953, 21.48128695274316158 ) ) ;
#89503 = CARTESIAN_POINT ( 'NONE',  ( -32.68833172073793492, -25.12026506542017046, 2.831122744435439209 ) ) ;
#89504 = VERTEX_POINT ( 'NONE', #67706 ) ;
#89505 = CARTESIAN_POINT ( 'NONE',  ( 11.62916340711181284, 5.965225279485572685, 28.75961759920349792 ) ) ;
#89506 = CARTESIAN_POINT ( 'NONE',  ( 31.42094490286590514, 4.276934461241891583, -0.4045216949806126339 ) ) ;
#89507 = CARTESIAN_POINT ( 'NONE',  ( 3.889286922045745776, 20.52237432693057073, -1.500000000000002220 ) ) ;
#89508 = AXIS2_PLACEMENT_3D ( 'NONE', #6340, #59649, #37301 ) ;
#89509 = VERTEX_POINT ( 'NONE', #12886 ) ;
#89511 = ORIENTED_EDGE ( 'NONE', *, *, #79437, .F. ) ;
#89510 = FACE_OUTER_BOUND ( 'NONE', #66206, .T. ) ;
#89512 = EDGE_LOOP ( 'NONE', ( #29842, #22490, #20142, #26838 ) ) ;
#89513 = CARTESIAN_POINT ( 'NONE',  ( -51.25961469856053299, -25.27945219851612535, 4.204089154875919832 ) ) ;
#89514 = CARTESIAN_POINT ( 'NONE',  ( 10.44912437418449969, 18.32051524777507723, -1.500000000000002220 ) ) ;
#89515 = VERTEX_POINT ( 'NONE', #36738 ) ;
#89516 = CARTESIAN_POINT ( 'NONE',  ( -28.52287095715006870, -24.17669640916165363, 0.1849426640301049252 ) ) ;
#89518 = EDGE_CURVE ( 'NONE', #67226, #47093, #74303, .T. ) ;
#89517 = CARTESIAN_POINT ( 'NONE',  ( -6.741682653110981249, 5.965225279485572685, 30.62569541381301619 ) ) ;
#89519 = CARTESIAN_POINT ( 'NONE',  ( -120.5208167607407574, -23.85049219812686871, 10.88485053497526778 ) ) ;
#89520 = ADVANCED_FACE ( 'NONE', ( #67207 ), #98623, .T. ) ;
#89521 = DIRECTION ( 'NONE',  ( 1.000000000000000000, 0.000000000000000000, 0.000000000000000000 ) ) ;
#89522 = CARTESIAN_POINT ( 'NONE',  ( -49.10800655684114702, -25.25745592776986825, 3.918720070390376176 ) ) ;
#89523 = CARTESIAN_POINT ( 'NONE',  ( -19.66401359581072583, -9.230316601043258018, -1.500000000000002220 ) ) ;
#89524 = DIRECTION ( 'NONE',  ( -0.000000000000000000, 1.000000000000000000, -0.000000000000000000 ) ) ;
#89526 = ORIENTED_EDGE ( 'NONE', *, *, #18721, .T. ) ;
#89525 = CARTESIAN_POINT ( 'NONE',  ( -21.62769966018443313, 5.350386031573528989, 11.49999999999999645 ) ) ;
#89527 = CARTESIAN_POINT ( 'NONE',  ( -50.37830952628071657, -25.31441722265898875, 5.197788989113472979 ) ) ;
#89528 = CYLINDRICAL_SURFACE ( 'NONE', #44307, 1.000000000000000000 ) ;
#89529 = LINE ( 'NONE', #59094, #31025 ) ;
#89530 = ORIENTED_EDGE ( 'NONE', *, *, #58949, .F. ) ;
#89531 = EDGE_CURVE ( 'NONE', #2820, #78888, #74787, .T. ) ;
#89532 = EDGE_CURVE ( 'NONE', #64113, #84269, #99609, .T. ) ;
#89534 = ORIENTED_EDGE ( 'NONE', *, *, #13901, .F. ) ;
#89533 = CARTESIAN_POINT ( 'NONE',  ( -36.22287095715006444, -23.47596703998600276, 11.44779298504227683 ) ) ;
#89535 = VECTOR ( 'NONE', #8189, 1000.000000000000000 ) ;
#89536 = ORIENTED_EDGE ( 'NONE', *, *, #51188, .T. ) ;
#89537 = LOCAL_TIME ( 0, 54, 15.00000000000000000, #30284 ) ;
#89538 = CARTESIAN_POINT ( 'NONE',  ( -75.52287095715007581, -24.52232992886362695, 0.6492154411906060352 ) ) ;
#89539 = FACE_OUTER_BOUND ( 'NONE', #9649, .T. ) ;
#89540 = CARTESIAN_POINT ( 'NONE',  ( -103.5228709571500758, -24.65952944569304606, 1.056160979905702346 ) ) ;
#89541 = FACE_OUTER_BOUND ( 'NONE', #43324, .T. ) ;
#89542 = EDGE_CURVE ( 'NONE', #477, #2525, #21490, .T. ) ;
#89543 = CARTESIAN_POINT ( 'NONE',  ( -66.52287095715004739, -23.95044443724993144, 10.65354141964649237 ) ) ;
#89544 = ORIENTED_EDGE ( 'NONE', *, *, #35220, .F. ) ;
#89545 = CARTESIAN_POINT ( 'NONE',  ( 12.26431755764203047, -15.03328313062362298, 11.49999999999999645 ) ) ;
#89546 = DIRECTION ( 'NONE',  ( -0.000000000000000000, 2.173523156925979552E-06, -0.9999999999976378895 ) ) ;
#89547 = CARTESIAN_POINT ( 'NONE',  ( -1.649324495273077451, -22.40575143947253167, -1.500000000000002220 ) ) ;
#89548 = AXIS2_PLACEMENT_3D ( 'NONE', #35614, #3176, #11759 ) ;
#89549 = EDGE_LOOP ( 'NONE', ( #50158, #72068, #54838, #67521 ) ) ;
#89550 = FACE_OUTER_BOUND ( 'NONE', #63726, .T. ) ;
#89551 = CARTESIAN_POINT ( 'NONE',  ( 2.610950917001260141, -5.876774720514412742, 19.54489930512155027 ) ) ;
#89552 = FACE_OUTER_BOUND ( 'NONE', #62212, .T. ) ;
#89553 = CARTESIAN_POINT ( 'NONE',  ( -63.92535995814584027, -24.57215472537218304, 9.174899246800711339 ) ) ;
#89554 = CARTESIAN_POINT ( 'NONE',  ( 0.9049686737998731134, -19.58615294826029540, -1.500000000000002220 ) ) ;
#89555 = B_SPLINE_SURFACE_WITH_KNOTS ( 'NONE', 3, 3, ( 
 ( #98078, #28094, #28584, #4261 ),
 ( #20461, #35210, #51433, #82369 ),
 ( #73274, #66683, #89488, #42340 ),
 ( #12353, #74263, #20961, #57560 ),
 ( #51932, #5247, #43326, #97594 ),
 ( #43816, #74751, #36205, #13347 ),
 ( #72779, #88496, #80881, #3768 ) ),
 .UNSPECIFIED., .F., .F., .F.,
 ( 4, 3, 4 ),
 ( 4, 4 ),
 ( 0.0004766839783831800718, 0.1029713700210899974, 0.2054660560637968092 ),
 ( 0.9897457716632639402, 0.9912151630997512175 ),
 .UNSPECIFIED. ) ;
#89556 = CARTESIAN_POINT ( 'NONE',  ( -120.5228709571500616, -23.47596703998600631, 11.44779298504227860 ) ) ;
#89557 = VERTEX_POINT ( 'NONE', #4795 ) ;
#89558 = CARTESIAN_POINT ( 'NONE',  ( -11.74548148041400708, 18.04809798412036059, 11.49999999999998934 ) ) ;
#89559 = CARTESIAN_POINT ( 'NONE',  ( 5.109298100548420152, -3.316774720514426456, -27.55941679637948383 ) ) ;
#89560 = CARTESIAN_POINT ( 'NONE',  ( -71.30376622360817862, -25.12218957384495965, 6.239614793150383143 ) ) ;
#89562 = B_SPLINE_CURVE_WITH_KNOTS ( 'NONE', 3,
 ( #99661, #21548, #75840, #30167 ),
 .UNSPECIFIED., .F., .F.,
 ( 4, 4 ),
 ( 0.000000000000000000, 9.999999999998898659E-05 ),
 .UNSPECIFIED. ) ;
#89561 = CARTESIAN_POINT ( 'NONE',  ( -75.52287095715007581, -23.48786465467241769, 11.44779295918254469 ) ) ;
#89563 = LINE ( 'NONE', #2338, #79603 ) ;
#89564 = CARTESIAN_POINT ( 'NONE',  ( 16.23347398924790497, -16.23827457187686463, -1.500000000000002220 ) ) ;
#89565 = AXIS2_PLACEMENT_3D ( 'NONE', #57994, #50372, #28025 ) ;
#89566 = APPROVAL_ROLE ( '' ) ;
#89567 = LINE ( 'NONE', #90064, #6160 ) ;
#89568 = CARTESIAN_POINT ( 'NONE',  ( -49.58209155508411925, -24.51314013834316086, 0.6176544820404115121 ) ) ;
#89569 = CARTESIAN_POINT ( 'NONE',  ( -1.972954090310384379, -20.06304030521763337, 11.49999999999999645 ) ) ;
#89570 = CARTESIAN_POINT ( 'NONE',  ( -109.4252266130965552, -25.10927462135256150, 3.135431895769846822 ) ) ;
#89571 = LINE ( 'NONE', #72356, #98683 ) ;
#89572 = PRODUCT_DEFINITION_SHAPE ( 'NONE', 'NONE',  #29568 ) ;
#89573 = CARTESIAN_POINT ( 'NONE',  ( -4.533825836049095059, -5.876774720514412742, 19.59623724171353132 ) ) ;
#89574 = DIRECTION ( 'NONE',  ( -0.000000000000000000, -1.000000000000000000, 0.000000000000000000 ) ) ;
#89575 = CARTESIAN_POINT ( 'NONE',  ( -46.62287095715004881, -29.50247984919015209, -1.443849546365058689 ) ) ;
#89576 = CARTESIAN_POINT ( 'NONE',  ( -19.70454523906213495, -2.556213046838741842, 11.49999999999998934 ) ) ;
#89577 = AXIS2_PLACEMENT_3D ( 'NONE', #96475, #3642, #26477 ) ;
#89578 = CARTESIAN_POINT ( 'NONE',  ( -109.6228709571500559, -24.64898659630368627, 1.056161002820831474 ) ) ;
#89579 = CARTESIAN_POINT ( 'NONE',  ( 2.169241753049089727, -19.58708112974024829, -1.500000000000002220 ) ) ;
#89580 = EDGE_CURVE ( 'NONE', #46174, #81901, #47055, .T. ) ;
#89581 = CARTESIAN_POINT ( 'NONE',  ( -126.5899057953276667, -24.15620529776629510, 10.23563542870658871 ) ) ;
#89582 = AXIS2_PLACEMENT_3D ( 'NONE', #86442, #38759, #48388 ) ;
#89583 = CARTESIAN_POINT ( 'NONE',  ( -110.5228709571500190, -24.14406661686757971, 10.28769366194080526 ) ) ;
#89584 = CARTESIAN_POINT ( 'NONE',  ( -79.52287095715006160, -24.50321055353805377, 9.387540953477524042 ) ) ;
#89585 = CARTESIAN_POINT ( 'NONE',  ( 20.28538307770854487, 3.844468116359331944, 11.49999999999999645 ) ) ;
#89586 = EDGE_CURVE ( 'NONE', #53085, #1756, #35749, .T. ) ;
#89587 = PLANE ( 'NONE',  #36679 ) ;
#89588 = CARTESIAN_POINT ( 'NONE',  ( -22.35490716430079061, -3.811827842488555440, 11.49999999999999645 ) ) ;
#89589 = ORIENTED_EDGE ( 'NONE', *, *, #23311, .F. ) ;
#89590 = CARTESIAN_POINT ( 'NONE',  ( -8.160000000000000142, -10.65233964170348635, -1.621096496867198589 ) ) ;
#89591 = CARTESIAN_POINT ( 'NONE',  ( 30.61643171255909479, 3.477635932356431869, 27.37433006808820579 ) ) ;
#89592 = CARTESIAN_POINT ( 'NONE',  ( -63.59273280689718888, -24.15543982623906771, -0.2315651400026651485 ) ) ;
#89593 = PLANE ( 'NONE',  #22040 ) ;
#89594 = ORIENTED_EDGE ( 'NONE', *, *, #6477, .T. ) ;
#89595 = B_SPLINE_CURVE_WITH_KNOTS ( 'NONE', 3,
 ( #51500, #14412, #74330, #76304 ),
 .UNSPECIFIED., .F., .F.,
 ( 4, 4 ),
 ( 0.000000000000000000, 9.999999999998897304E-05 ),
 .UNSPECIFIED. ) ;
#89596 = ORIENTED_EDGE ( 'NONE', *, *, #12767, .F. ) ;
#89597 = AXIS2_PLACEMENT_3D ( 'NONE', #9705, #71111, #24422 ) ;
#89598 = CARTESIAN_POINT ( 'NONE',  ( -30.51968327036646400, -23.47799326397811726, -1.443836481326576271 ) ) ;
#89599 = CARTESIAN_POINT ( 'NONE',  ( 18.61037501828884189, -13.27421459584354579, -1.500000000000002220 ) ) ;
#89600 = CARTESIAN_POINT ( 'NONE',  ( -130.5728709571500588, -23.56000036390796737, 11.50200000000000244 ) ) ;
#89601 = CARTESIAN_POINT ( 'NONE',  ( 17.58597629297885589, -12.55149374826878272, -1.500000000000002220 ) ) ;
#89602 = CARTESIAN_POINT ( 'NONE',  ( -113.5949056871682359, -23.48786465467241413, 11.44779295918254292 ) ) ;
#89603 = LINE ( 'NONE', #82972, #77625 ) ;
#89604 = CC_DESIGN_SECURITY_CLASSIFICATION ( #2120, ( #100426 ) ) ;
#89605 = CARTESIAN_POINT ( 'NONE',  ( -15.68175098440391402, -16.16561365185589594, 11.49999999999999645 ) ) ;
#89606 = ORIENTED_EDGE ( 'NONE', *, *, #46743, .T. ) ;
#89607 = CARTESIAN_POINT ( 'NONE',  ( -43.52287095715006160, -24.65952944569304606, 1.056160979905691910 ) ) ;
#89608 = CARTESIAN_POINT ( 'NONE',  ( 21.96865551644221881, -1.217672407684077918, -1.500000000000002220 ) ) ;
#89609 = DIRECTION ( 'NONE',  ( 1.000000000000000000, 0.000000000000000000, 0.000000000000000000 ) ) ;
#89610 = CARTESIAN_POINT ( 'NONE',  ( -29.23483314410334444, -25.21724520516633561, 5.425066621826060143 ) ) ;
#89611 = VECTOR ( 'NONE', #21170, 1000.000000000000000 ) ;
#89612 = ORIENTED_EDGE ( 'NONE', *, *, #81422, .F. ) ;
#89613 = FACE_OUTER_BOUND ( 'NONE', #56896, .T. ) ;
#89614 = CARTESIAN_POINT ( 'NONE',  ( -47.62287095715006302, -23.47596703998600276, 11.44779298504227505 ) ) ;
#89615 = ORIENTED_EDGE ( 'NONE', *, *, #99037, .F. ) ;
#89616 = CARTESIAN_POINT ( 'NONE',  ( -6.741682653110981249, 0.3587747205144265483, 30.62569541381301619 ) ) ;
#89617 = VERTEX_POINT ( 'NONE', #20500 ) ;
#89618 = ORIENTED_EDGE ( 'NONE', *, *, #65848, .F. ) ;
#89619 = AXIS2_PLACEMENT_3D ( 'NONE', #1805, #64223, #95149 ) ;
#89620 = ORIENTED_EDGE ( 'NONE', *, *, #57526, .F. ) ;
#89621 = DIRECTION ( 'NONE',  ( -3.773278334453079618E-23, 0.9999999999976377785, 2.173523156925979975E-06 ) ) ;
#89622 = LINE ( 'NONE', #52558, #71344 ) ;
#89623 = CARTESIAN_POINT ( 'NONE',  ( -50.52287095715006160, -24.99132157543166599, 2.256160258750667502 ) ) ;
#89624 = CARTESIAN_POINT ( 'NONE',  ( -4.163110563111144913, -19.98234244090558320, -1.500000000000002220 ) ) ;
#89625 = ORIENTED_EDGE ( 'NONE', *, *, #47826, .T. ) ;
#89626 = CARTESIAN_POINT ( 'NONE',  ( -1.022535880784302353, -5.876774720514415407, 19.99258394656883908 ) ) ;
#89627 = LINE ( 'NONE', #50566, #69262 ) ;
#89628 = EDGE_CURVE ( 'NONE', #30676, #78152, #79742, .T. ) ;
#89629 = CARTESIAN_POINT ( 'NONE',  ( -97.52287095715006160, -23.94994826722564341, -0.6494450866342716955 ) ) ;
#89630 = CARTESIAN_POINT ( 'NONE',  ( -56.62287095715005592, -29.50250243563736774, 8.947779886222145151 ) ) ;
#89631 = ORIENTED_EDGE ( 'NONE', *, *, #64587, .F. ) ;
#89632 = CARTESIAN_POINT ( 'NONE',  ( -83.62287095715007013, -23.47596703998600631, 11.44779298504227860 ) ) ;
#89633 = FACE_OUTER_BOUND ( 'NONE', #48761, .T. ) ;
#89634 = ORIENTED_EDGE ( 'NONE', *, *, #49906, .F. ) ;
#89635 = CARTESIAN_POINT ( 'NONE',  ( -19.11632921840048738, -8.121837694355717119, -1.500000000000002220 ) ) ;
#89636 = ORIENTED_EDGE ( 'NONE', *, *, #38154, .T. ) ;
#89638 = ORIENTED_EDGE ( 'NONE', *, *, #78741, .T. ) ;
#89637 = CARTESIAN_POINT ( 'NONE',  ( -53.52287095715006870, -29.50250243563736774, 8.947779886222146928 ) ) ;
#89639 = B_SPLINE_SURFACE_WITH_KNOTS ( 'NONE', 3, 1, ( 
 ( #23296, #16695 ),
 ( #78580, #55281 ),
 ( #84705, #15196 ),
 ( #54282, #39037 ),
 ( #46159, #22293 ),
 ( #45658, #77087 ),
 ( #93315, #7587 ),
 ( #85716, #69495 ),
 ( #47162, #15698 ),
 ( #62385, #40041 ),
 ( #100411, #29924 ),
 ( #8593, #70495 ),
 ( #980, #31932 ),
 ( #62901, #60891 ),
 ( #87211, #4365 ),
 ( #17704, #72005 ),
 ( #59148, #64410 ),
 ( #10090, #20564 ),
 ( #51534, #32429 ) ),
 .UNSPECIFIED., .F., .F., .F.,
 ( 4, 1, 1, 1, 1, 1, 1, 1, 1, 1, 1, 1, 1, 1, 1, 1, 4 ),
 ( 2, 2 ),
 ( 0.000000000000000000, 0.07269466619231579330, 0.1413526962021420808, 0.2082288969497901876, 0.2736894576468447138, 0.3380517659755425397, 0.4009220982745032025, 0.4636163844951721735, 0.5278777255384771161, 0.5636262148099120406, 0.6061036626598774735, 0.6545011613018643093, 0.7100543472033249426, 0.7722619378848212257, 0.8412211450824306214, 0.9174702961779349630, 1.000000000000000000 ),
 ( 0.000000000000000000, 1.000000000000000000 ),
 .UNSPECIFIED. ) ;
#89640 = CARTESIAN_POINT ( 'NONE',  ( -44.55620429048338593, -23.47596703998600276, 11.44779298504227505 ) ) ;
#89641 = CARTESIAN_POINT ( 'NONE',  ( -67.62287095715005592, -29.50248528299804818, 1.056150453629036701 ) ) ;
#89642 = ORIENTED_EDGE ( 'NONE', *, *, #93018, .F. ) ;
#89643 = EDGE_LOOP ( 'NONE', ( #81983, #46679, #53042, #50578 ) ) ;
#89644 = CARTESIAN_POINT ( 'NONE',  ( -79.62287095715004170, -24.65952944569304606, 1.056160979905697461 ) ) ;
#89645 = EDGE_CURVE ( 'NONE', #38032, #37450, #65236, .T. ) ;
#89646 = CARTESIAN_POINT ( 'NONE',  ( -123.5895376238167245, -24.64965694238408034, 8.947790433994649462 ) ) ;
#89647 = CARTESIAN_POINT ( 'NONE',  ( -55.55620429048340014, -23.48783264082478439, -1.443836473390068820 ) ) ;
#89648 = CARTESIAN_POINT ( 'NONE',  ( -71.30164606794451743, -25.24515217160483971, 6.118441223290502329 ) ) ;
#89650 = ORIENTED_EDGE ( 'NONE', *, *, #80746, .F. ) ;
#89649 = CARTESIAN_POINT ( 'NONE',  ( 7.254013858510784729, 20.86747967231135803, 11.49999999999999645 ) ) ;
#89651 = CARTESIAN_POINT ( 'NONE',  ( 9.299999999999993605, 12.00000000000002309, 0.000000000000000000 ) ) ;
#89652 = CIRCLE ( 'NONE', #18307, 2.500000000000000444 ) ;
#89653 = EDGE_CURVE ( 'NONE', #22449, #73934, #80984, .T. ) ;
#89654 = CARTESIAN_POINT ( 'NONE',  ( 12.73759380600583846, -18.68238426224762350, 11.49999999999998934 ) ) ;
#89655 = EDGE_CURVE ( 'NONE', #99448, #99058, #17830, .T. ) ;
#89657 = ORIENTED_EDGE ( 'NONE', *, *, #98921, .F. ) ;
#89656 = DIRECTION ( 'NONE',  ( 0.000000000000000000, -2.173523156925979552E-06, 0.9999999999976378895 ) ) ;
#89658 = AXIS2_PLACEMENT_3D ( 'NONE', #7828, #56025, #63137 ) ;
#89659 = EDGE_CURVE ( 'NONE', #71190, #42155, #43859, .T. ) ;
#89660 = ORIENTED_EDGE ( 'NONE', *, *, #16939, .T. ) ;
#89661 = EDGE_CURVE ( 'NONE', #43450, #33967, #83335, .T. ) ;
#89662 = CARTESIAN_POINT ( 'NONE',  ( -80.43221577628075636, -25.31553502933635968, 4.967019755914117596 ) ) ;
#89663 = DIRECTION ( 'NONE',  ( 0.000000000000000000, 0.000000000000000000, -1.000000000000000000 ) ) ;
#89664 = ORIENTED_EDGE ( 'NONE', *, *, #20223, .F. ) ;
#89665 = CARTESIAN_POINT ( 'NONE',  ( -17.67215177357914513, -11.65580189297658897, 11.49999999999998934 ) ) ;
#89666 = CARTESIAN_POINT ( 'NONE',  ( 32.96821357219067750, 5.071478440980570213, -13.00504694253962867 ) ) ;
#89667 = CYLINDRICAL_SURFACE ( 'NONE', #45435, 4.080000000000000071 ) ;
#89668 = CARTESIAN_POINT ( 'NONE',  ( 11.81759748825469281, -18.92407201980706333, -1.500000000000002220 ) ) ;
#89669 = DIRECTION ( 'NONE',  ( 0.000000000000000000, 0.000000000000000000, 1.000000000000000000 ) ) ;
#89670 = ADVANCED_FACE ( 'NONE', ( #51971 ), #76280, .F. ) ;
#89671 = VERTEX_POINT ( 'NONE', #15379 ) ;
#89672 = DIRECTION ( 'NONE',  ( 0.9975640502598243087, -0.06975647374412546897, -0.000000000000000000 ) ) ;
#89673 = CARTESIAN_POINT ( 'NONE',  ( -50.62287095715005592, -23.47596703998600631, 11.44779298504227505 ) ) ;
#89674 = DIRECTION ( 'NONE',  ( -1.000000000000000000, 0.000000000000000000, 0.000000000000000000 ) ) ;
#89675 = CARTESIAN_POINT ( 'NONE',  ( 20.07151214508649772, 3.809612236891415094E-15, 0.000000000000000000 ) ) ;
#89676 = AXIS2_PLACEMENT_3D ( 'NONE', #92315, #60398, #45654 ) ;
#89677 = CARTESIAN_POINT ( 'NONE',  ( -13.79594968651775666, -13.80015156857029268, 11.49999999999998934 ) ) ;
#89678 = CARTESIAN_POINT ( 'NONE',  ( -18.57871158907727249, 10.67946855401146777, -1.500000000000002220 ) ) ;
#89679 = CARTESIAN_POINT ( 'NONE',  ( -27.65533724976895869, -24.92774666542950257, 1.629627248584496257 ) ) ;
#89680 = CARTESIAN_POINT ( 'NONE',  ( 6.817041430359983778, -0.6681657214399134848, 19.30000000000000071 ) ) ;
#89681 = CARTESIAN_POINT ( 'NONE',  ( 8.376690734369038438, 11.49999999999999645, 0.000000000000000000 ) ) ;
#89682 = CARTESIAN_POINT ( 'NONE',  ( -21.74551633039419585, 6.958787177381512201, -1.500000000000002220 ) ) ;
#89683 = AXIS2_PLACEMENT_3D ( 'NONE', #45503, #14023, #60234 ) ;
#89684 =( NAMED_UNIT ( * ) PLANE_ANGLE_UNIT ( ) SI_UNIT ( $, .RADIAN. ) );
#89685 = DIRECTION ( 'NONE',  ( 0.000000000000000000, -0.9999999999976377785, -2.173523156925979975E-06 ) ) ;
#89686 = DIRECTION ( 'NONE',  ( -3.773278334453079618E-23, 0.9999999999976377785, 2.173523156925979975E-06 ) ) ;
#89687 = CARTESIAN_POINT ( 'NONE',  ( 19.23997954701083657, -5.074110557352235595, 11.49999999999999645 ) ) ;
#89688 = CARTESIAN_POINT ( 'NONE',  ( -104.5928578189489855, -23.96119346886880663, -0.6495511937832033622 ) ) ;
#89689 = CIRCLE ( 'NONE', #36238, 1.020000000000000018 ) ;
#89690 = CARTESIAN_POINT ( 'NONE',  ( -123.6228709571500559, -24.50216790748099527, 0.6166512839513689226 ) ) ;
#89691 = CARTESIAN_POINT ( 'NONE',  ( -56.62287095715008434, -23.47596703998600276, 11.44779298504227683 ) ) ;
#89692 = B_SPLINE_CURVE_WITH_KNOTS ( 'NONE', 3,
 ( #21143, #7797, #83038, #90172 ),
 .UNSPECIFIED., .F., .F.,
 ( 4, 4 ),
 ( 1.387778780781445521E-17, 9.999999999996123101E-05 ),
 .UNSPECIFIED. ) ;
#89693 = VERTEX_POINT ( 'NONE', #38723 ) ;
#89694 = LINE ( 'NONE', #81587, #49417 ) ;
#89695 = EDGE_CURVE ( 'NONE', #34128, #6026, #74536, .T. ) ;
#89696 = CARTESIAN_POINT ( 'NONE',  ( -62.62287095715004881, -24.64965695001468404, 8.947790433994185832 ) ) ;
#89697 = CARTESIAN_POINT ( 'NONE',  ( 13.45394552336293614, 17.01807010946250287, 11.49999999999998934 ) ) ;
#89698 = DIRECTION ( 'NONE',  ( 0.9762960071199348056, 0.2164396139380966033, 0.000000000000000000 ) ) ;
#89699 = B_SPLINE_CURVE_WITH_KNOTS ( 'NONE', 3,
 ( #47411, #78338, #84959, #77337, #38786, #228 ),
 .UNSPECIFIED., .F., .F.,
 ( 4, 2, 4 ),
 ( 0.000000000000000000, 0.001380764517854767134, 0.002761529035709534268 ),
 .UNSPECIFIED. ) ;
#89700 = CARTESIAN_POINT ( 'NONE',  ( -12.82114019720147802, -14.77593736753402709, -1.500000000000002220 ) ) ;
#89701 = B_SPLINE_CURVE_WITH_KNOTS ( 'NONE', 3,
 ( #94117, #63704, #64203, #86010, #79892, #70794 ),
 .UNSPECIFIED., .F., .F.,
 ( 4, 2, 4 ),
 ( 6.384118695823475424E-06, 0.001386860460836977695, 0.002767336802978131918 ),
 .UNSPECIFIED. ) ;
#89702 = PLANE ( 'NONE',  #11810 ) ;
#89703 = EDGE_CURVE ( 'NONE', #87231, #35025, #1040, .T. ) ;
#89704 = ORIENTED_EDGE ( 'NONE', *, *, #43077, .T. ) ;
#89705 = COORDINATED_UNIVERSAL_TIME_OFFSET ( 0, 0, .AHEAD. ) ;
#89706 = B_SPLINE_CURVE_WITH_KNOTS ( 'NONE', 3,
 ( #98914, #77069, #7575, #76076, #99898, #61876, #60387, #38523 ),
 .UNSPECIFIED., .F., .F.,
 ( 4, 2, 2, 4 ),
 ( 6.391158118966157767E-06, 0.002007136338672926151, 0.003007508928949903862, 0.004007881519226882440 ),
 .UNSPECIFIED. ) ;
#89707 = PLANE ( 'NONE',  #77496 ) ;
#89708 = CARTESIAN_POINT ( 'NONE',  ( -18.53176153473302179, -8.692061069824589481, 11.49999999999999645 ) ) ;
#89709 = CARTESIAN_POINT ( 'NONE',  ( -49.27764846858840997, -25.25176233969420636, 6.145204990682164414 ) ) ;
#89710 = DIRECTION ( 'NONE',  ( -0.9970298735180330718, -0.07701578612606008178, -9.020562075079398124E-17 ) ) ;
#89711 = VERTEX_POINT ( 'NONE', #8280 ) ;
#89712 = EDGE_CURVE ( 'NONE', #37238, #18378, #55497, .T. ) ;
#89713 = LINE ( 'NONE', #81600, #36218 ) ;
#89714 = PLANE ( 'NONE',  #29934 ) ;
#89715 = DIRECTION ( 'NONE',  ( -1.000000000000000000, -1.232047923278981953E-16, 0.000000000000000000 ) ) ;
#89716 = EDGE_CURVE ( 'NONE', #96004, #57696, #76145, .T. ) ;
#89717 = CARTESIAN_POINT ( 'NONE',  ( 1.949999999999999956, -0.1925000000000007261, 0.1924999999999992828 ) ) ;
#89718 = AXIS2_PLACEMENT_3D ( 'NONE', #88536, #31365, #80417 ) ;
#89719 = VERTEX_POINT ( 'NONE', #39221 ) ;
#89720 = PLANE ( 'NONE',  #73932 ) ;
#89721 = CARTESIAN_POINT ( 'NONE',  ( -20.90396053131702914, -9.656267258341529214, 11.49999999999999645 ) ) ;
#89722 = CARTESIAN_POINT ( 'NONE',  ( 4.306090731860143350, 22.38281141545218844, 11.49999999999998934 ) ) ;
#89723 = CARTESIAN_POINT ( 'NONE',  ( -70.66110687620329145, -25.30458803562652292, 4.882286574251741840 ) ) ;
#89724 = AXIS2_PLACEMENT_3D ( 'NONE', #81565, #73454, #34890 ) ;
#89725 = CARTESIAN_POINT ( 'NONE',  ( -40.52287095715010423, -24.14321612903120950, -0.2833117244520996780 ) ) ;
#89726 = CARTESIAN_POINT ( 'NONE',  ( -49.50841769935765768, -25.27292115247390569, 3.984447733149576898 ) ) ;
#89727 = LINE ( 'NONE', #58287, #43075 ) ;
#89728 = CARTESIAN_POINT ( 'NONE',  ( -69.47459837275444272, -25.20046511427854341, 6.675966739650351478 ) ) ;
#89729 = CARTESIAN_POINT ( 'NONE',  ( 18.42579859434530931, 11.83097890990371148, -1.500000000000002220 ) ) ;
#89730 = CC_DESIGN_PERSON_AND_ORGANIZATION_ASSIGNMENT ( #41271, #56510, ( #70488 ) ) ;
#89731 = CARTESIAN_POINT ( 'NONE',  ( -82.62287095715005592, -29.50250243563736774, 8.947779886222141599 ) ) ;
#89732 = PLANE ( 'NONE',  #47648 ) ;
#89733 = CARTESIAN_POINT ( 'NONE',  ( -120.6228709571500133, -24.14321612903117753, -0.2833117244520986233 ) ) ;
#89734 = LINE ( 'NONE', #13088, #76054 ) ;
#89735 = ORIENTED_EDGE ( 'NONE', *, *, #83269, .F. ) ;
#89736 = B_SPLINE_CURVE_WITH_KNOTS ( 'NONE', 3,
 ( #17947, #42592, #24458, #43579, #89752, #34468, #74518, #63044 ),
 .UNSPECIFIED., .F., .F.,
 ( 4, 2, 2, 4 ),
 ( -0.001240666984355843008, -0.0002401179793395007492, 0.0007604310256768415099, 0.002761529035709526028 ),
 .UNSPECIFIED. ) ;
#89737 = CARTESIAN_POINT ( 'NONE',  ( 3.609400094169940676, -20.08663944828865766, 11.49999999999998934 ) ) ;
#89738 = EDGE_LOOP ( 'NONE', ( #30866, #26890, #55993 ) ) ;
#89739 = VERTEX_POINT ( 'NONE', #62577 ) ;
#89740 = VERTEX_POINT ( 'NONE', #663 ) ;
#89741 = ORIENTED_EDGE ( 'NONE', *, *, #59997, .T. ) ;
#89742 = CARTESIAN_POINT ( 'NONE',  ( -21.75560140871883164, 7.562747417745157463, -1.500000000000002220 ) ) ;
#89743 = CARTESIAN_POINT ( 'NONE',  ( -34.62287095715005592, -29.50250786944525672, 11.44777988621624409 ) ) ;
#89744 = CARTESIAN_POINT ( 'NONE',  ( 20.17645099164838030, 1.678240329834772115, -1.500000000000002220 ) ) ;
#89745 = ORIENTED_EDGE ( 'NONE', *, *, #56660, .F. ) ;
#89746 = CARTESIAN_POINT ( 'NONE',  ( -5.837039262820512775, -6.376774720514413630, 19.76512419871795245 ) ) ;
#89747 = CARTESIAN_POINT ( 'NONE',  ( -78.22287095715006444, -23.47596703998600631, 11.44779298504227860 ) ) ;
#89748 = CARTESIAN_POINT ( 'NONE',  ( -51.62287095715005592, -23.47596703998600631, 11.44779298504227505 ) ) ;
#89749 = LINE ( 'NONE', #27350, #64231 ) ;
#89751 = ORIENTED_EDGE ( 'NONE', *, *, #74234, .T. ) ;
#89750 = CARTESIAN_POINT ( 'NONE',  ( -7.638042729800005759, 19.97414216180626667, 11.49999999999999645 ) ) ;
#89752 = CARTESIAN_POINT ( 'NONE',  ( -55.52287095715007581, -24.51163499207173402, 0.6490370598554341397 ) ) ;
#89753 = ORIENTED_EDGE ( 'NONE', *, *, #86690, .T. ) ;
#89754 = CARTESIAN_POINT ( 'NONE',  ( 14.93699691249320693, 16.48547057857716425, 11.49999999999998934 ) ) ;
#89755 = CARTESIAN_POINT ( 'NONE',  ( -6.067718162532647064, 19.77315050736717694, 11.49999999999998934 ) ) ;
#89757 = EDGE_LOOP ( 'NONE', ( #12295, #82862, #6125, #60678 ) ) ;
#89756 = VECTOR ( 'NONE', #80571, 1000.000000000000000 ) ;
#89758 = CARTESIAN_POINT ( 'NONE',  ( 2.904396343079095111, -5.876774720514415407, 19.95793242748194984 ) ) ;
#89759 = ORIENTED_EDGE ( 'NONE', *, *, #19206, .T. ) ;
#89760 = CARTESIAN_POINT ( 'NONE',  ( -56.52287095715004739, -23.94994826722565406, -0.6494450866342736939 ) ) ;
#89761 = ORIENTED_EDGE ( 'NONE', *, *, #89653, .T. ) ;
#89762 = VECTOR ( 'NONE', #950, 1000.000000000000114 ) ;
#89763 = CARTESIAN_POINT ( 'NONE',  ( -13.90609606471210391, -15.62508359690603221, -1.500000000000002220 ) ) ;
#89764 = ADVANCED_FACE ( 'NONE', ( #94514 ), #31610, .T. ) ;
#89765 = CARTESIAN_POINT ( 'NONE',  ( 19.94191871449930531, -9.063712221575384476, 11.49999999999999645 ) ) ;
#89766 = CARTESIAN_POINT ( 'NONE',  ( -37.59388924453935488, -24.15620529776627379, 10.23563542870660825 ) ) ;
#89767 = CARTESIAN_POINT ( 'NONE',  ( -18.84819291449097278, 12.34854029719970825, -1.500000000000002220 ) ) ;
#89768 = CARTESIAN_POINT ( 'NONE',  ( 5.581485548573628996, 20.18083795961418403, 11.49999999999998934 ) ) ;
#89769 = DIRECTION ( 'NONE',  ( -1.000000000000000000, -3.773278334444167608E-23, -8.201307833595939069E-29 ) ) ;
#89770 = CARTESIAN_POINT ( 'NONE',  ( -12.84880425037203011, 5.965225279485592225, -26.59900746623528534 ) ) ;
#89771 = CARTESIAN_POINT ( 'NONE',  ( -119.5532575478694071, -24.51419770103158768, 9.386484678747164523 ) ) ;
#89772 = DIRECTION ( 'NONE',  ( 1.000000000000000000, 0.000000000000000000, 5.238131417152343399E-15 ) ) ;
#89773 = VERTEX_POINT ( 'NONE', #100098 ) ;
#89774 = ADVANCED_FACE ( 'NONE', ( #8783 ), #63084, .F. ) ;
#89775 = ORIENTED_EDGE ( 'NONE', *, *, #91449, .T. ) ;
#89776 = B_SPLINE_CURVE_WITH_KNOTS ( 'NONE', 3,
 ( #23338, #8141, #85248, #94866 ),
 .UNSPECIFIED., .F., .F.,
 ( 4, 4 ),
 ( 0.000000000000000000, 9.999999999998897304E-05 ),
 .UNSPECIFIED. ) ;
#89777 = ORIENTED_EDGE ( 'NONE', *, *, #51482, .F. ) ;
#89778 = EDGE_CURVE ( 'NONE', #81148, #11463, #29956, .T. ) ;
#89779 = CARTESIAN_POINT ( 'NONE',  ( 1.542438661763949392, 0.000000000000000000, 0.000000000000000000 ) ) ;
#89780 = CARTESIAN_POINT ( 'NONE',  ( -12.84383942963603964, -17.20202612561282862, -1.500000000000002220 ) ) ;
#89781 = CARTESIAN_POINT ( 'NONE',  ( -65.05438548721848235, 3.316774720514426456, 29.49402280011861777 ) ) ;
#89782 = EDGE_LOOP ( 'NONE', ( #76373, #49115, #26928, #41474, #80548, #51434 ) ) ;
#89783 = CARTESIAN_POINT ( 'NONE',  ( 19.39439428382967634, -8.317090367284466268, -1.500000000000002220 ) ) ;
#89784 = CARTESIAN_POINT ( 'NONE',  ( -99.91756162674147390, -25.21046098787585521, 3.405294827540925606 ) ) ;
#89785 = CARTESIAN_POINT ( 'NONE',  ( -37.62287095715005592, -23.48783264082477373, -1.443836473390072372 ) ) ;
#89786 = CARTESIAN_POINT ( 'NONE',  ( -109.6228709571500559, -24.64898659630368627, 1.056161002820831474 ) ) ;
#89787 = DIRECTION ( 'NONE',  ( 3.773278334444167608E-23, -1.000000000000000000, 0.000000000000000000 ) ) ;
#89788 = DIRECTION ( 'NONE',  ( 0.7512896232465891000, 1.109416176496795172E-16, 0.6599726524652352877 ) ) ;
#89789 = CARTESIAN_POINT ( 'NONE',  ( 18.88560736741940005, 11.47387103136259690, -1.500000000000002220 ) ) ;
#89790 = CARTESIAN_POINT ( 'NONE',  ( -101.6228709571500559, -29.50250786944525672, 11.44777988621623166 ) ) ;
#89791 = ADVANCED_FACE ( 'NONE', ( #86403 ), #14882, .F. ) ;
#89792 = AXIS2_PLACEMENT_3D ( 'NONE', #35194, #97083, #58532 ) ;
#89793 = DIRECTION ( 'NONE',  ( 0.000000000000000000, 0.000000000000000000, -1.000000000000000000 ) ) ;
#89794 = CARTESIAN_POINT ( 'NONE',  ( -78.62287095715004170, -23.48786465467241413, 11.44779295918254469 ) ) ;
#89795 = DIRECTION ( 'NONE',  ( 1.000000000000000000, -4.089440751051245812E-15, 0.000000000000000000 ) ) ;
#89796 = AXIS2_PLACEMENT_3D ( 'NONE', #21446, #30068, #99564 ) ;
#89797 = CARTESIAN_POINT ( 'NONE',  ( 20.65877813657638740, 5.380652674160894655, 11.49999999999998934 ) ) ;
#89798 = CARTESIAN_POINT ( 'NONE',  ( 22.02124265030973760, -6.376774720514428729, 13.20402280011862395 ) ) ;
#89799 = CARTESIAN_POINT ( 'NONE',  ( -48.86012939852317771, -25.11539320716599377, 2.804431449967496714 ) ) ;
#89800 = CARTESIAN_POINT ( 'NONE',  ( -84.62287095715005592, -24.66019654487199730, 8.947790411086128159 ) ) ;
#89801 = DIRECTION ( 'NONE',  ( 1.000000000000000000, -0.000000000000000000, -0.000000000000000000 ) ) ;
#89802 = CARTESIAN_POINT ( 'NONE',  ( -22.13905560727926414, 4.690293145198261904, -1.500000000000002220 ) ) ;
#89803 = ORIENTED_EDGE ( 'NONE', *, *, #34229, .F. ) ;
#89804 = CARTESIAN_POINT ( 'NONE',  ( 27.53860345374771867, 1.682774720514426114, -9.482392034746240483 ) ) ;
#89805 = CARTESIAN_POINT ( 'NONE',  ( -79.55873559869328915, -23.73766607897669800, -1.055555164236459564 ) ) ;
#89806 = CARTESIAN_POINT ( 'NONE',  ( -19.30086548479123465, -4.275078920326023990, 11.49999999999999645 ) ) ;
#89807 = DIRECTION ( 'NONE',  ( -3.773278334453079030E-23, 0.9999999999976377785, 2.173523156925979128E-06 ) ) ;
#89808 = CARTESIAN_POINT ( 'NONE',  ( -67.51047822507001683, -23.96119346886879953, -0.6495511937832114668 ) ) ;
#89809 = VERTEX_POINT ( 'NONE', #71188 ) ;
#89810 = DIRECTION ( 'NONE',  ( 3.773278334444167608E-23, -1.000000000000000000, 0.000000000000000000 ) ) ;
#89811 = CARTESIAN_POINT ( 'NONE',  ( -29.47844009783932862, -25.26026551470690507, 2.848994710608491854 ) ) ;
#89812 = CARTESIAN_POINT ( 'NONE',  ( 4.621320343559619737, 12.50000000000004974, 0.000000000000000000 ) ) ;
#89813 = CARTESIAN_POINT ( 'NONE',  ( 10.18377579766961283, -19.05927572544859672, -1.500000000000002220 ) ) ;
#89814 = CARTESIAN_POINT ( 'NONE',  ( -49.36186039879741116, -25.10935227259399127, 3.293515131321622658 ) ) ;
#89815 = CARTESIAN_POINT ( 'NONE',  ( -5.843762028675351772, -18.45606589188993141, -1.500000000000002220 ) ) ;
#89816 = CARTESIAN_POINT ( 'NONE',  ( -10.30858931494281450, -5.088649829473331110, 28.47370074478044444 ) ) ;
#89817 = CARTESIAN_POINT ( 'NONE',  ( 30.77564450787170003, 4.772774720514425972, -9.689394075852829857 ) ) ;
#89818 = CARTESIAN_POINT ( 'NONE',  ( -17.81549539028256746, -8.563599010019245839, 11.49999999999998934 ) ) ;
#89819 = EDGE_CURVE ( 'NONE', #95272, #85275, #77205, .T. ) ;
#89820 = ORIENTED_EDGE ( 'NONE', *, *, #89819, .F. ) ;
#89821 = CARTESIAN_POINT ( 'NONE',  ( -16.53579703214142427, -11.71821515807347680, 11.49999999999999645 ) ) ;
#89822 = PLANE ( 'NONE',  #91043 ) ;
#89823 = ADVANCED_FACE ( 'NONE', ( #72194, #35127, #2187 ), #96020, .T. ) ;
#89824 = EDGE_CURVE ( 'NONE', #74588, #88045, #64097, .T. ) ;
#89825 = CARTESIAN_POINT ( 'NONE',  ( 5.920986267150416538, -5.876774720514421624, 21.32549308339960348 ) ) ;
#89826 = EDGE_LOOP ( 'NONE', ( #87526, #17231, #27338, #2392 ) ) ;
#89827 = B_SPLINE_SURFACE_WITH_KNOTS ( 'NONE', 3, 3, ( 
 ( #67781, #98699, #35814, #67275 ),
 ( #82969, #12470, #74369, #52536 ),
 ( #97706, #28200, #59663, #90101 ),
 ( #90593, #20575, #28703, #82478 ),
 ( #12958, #74857, #21564, #21072 ),
 ( #52040, #75357, #5857, #83472 ),
 ( #29195, #13959, #46415, #1252 ) ),
 .UNSPECIFIED., .F., .F., .F.,
 ( 4, 3, 4 ),
 ( 4, 4 ),
 ( 0.0004767105685617169480, 0.1029713956399723879, 0.2054660807113830590 ),
 ( 0.03212754048487516390, 0.03698070728729284384 ),
 .UNSPECIFIED. ) ;
#89828 = CARTESIAN_POINT ( 'NONE',  ( -110.5562042904833930, -24.99132157543166954, 2.256160258750667946 ) ) ;
#89829 = CARTESIAN_POINT ( 'NONE',  ( 32.84232313084847732, 4.840274619473232676, -11.71291885348859196 ) ) ;
#89830 = CARTESIAN_POINT ( 'NONE',  ( -71.52287095715009002, -24.51387760970726148, 9.387446482453414731 ) ) ;
#89831 = DIRECTION ( 'NONE',  ( 0.000000000000000000, 0.000000000000000000, -1.000000000000000000 ) ) ;
#89832 = B_SPLINE_CURVE_WITH_KNOTS ( 'NONE', 3,
 ( #40675, #11219, #87846, #17324, #25439, #10219 ),
 .UNSPECIFIED., .F., .F.,
 ( 4, 2, 4 ),
 ( 1.570755371634033063E-05, 0.001396183895866089921, 0.002776660238015839482 ),
 .UNSPECIFIED. ) ;
#89833 = CARTESIAN_POINT ( 'NONE',  ( -53.52287095715006870, -29.50247984919015209, -1.443849546365058689 ) ) ;
#89834 = CARTESIAN_POINT ( 'NONE',  ( 19.70663390988245922, 3.666079223618853966, 11.49999999999998934 ) ) ;
#89835 = CARTESIAN_POINT ( 'NONE',  ( 1.949999999999999956, -0.1925000000000001710, 0.1924999999999999212 ) ) ;
#89836 = EDGE_LOOP ( 'NONE', ( #34965, #52456, #82483, #43435 ) ) ;
#89837 = CARTESIAN_POINT ( 'NONE',  ( -103.5228709571500758, -23.48786465467241769, 11.44779295918254114 ) ) ;
#89838 = LINE ( 'NONE', #29427, #10532 ) ;
#89839 = CARTESIAN_POINT ( 'NONE',  ( -89.81226385320384509, -25.06732983082694943, 7.447789526168956620 ) ) ;
#89840 = DIRECTION ( 'NONE',  ( -0.000000000000000000, 2.173523156925979552E-06, -0.9999999999976378895 ) ) ;
#89841 = CIRCLE ( 'NONE', #46103, 1.699999999999999289 ) ;
#89842 = EDGE_CURVE ( 'NONE', #94973, #79746, #1611, .T. ) ;
#89843 = EDGE_CURVE ( 'NONE', #16634, #53307, #75959, .T. ) ;
#89844 = DIRECTION ( 'NONE',  ( 0.000000000000000000, 1.000000000000000000, 0.000000000000000000 ) ) ;
#89845 = CARTESIAN_POINT ( 'NONE',  ( -50.02146468009372171, -25.30419751004783535, 5.186272124421678953 ) ) ;
#89846 = ORIENTED_EDGE ( 'NONE', *, *, #6637, .F. ) ;
#89847 = CARTESIAN_POINT ( 'NONE',  ( -9.641467040090685003, 17.89903724589931855, 11.49999999999998934 ) ) ;
#89848 = VERTEX_POINT ( 'NONE', #55973 ) ;
#89849 = CARTESIAN_POINT ( 'NONE',  ( 22.95104020007722667, -0.4190376320207603866, 11.49999999999998934 ) ) ;
#89850 = CARTESIAN_POINT ( 'NONE',  ( -32.62373917829282988, -24.65952944569304606, 1.056160979905696351 ) ) ;
#89851 = CIRCLE ( 'NONE', #54237, 28.96799999999999642 ) ;
#89853 = ORIENTED_EDGE ( 'NONE', *, *, #86992, .T. ) ;
#89852 = ADVANCED_FACE ( 'NONE', ( #95015 ), #49868, .T. ) ;
#89854 = CARTESIAN_POINT ( 'NONE',  ( -108.5228709571501042, -24.66019654487200441, 8.947790411086113949 ) ) ;
#89855 = EDGE_CURVE ( 'NONE', #76180, #72299, #91778, .T. ) ;
#89856 = CARTESIAN_POINT ( 'NONE',  ( -49.27993637813898431, -25.26263991058249658, 6.239168797676713396 ) ) ;
#89857 = DIRECTION ( 'NONE',  ( 0.000000000000000000, 0.000000000000000000, 1.000000000000000000 ) ) ;
#89859 = VERTEX_POINT ( 'NONE', #26004 ) ;
#89858 = CARTESIAN_POINT ( 'NONE',  ( 3.302162439418223627, -20.95225242093645690, 11.49999999999999645 ) ) ;
#89860 = EDGE_LOOP ( 'NONE', ( #8343, #34634, #10148, #51111 ) ) ;
#89861 = CARTESIAN_POINT ( 'NONE',  ( -14.73459587841175633, -16.56598928932902837, 11.49999999999998934 ) ) ;
#89862 = CARTESIAN_POINT ( 'NONE',  ( 17.30552477474510908, -11.17933342135444086, 11.49999999999998934 ) ) ;
#89863 = ORIENTED_EDGE ( 'NONE', *, *, #21471, .F. ) ;
#89864 = EDGE_LOOP ( 'NONE', ( #67578, #81624, #22590, #46700 ) ) ;
#89865 = CARTESIAN_POINT ( 'NONE',  ( 6.826756808399247589, -6.376774720514424288, 21.36722843294932161 ) ) ;
#89866 = CARTESIAN_POINT ( 'NONE',  ( -1.358974358974357921, -5.876774720514419847, 20.75510817307693046 ) ) ;
#89867 = ORIENTED_EDGE ( 'NONE', *, *, #56543, .F. ) ;
#89868 = ORIENTED_EDGE ( 'NONE', *, *, #86852, .T. ) ;
#89869 = ORIENTED_EDGE ( 'NONE', *, *, #42780, .F. ) ;
#89870 = CARTESIAN_POINT ( 'NONE',  ( -111.7766730966630604, -25.29170726702208682, 4.234259702825696969 ) ) ;
#89871 = DIRECTION ( 'NONE',  ( -1.000000000000000000, 0.000000000000000000, 0.000000000000000000 ) ) ;
#89872 = CARTESIAN_POINT ( 'NONE',  ( 32.59332756141814258, 1.477225279485574028, -11.41404606144462086 ) ) ;
#89873 = CARTESIAN_POINT ( 'NONE',  ( 20.56943099487245519, -2.726235779781958968, -1.500000000000002220 ) ) ;
#89874 = EDGE_CURVE ( 'NONE', #75373, #78258, #57977, .T. ) ;
#89875 = CARTESIAN_POINT ( 'NONE',  ( -21.04499429308205549, 5.405531755741471045, 11.49999999999999645 ) ) ;
#89876 = ORIENTED_EDGE ( 'NONE', *, *, #23466, .T. ) ;
#89877 = PLANE ( 'NONE',  #39615 ) ;
#89878 = CARTESIAN_POINT ( 'NONE',  ( -77.58953762381673869, -23.48786465467241413, 11.44779295918254469 ) ) ;
#89879 = CARTESIAN_POINT ( 'NONE',  ( -115.5522256392173261, -24.63355581998386157, 0.9682620441943915468 ) ) ;
#89880 = CARTESIAN_POINT ( 'NONE',  ( -5.254942042970298210, 21.81482460008805546, 11.49999999999998934 ) ) ;
#89881 = B_SPLINE_CURVE_WITH_KNOTS ( 'NONE', 3,
 ( #20488, #59079, #68177, #89513, #89021, #97126, #19497, #67692, #98611, #11888, #50457, #29103, #58087, #59577 ),
 .UNSPECIFIED., .F., .F.,
 ( 4, 2, 2, 2, 2, 2, 4 ),
 ( 8.673617379884035472E-19, 0.0001608593726895868325, 0.0003217187453791727977, 0.0006434374907583468965, 0.0009651562361375208869, 0.001126015608827097636, 0.001286874981516674277 ),
 .UNSPECIFIED. ) ;
#89882 = LINE ( 'NONE', #10259, #10853 ) ;
#89883 = CARTESIAN_POINT ( 'NONE',  ( -65.58633529694422748, -24.63355581998386867, 0.9682620441943842193 ) ) ;
#89884 = VERTEX_POINT ( 'NONE', #19387 ) ;
#89885 = CARTESIAN_POINT ( 'NONE',  ( -70.62287095715007013, -23.47596703998600631, 11.44779298504227505 ) ) ;
#89886 = CARTESIAN_POINT ( 'NONE',  ( -93.62287095715005592, -24.64898659630367916, 1.056161002820827921 ) ) ;
#89887 = AXIS2_PLACEMENT_3D ( 'NONE', #27542, #97539, #38516 ) ;
#89888 = EDGE_LOOP ( 'NONE', ( #87603, #43694, #70391, #56935 ) ) ;
#89889 = VERTEX_POINT ( 'NONE', #11777 ) ;
#89891 = EDGE_CURVE ( 'NONE', #2274, #76771, #42750, .T. ) ;
#89890 = CARTESIAN_POINT ( 'NONE',  ( -69.62287095715005592, -23.48786465467241058, 11.44779295918254824 ) ) ;
#89892 = ORIENTED_EDGE ( 'NONE', *, *, #21172, .T. ) ;
#89893 = CARTESIAN_POINT ( 'NONE',  ( -20.14006130340733236, -7.001243683211865410, -1.500000000000002220 ) ) ;
#89894 = EDGE_CURVE ( 'NONE', #75557, #86771, #41239, .T. ) ;
#89895 = ORIENTED_EDGE ( 'NONE', *, *, #74997, .T. ) ;
#89896 = CARTESIAN_POINT ( 'NONE',  ( -80.55620429048337883, -25.00182538069145721, 7.747789668545097541 ) ) ;
#89897 = CARTESIAN_POINT ( 'NONE',  ( 12.58402814888991372, -17.87355554032721372, -1.500000000000002220 ) ) ;
#89898 = DIRECTION ( 'NONE',  ( -0.000000000000000000, -1.000000000000000000, -0.000000000000000000 ) ) ;
#89899 = CARTESIAN_POINT ( 'NONE',  ( 22.70222466501550329, 0.2752559529566028229, 11.49999999999998934 ) ) ;
#89900 = CARTESIAN_POINT ( 'NONE',  ( 7.475222833218381879, -6.376774720514418959, 20.91460388675487891 ) ) ;
#89901 = CARTESIAN_POINT ( 'NONE',  ( 5.327901167172695907, -5.876774720514418959, 20.73192761314082233 ) ) ;
#89902 = CARTESIAN_POINT ( 'NONE',  ( 21.77894307773758698, -2.757304969434911879, -1.500000000000002220 ) ) ;
#89903 = CARTESIAN_POINT ( 'NONE',  ( 7.166040305186291093, -5.876774720514419847, 20.81030863372915718 ) ) ;
#89904 = ORIENTED_EDGE ( 'NONE', *, *, #31678, .T. ) ;
#89905 = CARTESIAN_POINT ( 'NONE',  ( 29.65385891689261655, -5.748374461104726940, 28.02705487427158104 ) ) ;
#89906 = CARTESIAN_POINT ( 'NONE',  ( -49.13273521788515552, -25.12782683882157642, 6.968846603086977787 ) ) ;
#89907 = EDGE_CURVE ( 'NONE', #31070, #98531, #25099, .T. ) ;
#89908 = EDGE_CURVE ( 'NONE', #12714, #38118, #6657, .T. ) ;
#89909 = ORIENTED_EDGE ( 'NONE', *, *, #45488, .T. ) ;
#89910 = DIRECTION ( 'NONE',  ( -1.226388327005079762E-16, -0.000000000000000000, 1.000000000000000000 ) ) ;
#89911 = CARTESIAN_POINT ( 'NONE',  ( -27.15721599100127648, 5.965225279485572685, -10.22292133548836546 ) ) ;
#89912 = CARTESIAN_POINT ( 'NONE',  ( -0.008165992925886865830, -22.94428480439657037, 3.856996771330998719 ) ) ;
#89913 = CARTESIAN_POINT ( 'NONE',  ( -20.48789480994130230, 5.740754632170482097, 11.49999999999998934 ) ) ;
#89914 = CARTESIAN_POINT ( 'NONE',  ( -112.6270366129879790, -24.15543982623908192, -0.2315651400026420559 ) ) ;
#89915 = CARTESIAN_POINT ( 'NONE',  ( -26.14706027629300422, -24.97064798144177900, 4.097424676804005017 ) ) ;
#89916 = VECTOR ( 'NONE', #75103, 1000.000000000000000 ) ;
#89917 = CARTESIAN_POINT ( 'NONE',  ( -85.54877897942525067, -24.40034930558991277, 0.3402023900116044608 ) ) ;
#89918 = DIRECTION ( 'NONE',  ( 0.000000000000000000, -1.000000000000000000, 0.000000000000000000 ) ) ;
#89919 = CARTESIAN_POINT ( 'NONE',  ( -10.79305683637731406, -5.965225279485594001, -27.49869550653260930 ) ) ;
#89920 = EDGE_LOOP ( 'NONE', ( #33409, #796, #58970, #9018 ) ) ;
#89921 = CARTESIAN_POINT ( 'NONE',  ( -2.459534284235005863, 19.42625828800391119, 11.49999999999999645 ) ) ;
#89922 = CARTESIAN_POINT ( 'NONE',  ( -108.5228709571500616, -24.64965694238408034, 8.947790433994192938 ) ) ;
#89923 = CARTESIAN_POINT ( 'NONE',  ( -68.55620429048339304, -24.64898659630528854, 1.056161002820824368 ) ) ;
#89924 = VERTEX_POINT ( 'NONE', #60472 ) ;
#89925 = B_SPLINE_CURVE_WITH_KNOTS ( 'NONE', 3,
 ( #83297, #38121, #99510, #8185, #92906, #16290, #6675, #31515 ),
 .UNSPECIFIED., .F., .F.,
 ( 4, 2, 2, 4 ),
 ( -0.001224873891641412851, -0.0002244903592271006894, 0.0007758931731872114722, 0.002776660238015839048 ),
 .UNSPECIFIED. ) ;
#89926 = VECTOR ( 'NONE', #70425, 1000.000000000000000 ) ;
#89927 = CARTESIAN_POINT ( 'NONE',  ( -117.5228709571500758, -24.64965694238408034, 8.947790433994191162 ) ) ;
#89928 = CARTESIAN_POINT ( 'NONE',  ( -101.9127759831245612, -25.22330154418774129, 6.417289855096420581 ) ) ;
#89929 = CARTESIAN_POINT ( 'NONE',  ( -42.62287095715004881, -23.48783264082477373, -1.443836473390072817 ) ) ;
#89930 = CARTESIAN_POINT ( 'NONE',  ( -45.62287095715004170, -24.51163499207174468, 0.6490370598554238146 ) ) ;
#89931 = ADVANCED_FACE ( 'NONE', ( #19879 ), #97101, .T. ) ;
#89932 = CARTESIAN_POINT ( 'NONE',  ( -8.027368788987615744, 17.96763083595211441, -1.500000000000002220 ) ) ;
#89933 = ORIENTED_EDGE ( 'NONE', *, *, #43189, .T. ) ;
#89934 = CARTESIAN_POINT ( 'NONE',  ( -28.84663072490566194, 5.965225279485572685, 28.73989617533406715 ) ) ;
#89935 = CARTESIAN_POINT ( 'NONE',  ( -58.87764846858842560, -25.13069340115296058, 2.947789388436138580 ) ) ;
#89936 = PERSON_AND_ORGANIZATION_ROLE ( 'design_supplier' ) ;
#89937 = ORIENTED_EDGE ( 'NONE', *, *, #29950, .F. ) ;
#89938 = CARTESIAN_POINT ( 'NONE',  ( 8.984133506251074763, -0.9496381019629098752, 3.727086380289611700 ) ) ;
#89939 = CARTESIAN_POINT ( 'NONE',  ( -87.52287095715006160, -24.64965694238575011, 8.947790433994196491 ) ) ;
#89940 = CARTESIAN_POINT ( 'NONE',  ( -47.56852929004255515, -23.48783264082478084, -1.443836473390071706 ) ) ;
#89941 = CARTESIAN_POINT ( 'NONE',  ( -118.6258448024444334, -24.15543982623907837, -0.2315651400026558782 ) ) ;
#89942 = CARTESIAN_POINT ( 'NONE',  ( -19.69812919673063689, -0.3587747205143964613, -22.00173861453436430 ) ) ;
#89943 = CARTESIAN_POINT ( 'NONE',  ( -70.25652273905276957, -25.31201591132865403, 5.316156949182883729 ) ) ;
#89944 = CARTESIAN_POINT ( 'NONE',  ( -107.5924963967767667, -23.96119346886881374, -0.6495511937831857097 ) ) ;
#89945 = CARTESIAN_POINT ( 'NONE',  ( -14.87316555497233495, -13.31901947624662519, 11.49999999999998934 ) ) ;
#89946 = DIRECTION ( 'NONE',  ( -1.000000000000000000, 0.000000000000000000, 0.000000000000000000 ) ) ;
#89947 = CARTESIAN_POINT ( 'NONE',  ( -0.09833458469086159282, -21.77698152587677427, -0.5187616176870144535 ) ) ;
#89948 = VERTEX_POINT ( 'NONE', #59459 ) ;
#89949 = CARTESIAN_POINT ( 'NONE',  ( -116.5895376238167103, -23.47596703998600631, 11.44779298504227683 ) ) ;
#89950 = CARTESIAN_POINT ( 'NONE',  ( 10.70203014590133783, -5.295085572968130094, -27.33604350180555187 ) ) ;
#89951 =( LENGTH_UNIT ( ) NAMED_UNIT ( * ) SI_UNIT ( .MILLI., .METRE. ) );
#89952 = CIRCLE ( 'NONE', #94810, 1.399999999999998579 ) ;
#89953 = CARTESIAN_POINT ( 'NONE',  ( 11.40529837384167777, -3.316774720514342967, -28.07356074712937044 ) ) ;
#89954 = CARTESIAN_POINT ( 'NONE',  ( 8.160000000000000142, -6.754662360505033547, 7.925641719537454222 ) ) ;
#89955 = CARTESIAN_POINT ( 'NONE',  ( -107.5562042904833788, -24.66019654487200441, 8.947790411086124607 ) ) ;
#89956 = B_SPLINE_CURVE_WITH_KNOTS ( 'NONE', 3,
 ( #18857, #74638, #58440, #10755, #49835, #89374 ),
 .UNSPECIFIED., .F., .F.,
 ( 4, 2, 4 ),
 ( 1.570755371633679342E-05, 0.001396183895866085151, 0.002776660238015833410 ),
 .UNSPECIFIED. ) ;
#89957 = DIRECTION ( 'NONE',  ( 0.000000000000000000, -0.9967269304714136968, -0.08084198211964954695 ) ) ;
#89958 = CARTESIAN_POINT ( 'NONE',  ( -49.62287095715005592, -23.47593901973091235, -1.443836447539009749 ) ) ;
#89960 = EDGE_CURVE ( 'NONE', #66785, #92874, #89275, .T. ) ;
#89959 = EDGE_LOOP ( 'NONE', ( #47784, #73870, #61314, #13795 ) ) ;
#89961 = PLANE ( 'NONE',  #93278 ) ;
#89962 = CARTESIAN_POINT ( 'NONE',  ( -127.5900869156286745, -23.96119346886880663, -0.6495511937832001426 ) ) ;
#89963 = VERTEX_POINT ( 'NONE', #44239 ) ;
#89964 =( BOUNDED_SURFACE ( )  B_SPLINE_SURFACE ( 3, 2, ( 
 ( #34069, #65043, #27456 ),
 ( #88351, #18825, #49807 ),
 ( #3623, #50297, #17841 ),
 ( #58415, #81233, #80740 ),
 ( #25444, #26947, #2624 ),
 ( #11223, #33563, #42200 ),
 ( #34570, #57916, #48803 ),
 ( #50793, #65540, #56420 ) ),
 .UNSPECIFIED., .F., .F., .F. ) 
 B_SPLINE_SURFACE_WITH_KNOTS ( ( 4, 2, 2, 4 ),
 ( 3, 3 ),
 ( -2.579859069429257801E-16, 0.0001012599413938864427, 0.0002025198827880308713, 0.0004050397655763197284 ),
 ( 0.000000000000000000, 1.000000000000000000 ),
 .UNSPECIFIED. ) 
 GEOMETRIC_REPRESENTATION_ITEM ( )  RATIONAL_B_SPLINE_SURFACE ( (
 ( 1.000000000000000000, 0.8117984224358012479, 1.000000000000000000),
 ( 1.000000000000000000, 0.8431000163380963919, 1.000000000000000000),
 ( 1.000000000000000000, 0.8706302742274230066, 1.000000000000000000),
 ( 1.000000000000000000, 0.9180857590576201321, 1.000000000000000000),
 ( 1.000000000000000000, 0.9379650217685419067, 1.000000000000000000),
 ( 1.000000000000000000, 0.9847826944374993285, 1.000000000000000000),
 ( 1.000000000000000000, 1.000057331645191283, 1.000000000000000000),
 ( 1.000000000000000000, 1.000000000000000000, 1.000000000000000000) ) ) 
 REPRESENTATION_ITEM ( '' )  SURFACE ( )  );
#89965 = CARTESIAN_POINT ( 'NONE',  ( 5.465678960246475704, -19.50585317057041124, -1.500000000000002220 ) ) ;
#89966 = CARTESIAN_POINT ( 'NONE',  ( -28.98875734969026396, -5.965225279485572685, 2.362022800118626531 ) ) ;
#89967 = CARTESIAN_POINT ( 'NONE',  ( -129.6228709571500701, -23.72747288104470442, -1.053458166803223683 ) ) ;
#89968 = EDGE_CURVE ( 'NONE', #62568, #88839, #15388, .T. ) ;
#89969 = EDGE_CURVE ( 'NONE', #19969, #30940, #84277, .T. ) ;
#89970 = CARTESIAN_POINT ( 'NONE',  ( -76.62287095715007013, -24.65952944569304606, 1.056160979905700126 ) ) ;
#89971 = EDGE_CURVE ( 'NONE', #41837, #95120, #95544, .T. ) ;
#89972 = EDGE_LOOP ( 'NONE', ( #88915, #31112, #69419, #75917 ) ) ;
#89973 = CARTESIAN_POINT ( 'NONE',  ( -77.52287095715006160, -24.50321055353804311, 9.387540953477509831 ) ) ;
#89974 = CARTESIAN_POINT ( 'NONE',  ( -29.49975734969026320, 6.475225279485573360, 25.41160796525321430 ) ) ;
#89975 = CARTESIAN_POINT ( 'NONE',  ( -4.751880754313710042, -19.48972053015312866, -1.500000000000002220 ) ) ;
#89976 = CARTESIAN_POINT ( 'NONE',  ( 18.71565868802652588, -9.641079743366450572, 11.49999999999999645 ) ) ;
#89977 = ADVANCED_FACE ( 'NONE', ( #23365 ), #31999, .F. ) ;
#89978 = DIRECTION ( 'NONE',  ( -1.000000000000000000, 0.000000000000000000, 0.000000000000000000 ) ) ;
#89979 = DIRECTION ( 'NONE',  ( -3.773278334453079030E-23, 0.9999999999976377785, 2.173523156925979128E-06 ) ) ;
#89980 = CARTESIAN_POINT ( 'NONE',  ( 20.41560922187292348, 8.460057656491983380, -1.500000000000002220 ) ) ;
#89981 = VECTOR ( 'NONE', #93711, 1000.000000000000114 ) ;
#89982 = LINE ( 'NONE', #12842, #13841 ) ;
#89983 = CARTESIAN_POINT ( 'NONE',  ( -47.62287095715004170, -23.72747288104469732, -1.053458166803227236 ) ) ;
#89984 = PLANE ( 'NONE',  #42799 ) ;
#89985 = ORIENTED_EDGE ( 'NONE', *, *, #72697, .F. ) ;
#89986 = CARTESIAN_POINT ( 'NONE',  ( -69.62287095715005592, -23.47593901973091235, -1.443836447539006196 ) ) ;
#89987 = LINE ( 'NONE', #96110, #14561 ) ;
#89988 = ORIENTED_EDGE ( 'NONE', *, *, #58807, .F. ) ;
#89989 = VERTEX_POINT ( 'NONE', #78651 ) ;
#89990 = CARTESIAN_POINT ( 'NONE',  ( -55.52287095715006160, -23.85196035786899671, -0.8779234886475230093 ) ) ;
#89991 = DIRECTION ( 'NONE',  ( 0.000000000000000000, 0.000000000000000000, -1.000000000000000000 ) ) ;
#89992 = CARTESIAN_POINT ( 'NONE',  ( -61.62287095715004881, -23.47593901973091235, -1.443836447539007972 ) ) ;
#89993 = CARTESIAN_POINT ( 'NONE',  ( -9.157874670058189892, -18.46812626297970539, -1.500000000000002220 ) ) ;
#89994 = EDGE_CURVE ( 'NONE', #67426, #46485, #8118, .T. ) ;
#89995 = CIRCLE ( 'NONE', #31759, 1.306876713926001354 ) ;
#89996 = CARTESIAN_POINT ( 'NONE',  ( 4.073501596442082651, -21.17334570714589859, 11.49999999999999645 ) ) ;
#89997 = ORIENTED_EDGE ( 'NONE', *, *, #60696, .T. ) ;
#89998 = CARTESIAN_POINT ( 'NONE',  ( -83.62287095715009855, -24.33927499327854704, 9.819080762295815390 ) ) ;
#89999 = DIRECTION ( 'NONE',  ( -3.773278334453079618E-23, 0.9999999999976377785, 2.173523156925979975E-06 ) ) ;
#90000 = CARTESIAN_POINT ( 'NONE',  ( 7.160000000000000142, 0.1579206558577706254, 7.788828319098143105 ) ) ;
#90001 = CARTESIAN_POINT ( 'NONE',  ( 17.53502452033532677, 13.85421504792973479, -1.500000000000002220 ) ) ;
#90002 = VECTOR ( 'NONE', #79997, 1000.000000000000114 ) ;
#90003 = CARTESIAN_POINT ( 'NONE',  ( -59.62287095715006302, -23.48786465467241058, 11.44779295918254824 ) ) ;
#90004 = CARTESIAN_POINT ( 'NONE',  ( -50.40445135320378967, -25.13313949306887451, 7.101635536975466678 ) ) ;
#90005 = EDGE_CURVE ( 'NONE', #88484, #50353, #36075, .T. ) ;
#90006 = EDGE_LOOP ( 'NONE', ( #44647, #50818, #74530, #33852 ) ) ;
#90007 = CARTESIAN_POINT ( 'NONE',  ( -124.5228709571500616, -29.50247984919015209, -1.443849546365046699 ) ) ;
#90008 = B_SPLINE_CURVE_WITH_KNOTS ( 'NONE', 3,
 ( #99741, #22621, #45991, #47990, #94144, #31756, #7915, #62724, #1314, #69821 ),
 .UNSPECIFIED., .F., .F.,
 ( 4, 2, 2, 2, 4 ),
 ( 0.000000000000000000, 0.0004275315936953677531, 0.0008550631873907355062, 0.001282594781086103313, 0.001710126374781471012 ),
 .UNSPECIFIED. ) ;
#90009 = CARTESIAN_POINT ( 'NONE',  ( 3.094204744773375815, -5.876774720514422512, 21.02053020447315745 ) ) ;
#90010 = CARTESIAN_POINT ( 'NONE',  ( -20.82246440549779720, 1.468558417816581807, 11.49999999999998934 ) ) ;
#90011 = ORIENTED_EDGE ( 'NONE', *, *, #32773, .F. ) ;
#90014 = EDGE_LOOP ( 'NONE', ( #87382, #26600, #37222, #78020 ) ) ;
#90013 = EDGE_CURVE ( 'NONE', #66931, #20120, #9479, .T. ) ;
#90012 = LINE ( 'NONE', #12869, #76557 ) ;
#90015 = ORIENTED_EDGE ( 'NONE', *, *, #37, .F. ) ;
#90016 = CARTESIAN_POINT ( 'NONE',  ( -100.5881548977521618, -24.63419186844610920, 9.035850630976920428 ) ) ;
#90017 = CARTESIAN_POINT ( 'NONE',  ( -9.620199658202244208, 18.81650055922726494, -1.500000000000002220 ) ) ;
#90018 = VERTEX_POINT ( 'NONE', #99984 ) ;
#90019 = CARTESIAN_POINT ( 'NONE',  ( -91.62287095715004170, -24.66019654487199730, 8.947790411086124607 ) ) ;
#90020 = CARTESIAN_POINT ( 'NONE',  ( -49.46295085228823751, -25.30521617469763740, 5.104712615514442220 ) ) ;
#90021 = CARTESIAN_POINT ( 'NONE',  ( -48.62287095715007723, -24.35013146730204170, 9.818937971375113705 ) ) ;
#90022 = CARTESIAN_POINT ( 'NONE',  ( -67.62287095715005592, -23.47593901973091235, -1.443836447539006196 ) ) ;
#90023 = CARTESIAN_POINT ( 'NONE',  ( -50.38191529551148307, -25.11033443737753146, 2.832404817301930056 ) ) ;
#90024 = CARTESIAN_POINT ( 'NONE',  ( -19.23829340896090656, 10.21096329589227025, -1.500000000000002220 ) ) ;
#90025 = CARTESIAN_POINT ( 'NONE',  ( -81.41053730768496166, -25.12224268930417992, 6.535219352663868442 ) ) ;
#90027 = VERTEX_POINT ( 'NONE', #93387 ) ;
#90026 = CARTESIAN_POINT ( 'NONE',  ( -10.99827004860668822, -19.42154297629913628, 11.49999999999999645 ) ) ;
#90028 = CARTESIAN_POINT ( 'NONE',  ( -57.52287095715004739, -24.35013146730203104, 9.818937971375106599 ) ) ;
#90029 = CARTESIAN_POINT ( 'NONE',  ( 7.116579217368891541, -6.376774720514415407, 20.51774267661129869 ) ) ;
#90030 = DIRECTION ( 'NONE',  ( 0.000000000000000000, -1.000000000000000000, 0.000000000000000000 ) ) ;
#90032 = ORIENTED_EDGE ( 'NONE', *, *, #95823, .T. ) ;
#90031 = EDGE_CURVE ( 'NONE', #70518, #38515, #53847, .T. ) ;
#90033 = EDGE_CURVE ( 'NONE', #1553, #9293, #60963, .T. ) ;
#90034 = EDGE_LOOP ( 'NONE', ( #80118, #71816, #67662, #20470, #47351 ) ) ;
#90035 = ADVANCED_FACE ( 'NONE', ( #84778 ), #54349, .T. ) ;
#90036 = ORIENTED_EDGE ( 'NONE', *, *, #87125, .F. ) ;
#90037 = VECTOR ( 'NONE', #30550, 1000.000000000000000 ) ;
#90038 = CARTESIAN_POINT ( 'NONE',  ( -75.52287095715006160, -25.00158670708909625, 2.256160236439166411 ) ) ;
#90039 = DIRECTION ( 'NONE',  ( 0.000000000000000000, 1.000000000000000000, 0.000000000000000000 ) ) ;
#90040 = CARTESIAN_POINT ( 'NONE',  ( 33.13288845015618023, 0.3587747205144265483, -0.1650522222209214185 ) ) ;
#90041 = B_SPLINE_CURVE_WITH_KNOTS ( 'NONE', 3,
 ( #8536, #70437, #68932, #46102, #45603, #37982 ),
 .UNSPECIFIED., .F., .F.,
 ( 4, 2, 4 ),
 ( 0.000000000000000000, 0.001380901958385393966, 0.002761803916770787931 ),
 .UNSPECIFIED. ) ;
#90042 = CARTESIAN_POINT ( 'NONE',  ( -50.40895856474225667, -25.04307398257883577, 7.563174194274489892 ) ) ;
#90043 = DIRECTION ( 'NONE',  ( 2.352173255807804438E-16, -2.352173255807796056E-16, -1.000000000000000000 ) ) ;
#90044 = PLANE ( 'NONE',  #61974 ) ;
#90045 = ORIENTED_EDGE ( 'NONE', *, *, #83136, .T. ) ;
#90046 = CARTESIAN_POINT ( 'NONE',  ( 19.02374887324148389, -3.781047496429098764, 11.49999999999999645 ) ) ;
#90047 = CARTESIAN_POINT ( 'NONE',  ( -81.55620429048340725, -23.47596703998600276, 11.44779298504227683 ) ) ;
#90048 = ORIENTED_EDGE ( 'NONE', *, *, #38775, .F. ) ;
#90049 = CARTESIAN_POINT ( 'NONE',  ( 3.020285327128866992, -6.376774720514406525, 19.15473963397401391 ) ) ;
#90050 = CARTESIAN_POINT ( 'NONE',  ( 2.710830299132254595, -6.376774720514410077, 19.05039662921485544 ) ) ;
#90051 = FACE_OUTER_BOUND ( 'NONE', #41599, .T. ) ;
#90052 = LINE ( 'NONE', #14409, #8313 ) ;
#90053 = CARTESIAN_POINT ( 'NONE',  ( 13.97609912898263573, 13.72534901313461653, 11.49999999999998934 ) ) ;
#90054 = CARTESIAN_POINT ( 'NONE',  ( -50.37830952628070946, -25.30401792888237367, 5.197789011716579033 ) ) ;
#90055 = EDGE_LOOP ( 'NONE', ( #13001, #63854, #24407, #55456 ) ) ;
#90056 = CARTESIAN_POINT ( 'NONE',  ( 13.05104812959431548, -17.15854754814989391, -1.500000000000002220 ) ) ;
#90057 = CARTESIAN_POINT ( 'NONE',  ( -56.58953762381673158, -24.64898659630528499, 1.056161002820821704 ) ) ;
#90058 = CARTESIAN_POINT ( 'NONE',  ( -69.52287095715006160, -23.48786465467241058, 11.44779295918254647 ) ) ;
#90059 = CARTESIAN_POINT ( 'NONE',  ( -40.56084634221592466, -23.85016227208580730, -0.8807180028928395243 ) ) ;
#90060 = CARTESIAN_POINT ( 'NONE',  ( -104.5228709571500758, -29.50248528299804818, 1.056150453629042030 ) ) ;
#90061 = CARTESIAN_POINT ( 'NONE',  ( 0.2859537766682072601, -23.01552763051285666, -1.500000000000002220 ) ) ;
#90062 = VECTOR ( 'NONE', #53921, 1000.000000000000227 ) ;
#90063 = PERSON_AND_ORGANIZATION ( #70597, #27821 ) ;
#90064 = CARTESIAN_POINT ( 'NONE',  ( 25.61870917940689196, 0.3587747205144265483, 29.49402280011862487 ) ) ;
#90065 = CARTESIAN_POINT ( 'NONE',  ( -4.568292318365942073, 0.3587747205144265483, 30.06720597538392425 ) ) ;
#90066 = CARTESIAN_POINT ( 'NONE',  ( 18.53703574427524359, 7.882278514257341051, 11.49999999999999645 ) ) ;
#90067 = CARTESIAN_POINT ( 'NONE',  ( -66.62287095715005592, -23.47596703998600276, 11.44779298504227683 ) ) ;
#90068 = CARTESIAN_POINT ( 'NONE',  ( -120.6228709571500559, -25.00182538069145721, 7.747789668545100206 ) ) ;
#90069 = VECTOR ( 'NONE', #3187, 1000.000000000000114 ) ;
#90071 = CARTESIAN_POINT ( 'NONE',  ( 7.462166178408539352, -6.475225279485573360, -27.67315496249664974 ) ) ;
#90070 = VECTOR ( 'NONE', #46374, 1000.000000000000000 ) ;
#90072 = CARTESIAN_POINT ( 'NONE',  ( -65.05438548721848235, 6.376774720514426953, 29.49402280011861777 ) ) ;
#90073 = DIRECTION ( 'NONE',  ( 0.000000000000000000, 0.000000000000000000, -1.000000000000000000 ) ) ;
#90074 = CARTESIAN_POINT ( 'NONE',  ( -10.37884456512175291, 16.95428827495986823, 11.49999999999998934 ) ) ;
#90075 = AXIS2_PLACEMENT_3D ( 'NONE', #59343, #35999, #89795 ) ;
#90076 = CARTESIAN_POINT ( 'NONE',  ( -6.660000000000001030, -5.396855673853237919E-16, 5.288828319098142217 ) ) ;
#90077 = CARTESIAN_POINT ( 'NONE',  ( 18.87426695099163254, 5.791883100666666451, -1.500000000000002220 ) ) ;
#90078 = AXIS2_PLACEMENT_3D ( 'NONE', #32937, #63913, #79601 ) ;
#90079 = CARTESIAN_POINT ( 'NONE',  ( -126.5208993246462512, -24.35071581493544102, 9.817618358456011052 ) ) ;
#90080 = B_SPLINE_CURVE_WITH_KNOTS ( 'NONE', 3,
 ( #57013, #87950, #80329, #49402, #10820, #72730, #34166, #65136, #57515, #21405, #66633, #97548, #68602, #44772, #99526, #13797, #75696, #36158, #30024 ),
 .UNSPECIFIED., .F., .F.,
 ( 4, 1, 1, 1, 1, 1, 1, 1, 1, 1, 1, 1, 1, 1, 1, 1, 4 ),
 ( 0.000000000000000000, 0.06815824415599749941, 0.1347066022023570842, 0.2018649976035983007, 0.2707882662774625526, 0.3400242943604910306, 0.4080827390537214439, 0.4768131952581447508, 0.5473460643070945375, 0.5856397954238962145, 0.6288649531777642521, 0.6771532033637908121, 0.7308028113651056090, 0.7898066155325017546, 0.8543250087420143357, 0.9243651340575425035, 1.000000000000000000 ),
 .UNSPECIFIED. ) ;
#90081 = CARTESIAN_POINT ( 'NONE',  ( -1.001577508147789342, -6.376774720514411854, 19.87297243748311004 ) ) ;
#90082 = DIRECTION ( 'NONE',  ( 0.000000000000000000, 1.000000000000000000, 0.000000000000000000 ) ) ;
#90083 = CARTESIAN_POINT ( 'NONE',  ( 12.06641648444584369, 16.80774221200798735, 11.49999999999999645 ) ) ;
#90084 = CARTESIAN_POINT ( 'NONE',  ( -53.55620429048340014, -24.66019654487199020, 8.947790411086135265 ) ) ;
#90085 = LINE ( 'NONE', #74843, #69120 ) ;
#90086 = CARTESIAN_POINT ( 'NONE',  ( -5.639450322166912777, -21.95568564230989850, 11.49999999999999645 ) ) ;
#90087 = ORIENTED_EDGE ( 'NONE', *, *, #29261, .F. ) ;
#90088 = LINE ( 'NONE', #87721, #77051 ) ;
#90090 = EDGE_CURVE ( 'NONE', #32852, #11983, #85790, .T. ) ;
#90089 = CARTESIAN_POINT ( 'NONE',  ( -56.52287095715005449, -23.47593901973090169, -1.443836447538996870 ) ) ;
#90091 = EDGE_CURVE ( 'NONE', #99101, #84227, #2124, .T. ) ;
#90092 = FACE_OUTER_BOUND ( 'NONE', #92512, .T. ) ;
#90093 = EDGE_CURVE ( 'NONE', #90831, #59375, #77157, .T. ) ;
#90094 = CYLINDRICAL_SURFACE ( 'NONE', #33429, 0.3000000000000016542 ) ;
#90095 = EDGE_CURVE ( 'NONE', #29853, #16487, #16272, .T. ) ;
#90096 = ORIENTED_EDGE ( 'NONE', *, *, #20038, .T. ) ;
#90097 = ADVANCED_FACE ( 'NONE', ( #47735 ), #99496, .F. ) ;
#90098 = VERTEX_POINT ( 'NONE', #45728 ) ;
#90099 = DIRECTION ( 'NONE',  ( -0.000000000000000000, 2.173523156925979552E-06, -0.9999999999976378895 ) ) ;
#90100 = CARTESIAN_POINT ( 'NONE',  ( -22.64140897529919272, -3.284158816904186651, -1.500000000000002220 ) ) ;
#90101 = CARTESIAN_POINT ( 'NONE',  ( -29.50322070279044340, -23.87424752075005330, -0.6495508823503305385 ) ) ;
#90102 = CARTESIAN_POINT ( 'NONE',  ( -13.10987527212420645, -17.12674121770768920, -1.500000000000002220 ) ) ;
#90103 = CARTESIAN_POINT ( 'NONE',  ( -113.5144462355907677, -24.66019654487200086, 8.947790411086106843 ) ) ;
#90104 = CARTESIAN_POINT ( 'NONE',  ( -115.6228709571500559, -24.99156045073393173, 7.747789690856161648 ) ) ;
#90105 = CARTESIAN_POINT ( 'NONE',  ( 11.36372850657041589, -19.49111573544105624, 11.49999999999999645 ) ) ;
#90106 = EDGE_LOOP ( 'NONE', ( #55608, #69165, #53479, #10469 ) ) ;
#90107 = CARTESIAN_POINT ( 'NONE',  ( -28.70433822602927876, -24.95898107482323169, 2.741470262984665229 ) ) ;
#90108 = CARTESIAN_POINT ( 'NONE',  ( 19.14557405504459453, -10.84957060938160289, 11.49999999999998934 ) ) ;
#90109 = DIRECTION ( 'NONE',  ( 0.000000000000000000, -0.000000000000000000, 1.000000000000000000 ) ) ;
#90110 = CARTESIAN_POINT ( 'NONE',  ( -41.86995616089613748, -25.29087333980782404, 4.210709713361239004 ) ) ;
#90111 = EDGE_LOOP ( 'NONE', ( #95152, #31823, #74108, #68719 ) ) ;
#90112 = CARTESIAN_POINT ( 'NONE',  ( 0.000000000000000000, -5.876774720514426953, 0.000000000000000000 ) ) ;
#90113 = CYLINDRICAL_SURFACE ( 'NONE', #78608, 0.3000000000000016542 ) ;
#90114 = ORIENTED_EDGE ( 'NONE', *, *, #51496, .T. ) ;
#90115 = CARTESIAN_POINT ( 'NONE',  ( -41.32836283488544638, -5.356774720514427379, 39.26872235229541985 ) ) ;
#90116 = ORIENTED_EDGE ( 'NONE', *, *, #79169, .T. ) ;
#90117 = ORIENTED_EDGE ( 'NONE', *, *, #93228, .T. ) ;
#90118 = CARTESIAN_POINT ( 'NONE',  ( -126.5228709571500616, -24.64898659630368627, 1.056161002820834804 ) ) ;
#90119 = CARTESIAN_POINT ( 'NONE',  ( -87.52287095715006160, -29.50247984919015209, -1.443849546365051806 ) ) ;
#90120 = CARTESIAN_POINT ( 'NONE',  ( 0.000000000000000000, -16.94322527948557422, 0.000000000000000000 ) ) ;
#90121 = CARTESIAN_POINT ( 'NONE',  ( -8.611577853089924517, -18.50786853157798006, -1.500000000000002220 ) ) ;
#90122 = ADVANCED_FACE ( 'NONE', ( #76651 ), #7153, .T. ) ;
#90123 = ORIENTED_EDGE ( 'NONE', *, *, #6911, .F. ) ;
#90124 = CARTESIAN_POINT ( 'NONE',  ( -1.044639546681034536, -5.876774720514417183, 20.34213149456667580 ) ) ;
#90125 = DIRECTION ( 'NONE',  ( -0.000000000000000000, 1.000000000000000000, -0.000000000000000000 ) ) ;
#90126 = VECTOR ( 'NONE', #53144, 1000.000000000000114 ) ;
#90127 = CARTESIAN_POINT ( 'NONE',  ( -105.5855877894006625, -24.92564183028979130, 1.928384488918251316 ) ) ;
#90128 = FACE_OUTER_BOUND ( 'NONE', #32557, .T. ) ;
#90129 = ADVANCED_FACE ( 'NONE', ( #15266 ), #81718, .T. ) ;
#90130 = VERTEX_POINT ( 'NONE', #17783 ) ;
#90131 = DIRECTION ( 'NONE',  ( 0.000000000000000000, 1.000000000000000000, 0.000000000000000000 ) ) ;
#90132 = CARTESIAN_POINT ( 'NONE',  ( -59.56094173781918499, -25.21083105912962097, 3.409327675794633805 ) ) ;
#90133 = ORIENTED_EDGE ( 'NONE', *, *, #24007, .F. ) ;
#90134 = CARTESIAN_POINT ( 'NONE',  ( 17.18838054715250152, -11.71887806637979779, 11.49999999999998934 ) ) ;
#90135 = ORIENTED_EDGE ( 'NONE', *, *, #74142, .T. ) ;
#90137 = ORIENTED_EDGE ( 'NONE', *, *, #47879, .F. ) ;
#90136 = CARTESIAN_POINT ( 'NONE',  ( -101.6367431519704212, -23.48783264082477018, -1.443836473390089248 ) ) ;
#90138 = VECTOR ( 'NONE', #75471, 1000.000000000000000 ) ;
#90139 = CARTESIAN_POINT ( 'NONE',  ( -127.6228709571500275, -24.66019654487199730, 8.947790411086121054 ) ) ;
#90140 = CARTESIAN_POINT ( 'NONE',  ( -128.5228709571500758, -23.48786465467242479, 11.44779295918253581 ) ) ;
#90141 = ORIENTED_EDGE ( 'NONE', *, *, #91593, .F. ) ;
#90142 = ORIENTED_EDGE ( 'NONE', *, *, #93784, .F. ) ;
#90143 = AXIS2_PLACEMENT_3D ( 'NONE', #71532, #26348, #79626 ) ;
#90144 = CARTESIAN_POINT ( 'NONE',  ( -33.52287095715006160, -24.64965694238574656, 8.947790433994207149 ) ) ;
#90145 = CARTESIAN_POINT ( 'NONE',  ( -118.7287200997191405, -25.23482084814633097, 3.690491797311988176 ) ) ;
#90146 = AXIS2_PLACEMENT_3D ( 'NONE', #22887, #99025, #91417 ) ;
#90147 = CARTESIAN_POINT ( 'NONE',  ( -80.62287095715007013, -25.00158670708909625, 2.256160236439165967 ) ) ;
#90148 = CARTESIAN_POINT ( 'NONE',  ( -43.52203307092815265, -23.48786465467240347, 11.44779295918255180 ) ) ;
#90150 = ORIENTED_EDGE ( 'NONE', *, *, #20612, .T. ) ;
#90149 = CARTESIAN_POINT ( 'NONE',  ( -4.315754209668272168, 21.71352930684897942, 11.49999999999999645 ) ) ;
#90151 = AXIS2_PLACEMENT_3D ( 'NONE', #72714, #96040, #27535 ) ;
#90152 = LINE ( 'NONE', #23611, #61837 ) ;
#90153 = CARTESIAN_POINT ( 'NONE',  ( -21.41681981171885951, -7.298096547245328303, 11.49999999999998934 ) ) ;
#90154 = EDGE_CURVE ( 'NONE', #46797, #79998, #80178, .T. ) ;
#90156 = ORIENTED_EDGE ( 'NONE', *, *, #50341, .T. ) ;
#90155 = CARTESIAN_POINT ( 'NONE',  ( -115.6284348552737811, -24.15602025860897584, 10.28564288303533836 ) ) ;
#90157 = EDGE_LOOP ( 'NONE', ( #67270, #97724, #22492, #91638 ) ) ;
#90158 = B_SPLINE_CURVE_WITH_KNOTS ( 'NONE', 3,
 ( #96097, #18461, #65171, #57546 ),
 .UNSPECIFIED., .F., .F.,
 ( 4, 4 ),
 ( 0.000000000000000000, 9.999999999998897304E-05 ),
 .UNSPECIFIED. ) ;
#90159 = CARTESIAN_POINT ( 'NONE',  ( -80.85430032345135487, -25.31559690359951631, 5.016450530977278000 ) ) ;
#90160 = ADVANCED_FACE ( 'NONE', ( #79668 ), #21790, .T. ) ;
#90161 = B_SPLINE_CURVE_WITH_KNOTS ( 'NONE', 3,
 ( #87907, #94509, #80288, #94004, #10782, #63587, #72687, #24990, #62572, #9773, #12760, #42745, #89900, #89402, #19382 ),
 .UNSPECIFIED., .F., .F.,
 ( 4, 1, 1, 1, 1, 1, 1, 1, 1, 1, 1, 1, 4 ),
 ( 0.000000000000000000, 0.08433472199262730118, 0.1670523184160740138, 0.2495660772409658001, 0.3327404818018465660, 0.4159148863627275539, 0.4978280095399964522, 0.5803725886080518537, 0.6646001210565030126, 0.7494666931126164888, 0.8325102339401410090, 0.9156392816681726554, 1.000000000000000000 ),
 .UNSPECIFIED. ) ;
#90162 = DIRECTION ( 'NONE',  ( 0.000000000000000000, 0.000000000000000000, -1.000000000000000000 ) ) ;
#90163 = ORIENTED_EDGE ( 'NONE', *, *, #91709, .F. ) ;
#90164 = CARTESIAN_POINT ( 'NONE',  ( -103.5228709571500758, -24.64965694238408034, 8.947790433994194714 ) ) ;
#90165 = CARTESIAN_POINT ( 'NONE',  ( 20.80681148587913754, 8.022540738981085440, -1.500000000000002220 ) ) ;
#90166 = CARTESIAN_POINT ( 'NONE',  ( -50.22356044790234364, -25.13941496013254095, 7.558302963627013149 ) ) ;
#90167 = VERTEX_POINT ( 'NONE', #75046 ) ;
#90168 = LINE ( 'NONE', #34889, #67603 ) ;
#90169 = DIRECTION ( 'NONE',  ( 1.000000000000000000, 3.773278334444166432E-23, 8.201307841325785021E-29 ) ) ;
#90170 = DIRECTION ( 'NONE',  ( 0.000000000000000000, 0.000000000000000000, -1.000000000000000000 ) ) ;
#90171 = AXIS2_PLACEMENT_3D ( 'NONE', #37755, #68714, #62601 ) ;
#90172 = CARTESIAN_POINT ( 'NONE',  ( -84.62287095715004170, -24.65952944569304606, 1.056160979905699460 ) ) ;
#90173 = DIRECTION ( 'NONE',  ( 0.000000000000000000, -0.000000000000000000, -1.000000000000000000 ) ) ;
#90174 = CARTESIAN_POINT ( 'NONE',  ( -19.43040671759091609, -1.856541507571394467, -1.500000000000002220 ) ) ;
#90175 = CARTESIAN_POINT ( 'NONE',  ( 14.05358622956002357, 16.19628355576825385, 11.49999999999998934 ) ) ;
#90176 = FACE_OUTER_BOUND ( 'NONE', #37303, .T. ) ;
#90177 = DIRECTION ( 'NONE',  ( -0.000000000000000000, 1.000000000000000000, -0.000000000000000000 ) ) ;
#90178 = FACE_BOUND ( 'NONE', #27835, .T. ) ;
#90179 = CARTESIAN_POINT ( 'NONE',  ( -5.953223121155255981, 22.05028593715628560, -1.500000000000002220 ) ) ;
#90180 = APPROVAL_DATE_TIME ( #59237, #29008 ) ;
#90181 = DIRECTION ( 'NONE',  ( 0.000000000000000000, 0.000000000000000000, -1.000000000000000000 ) ) ;
#90182 = CARTESIAN_POINT ( 'NONE',  ( -128.5228709571500758, -24.33832256527048798, 0.1851278514138663678 ) ) ;
#90183 = CARTESIAN_POINT ( 'NONE',  ( 14.90458806734895703, -13.33898509196910886, 11.49999999999999645 ) ) ;
#90184 = CARTESIAN_POINT ( 'NONE',  ( 4.444543648262985869, 12.92677669529668627, 0.000000000000000000 ) ) ;
#90185 = CARTESIAN_POINT ( 'NONE',  ( -74.54207935781894889, -24.51419770103157703, 9.386484678747164523 ) ) ;
#90186 = CARTESIAN_POINT ( 'NONE',  ( -48.51406547070947539, -23.73766607897670866, -1.055555164236436028 ) ) ;
#90187 = ORIENTED_EDGE ( 'NONE', *, *, #34564, .T. ) ;
#90188 = CARTESIAN_POINT ( 'NONE',  ( -26.12160690352767389, -24.70321153058107910, 2.461338914291016255 ) ) ;
#90189 = CARTESIAN_POINT ( 'NONE',  ( -65.52287095715006160, -23.48786465467241058, 11.44779295918254647 ) ) ;
#90190 = CARTESIAN_POINT ( 'NONE',  ( 13.45394552336293614, 17.01807010946250287, -1.500000000000002220 ) ) ;
#90191 = FACE_BOUND ( 'NONE', #24106, .T. ) ;
#90192 = CARTESIAN_POINT ( 'NONE',  ( -19.51626497420292239, -0.3564122556526727048, -1.500000000000002220 ) ) ;
#90193 = VECTOR ( 'NONE', #94667, 1000.000000000000000 ) ;
#90194 = CARTESIAN_POINT ( 'NONE',  ( 30.93860345374796594, -6.475225279485573360, 28.07639619989136293 ) ) ;
#90195 = EDGE_LOOP ( 'NONE', ( #83741, #9715, #99823, #69585 ) ) ;
#90196 = PERSON_AND_ORGANIZATION ( #23494, #27961 ) ;
#90197 = LINE ( 'NONE', #20178, #14324 ) ;
#90198 = CARTESIAN_POINT ( 'NONE',  ( -65.55620429048339304, -23.47596703998600276, 11.44779298504227505 ) ) ;
#90199 = CARTESIAN_POINT ( 'NONE',  ( 8.813945691637787405, 18.49579627399651471, 11.49999999999999645 ) ) ;
#90200 = CARTESIAN_POINT ( 'NONE',  ( 16.15056352287345121, 3.622774720514426949, -27.77856273171767398 ) ) ;
#90201 = VECTOR ( 'NONE', #52398, 1000.000000000000114 ) ;
#90202 = CARTESIAN_POINT ( 'NONE',  ( -84.62287095715005592, -29.50250243563736774, 8.947779886222141599 ) ) ;
#90203 = VERTEX_POINT ( 'NONE', #66487 ) ;
#90204 = CARTESIAN_POINT ( 'NONE',  ( -109.8274915671167093, -25.30623678762077233, 5.180956911978509716 ) ) ;
#90205 = CARTESIAN_POINT ( 'NONE',  ( -86.52287095715006160, -24.64898659630367916, 1.056161002820827921 ) ) ;
#90206 = AXIS2_PLACEMENT_3D ( 'NONE', #53095, #6901, #30231 ) ;
#90208 = ADVANCED_FACE ( 'NONE', ( #43122 ), #12655, .T. ) ;
#90207 = LINE ( 'NONE', #21672, #59785 ) ;
#90209 = VECTOR ( 'NONE', #44977, 1000.000000000000000 ) ;
#90210 = LINE ( 'NONE', #15078, #92145 ) ;
#90212 = ORIENTED_EDGE ( 'NONE', *, *, #83716, .T. ) ;
#90211 = EDGE_CURVE ( 'NONE', #24849, #92377, #11807, .T. ) ;
#90213 = CARTESIAN_POINT ( 'NONE',  ( 5.641575934020636396, -6.376774720514420736, 20.76276410292889096 ) ) ;
#90214 = VECTOR ( 'NONE', #62895, 1000.000000000000114 ) ;
#90215 = ADVANCED_FACE ( 'NONE', ( #35995 ), #83161, .T. ) ;
#90216 = CARTESIAN_POINT ( 'NONE',  ( -21.75560140871883164, 7.562747417745157463, 11.49999999999999645 ) ) ;
#90217 = CARTESIAN_POINT ( 'NONE',  ( -22.52399778787742335, 3.408274809117095572, 11.49999999999998934 ) ) ;
#90218 = LINE ( 'NONE', #13076, #74607 ) ;
#90219 = ADVANCED_FACE ( 'NONE', ( #35512 ), #43619, .T. ) ;
#90220 = CARTESIAN_POINT ( 'NONE',  ( -2.169994883066378222, 10.75358048763951047, -3.549999999999999822 ) ) ;
#90221 = CARTESIAN_POINT ( 'NONE',  ( -61.64687923781919920, -25.13069339737145214, 2.947789366383932297 ) ) ;
#90222 = CARTESIAN_POINT ( 'NONE',  ( -115.5228709571500474, -24.63287334234179937, 0.9662140553045351909 ) ) ;
#90223 = EDGE_CURVE ( 'NONE', #14365, #61087, #81679, .T. ) ;
#90224 = CARTESIAN_POINT ( 'NONE',  ( -104.2228709571500644, -23.47596703998600631, 11.44779298504227860 ) ) ;
#90225 = CARTESIAN_POINT ( 'NONE',  ( -16.46405638241306946, -14.47283864684382237, -1.500000000000002220 ) ) ;
#90226 = DIRECTION ( 'NONE',  ( 1.000000000000000000, 3.773278334444167608E-23, 8.201307833595939069E-29 ) ) ;
#90227 = DIRECTION ( 'NONE',  ( 0.000000000000000000, -0.9999999999976377785, -2.173523156925979975E-06 ) ) ;
#90228 = CARTESIAN_POINT ( 'NONE',  ( -71.20541289166536103, -25.30502758240210071, 4.885889971059796721 ) ) ;
#90229 = CARTESIAN_POINT ( 'NONE',  ( -58.62366805386946567, -24.65952944569304606, 1.056160979905697461 ) ) ;
#90230 = ORIENTED_EDGE ( 'NONE', *, *, #56433, .T. ) ;
#90231 = CARTESIAN_POINT ( 'NONE',  ( 18.81987132735423174, -8.002443037797982939, 11.49999999999998934 ) ) ;
#90232 = ORIENTED_EDGE ( 'NONE', *, *, #45929, .F. ) ;
#90233 = ORIENTED_EDGE ( 'NONE', *, *, #34693, .T. ) ;
#90234 = ORIENTED_EDGE ( 'NONE', *, *, #43978, .F. ) ;
#90235 = ORIENTED_EDGE ( 'NONE', *, *, #36044, .F. ) ;
#90236 = CARTESIAN_POINT ( 'NONE',  ( -13.44081803467414638, 18.71018530922267686, -1.500000000000002220 ) ) ;
#90237 = CARTESIAN_POINT ( 'NONE',  ( -95.58953762381672448, -25.00158670708909625, 2.256160236439167299 ) ) ;
#90238 = CARTESIAN_POINT ( 'NONE',  ( -2.107266074560359748, -20.09985696230311447, -1.500000000000002220 ) ) ;
#90239 = ORIENTED_EDGE ( 'NONE', *, *, #61831, .T. ) ;
#90240 = CIRCLE ( 'NONE', #91825, 28.96799999999999642 ) ;
#90241 = CARTESIAN_POINT ( 'NONE',  ( -98.62287095715002749, -23.72773821059535848, 11.05748984161097326 ) ) ;
#90242 = CARTESIAN_POINT ( 'NONE',  ( -41.73392779468957769, -25.31439885490801345, 4.813727054875380773 ) ) ;
#90243 = EDGE_CURVE ( 'NONE', #84363, #62727, #3390, .T. ) ;
#90244 = CARTESIAN_POINT ( 'NONE',  ( -118.6228709571500559, -29.50248528299804818, 1.056150453629045360 ) ) ;
#90245 = CARTESIAN_POINT ( 'NONE',  ( -99.54653281135311715, -24.66019654487200086, 8.947790411086117501 ) ) ;
#90247 = VERTEX_POINT ( 'NONE', #66970 ) ;
#90246 = CARTESIAN_POINT ( 'NONE',  ( -15.65470850568805083, 14.63654280257262386, 11.49999999999999645 ) ) ;
#90248 = LINE ( 'NONE', #76500, #59779 ) ;
#90249 = ORIENTED_EDGE ( 'NONE', *, *, #99289, .T. ) ;
#90250 = AXIS2_PLACEMENT_3D ( 'NONE', #76775, #22493, #39231 ) ;
#90251 = CARTESIAN_POINT ( 'NONE',  ( 11.91227609878784399, -18.80521639033699799, 11.49999999999998934 ) ) ;
#90252 = CARTESIAN_POINT ( 'NONE',  ( 15.29587703590233971, -13.95322596517325664, 11.49999999999998934 ) ) ;
#90253 = B_SPLINE_CURVE_WITH_KNOTS ( 'NONE', 3,
 ( #1147, #15853, #9245, #78247 ),
 .UNSPECIFIED., .F., .F.,
 ( 4, 4 ),
 ( 0.8811291927886271136, 0.8901356240607424253 ),
 .UNSPECIFIED. ) ;
#90254 = ORIENTED_EDGE ( 'NONE', *, *, #14474, .T. ) ;
#90255 = CARTESIAN_POINT ( 'NONE',  ( -28.60235993766668017, -23.80466053152675698, -0.6495505116914124244 ) ) ;
#90256 = VERTEX_POINT ( 'NONE', #67960 ) ;
#90257 = CARTESIAN_POINT ( 'NONE',  ( -74.62287095715005592, -29.50250786944525672, 11.44777988621623699 ) ) ;
#90258 = ORIENTED_EDGE ( 'NONE', *, *, #16697, .T. ) ;
#90259 = CARTESIAN_POINT ( 'NONE',  ( 17.09260067683297635, -12.12037977771017871, -1.500000000000002220 ) ) ;
#90260 = CARTESIAN_POINT ( 'NONE',  ( 6.672210613628693388, 20.84999943921648935, 11.49999999999999645 ) ) ;
#90261 = CARTESIAN_POINT ( 'NONE',  ( -37.48483847649136891, -24.51419770103156637, 9.386484678747175181 ) ) ;
#90262 = CARTESIAN_POINT ( 'NONE',  ( -11.40494320173684351, 19.43794304404440254, 11.49999999999998934 ) ) ;
#90263 = VECTOR ( 'NONE', #73950, 1000.000000000000000 ) ;
#90264 = CARTESIAN_POINT ( 'NONE',  ( 20.69369447470243628, -3.267675865747468489, -1.500000000000002220 ) ) ;
#90265 = DIRECTION ( 'NONE',  ( 0.9161084732596777025, 7.885106708985488048E-16, -0.4009304992412306978 ) ) ;
#90266 = B_SPLINE_CURVE_WITH_KNOTS ( 'NONE', 3,
 ( #37400, #30776, #15042, #83556 ),
 .UNSPECIFIED., .F., .F.,
 ( 4, 4 ),
 ( 0.000000000000000000, 1.000000000000000000 ),
 .UNSPECIFIED. ) ;
#90267 = CARTESIAN_POINT ( 'NONE',  ( -119.5222409990807506, -23.48786465467241769, 11.44779295918253759 ) ) ;
#90268 = CARTESIAN_POINT ( 'NONE',  ( 5.654014271574485662, -6.376774720514420736, 20.92503208403226722 ) ) ;
#90269 = ORIENTED_EDGE ( 'NONE', *, *, #94259, .T. ) ;
#90270 = ORIENTED_EDGE ( 'NONE', *, *, #78404, .T. ) ;
#90271 = ORIENTED_EDGE ( 'NONE', *, *, #72637, .F. ) ;
#90272 = PLANE ( 'NONE',  #1227 ) ;
#90273 = AXIS2_PLACEMENT_3D ( 'NONE', #43058, #3006, #26824 ) ;
#90274 = CARTESIAN_POINT ( 'NONE',  ( -14.42888051209446409, 15.91495273949476363, -1.500000000000002220 ) ) ;
#90275 = ADVANCED_FACE ( 'NONE', ( #73570 ), #13644, .T. ) ;
#90276 = CARTESIAN_POINT ( 'NONE',  ( -121.5228709571500190, -24.66019654487199730, 8.947790411086119278 ) ) ;
#90278 = ORIENTED_EDGE ( 'NONE', *, *, #34135, .T. ) ;
#90277 = VECTOR ( 'NONE', #16001, 1000.000000000000000 ) ;
#90279 = CARTESIAN_POINT ( 'NONE',  ( 11.07546443054301655, -17.96822238807187233, 11.49999999999998934 ) ) ;
#90280 = CARTESIAN_POINT ( 'NONE',  ( 21.57151214508649772, -0.8999999999999998002, 0.000000000000000000 ) ) ;
#90281 = DIRECTION ( 'NONE',  ( -0.5658830507178048697, 0.000000000000000000, 0.8244855201338046058 ) ) ;
#90282 = DIRECTION ( 'NONE',  ( 0.000000000000000000, 1.000000000000000000, 0.000000000000000000 ) ) ;
#90283 = AXIS2_PLACEMENT_3D ( 'NONE', #16642, #32884, #8540 ) ;
#90284 = CARTESIAN_POINT ( 'NONE',  ( 10.22568704553358643, -6.475225279485576024, -27.02513721610328901 ) ) ;
#90285 = CARTESIAN_POINT ( 'NONE',  ( -37.52287095715006870, -23.47596703998600631, 11.44779298504229281 ) ) ;
#90286 = CARTESIAN_POINT ( 'NONE',  ( -17.14978611337857473, 13.99085498846200437, -1.500000000000002220 ) ) ;
#90287 = CARTESIAN_POINT ( 'NONE',  ( -108.8968792378191921, -25.14264220134206695, 6.986250900936221697 ) ) ;
#90288 = EDGE_CURVE ( 'NONE', #67166, #60099, #37078, .T. ) ;
#90289 = CARTESIAN_POINT ( 'NONE',  ( -108.9606173779806682, -25.28716625322443790, 4.328991613801438376 ) ) ;
#90290 = CARTESIAN_POINT ( 'NONE',  ( 30.53060340732035982, 4.594240983522013266, 19.84760796525321780 ) ) ;
#90291 = CARTESIAN_POINT ( 'NONE',  ( -97.52287095715011844, -24.33927499327856125, 9.819080762295813614 ) ) ;
#90292 = CARTESIAN_POINT ( 'NONE',  ( 14.64286990871793392, 12.78475832571431070, -1.500000000000002220 ) ) ;
#90293 = CARTESIAN_POINT ( 'NONE',  ( 18.88549913130557556, 9.949676122998861061, 11.49999999999998934 ) ) ;
#90294 = DIRECTION ( 'NONE',  ( 0.000000000000000000, 0.000000000000000000, 1.000000000000000000 ) ) ;
#90295 = CARTESIAN_POINT ( 'NONE',  ( -51.94775699965006766, -25.32724633150699489, 4.398074151685129607 ) ) ;
#90296 = DIRECTION ( 'NONE',  ( 0.000000000000000000, -2.173523156925979552E-06, 0.9999999999976378895 ) ) ;
#90297 = DIRECTION ( 'NONE',  ( 1.000000000000000000, -7.960204194457801640E-17, 0.000000000000000000 ) ) ;
#90298 = CC_DESIGN_DATE_AND_TIME_ASSIGNMENT ( #50642, #50150, ( #14993 ) ) ;
#90299 = CARTESIAN_POINT ( 'NONE',  ( -15.94491270116497184, -16.04792668696150315, -1.500000000000002220 ) ) ;
#90300 = EDGE_LOOP ( 'NONE', ( #70814, #9118, #46851, #37378, #69647, #18530, #45303, #50064, #18619, #89475, #1890, #67525, #20633, #11761, #95364, #90859, #34492, #62065, #13402, #17475, #32727, #2631, #7621, #66, #62492, #36102, #63972 ) ) ;
#90301 = CARTESIAN_POINT ( 'NONE',  ( -87.52287095715010423, -24.35013146730204170, 9.818937971375099494 ) ) ;
#90302 = CARTESIAN_POINT ( 'NONE',  ( -104.6228709571500559, -24.64965695001468404, 8.947790433994178727 ) ) ;
#90303 = CARTESIAN_POINT ( 'NONE',  ( -7.851535696030730982, 18.15458241006858131, 11.49999999999999645 ) ) ;
#90304 = CARTESIAN_POINT ( 'NONE',  ( -29.49875734969026198, -5.965225279485572685, 10.11402280011862587 ) ) ;
#90305 = B_SPLINE_CURVE_WITH_KNOTS ( 'NONE', 3,
 ( #46288, #15323, #30051, #61027, #69121, #77217, #69634, #22429 ),
 .UNSPECIFIED., .F., .F.,
 ( 4, 2, 2, 4 ),
 ( -0.001240666984356056596, -0.0002401179793396612111, 0.0007604310256767346076, 0.002761529035709530365 ),
 .UNSPECIFIED. ) ;
#90306 = CARTESIAN_POINT ( 'NONE',  ( -76.62287095715007013, -23.48783264082478084, -1.443836473390065489 ) ) ;
#90307 = ORIENTED_EDGE ( 'NONE', *, *, #2278, .T. ) ;
#90308 = CARTESIAN_POINT ( 'NONE',  ( 0.1645010273463760886, -0.3687607960183646449, -1.417169167140628350 ) ) ;
#90309 = CARTESIAN_POINT ( 'NONE',  ( -29.81001385051325414, -25.26026941986502550, 4.645689688962429287 ) ) ;
#90310 = CARTESIAN_POINT ( 'NONE',  ( -100.9506922656100727, -25.12268545600608860, 7.008856018889373374 ) ) ;
#90311 = CARTESIAN_POINT ( 'NONE',  ( -19.46174652491427182, -9.421329337880418819, -1.500000000000002220 ) ) ;
#90312 = AXIS2_PLACEMENT_3D ( 'NONE', #36114, #95514, #75166 ) ;
#90313 = CARTESIAN_POINT ( 'NONE',  ( 30.45304879119406039, -4.772774720514425972, -10.07140455160086390 ) ) ;
#90314 = CARTESIAN_POINT ( 'NONE',  ( -9.862393454161701101, 16.67994275214481092, -1.500000000000002220 ) ) ;
#90315 = LINE ( 'NONE', #28405, #15657 ) ;
#90316 = CARTESIAN_POINT ( 'NONE',  ( -40.62287095715004170, -24.99156045073392463, 7.747789690856161648 ) ) ;
#90317 = CARTESIAN_POINT ( 'NONE',  ( -7.013475202606065828, -18.52788797337992222, 11.49999999999998934 ) ) ;
#90318 = VERTEX_POINT ( 'NONE', #97400 ) ;
#90319 = VECTOR ( 'NONE', #24020, 1000.000000000000000 ) ;
#90320 = CARTESIAN_POINT ( 'NONE',  ( -17.45352675615719917, 10.31968153043333380, 11.49999999999999645 ) ) ;
#90321 = CARTESIAN_POINT ( 'NONE',  ( -58.62287095715004881, -29.50247984919015209, -1.443849546365056913 ) ) ;
#90322 = DIRECTION ( 'NONE',  ( 0.000000000000000000, 0.000000000000000000, 1.000000000000000000 ) ) ;
#90323 = ORIENTED_EDGE ( 'NONE', *, *, #63603, .F. ) ;
#90324 = DIRECTION ( 'NONE',  ( 0.000000000000000000, 0.000000000000000000, 1.000000000000000000 ) ) ;
#90325 = CARTESIAN_POINT ( 'NONE',  ( 31.63207147031214106, 3.934018429836814601, 27.19231918963763661 ) ) ;
#90326 = CARTESIAN_POINT ( 'NONE',  ( -99.52287095715006160, -23.48786465467241769, 11.44779295918254114 ) ) ;
#90327 = CARTESIAN_POINT ( 'NONE',  ( 22.81105451610979173, -2.682774720514426559, -18.46691820600746681 ) ) ;
#90328 = PLANE ( 'NONE',  #72222 ) ;
#90329 = CARTESIAN_POINT ( 'NONE',  ( -10.05502934987021391, 17.38067806581081598, -1.500000000000002220 ) ) ;
#90330 = DIRECTION ( 'NONE',  ( 0.000000000000000000, -1.478457507934778393E-16, -1.000000000000000000 ) ) ;
#90331 = ORIENTED_EDGE ( 'NONE', *, *, #87945, .F. ) ;
#90332 = CIRCLE ( 'NONE', #9340, 1.149999999999998135 ) ;
#90333 = CARTESIAN_POINT ( 'NONE',  ( 22.28265747778879202, 5.072132558558076099, 11.49999999999999645 ) ) ;
#90334 = CARTESIAN_POINT ( 'NONE',  ( -49.50841769935764347, -25.26258722004150670, 3.984447755610470487 ) ) ;
#90335 = EDGE_CURVE ( 'NONE', #87641, #3446, #21752, .T. ) ;
#90336 = CARTESIAN_POINT ( 'NONE',  ( -127.5228709571500900, -23.72747288104470798, -1.053458166803224572 ) ) ;
#90337 = FACE_OUTER_BOUND ( 'NONE', #29575, .T. ) ;
#90338 = B_SPLINE_CURVE_WITH_KNOTS ( 'NONE', 3,
 ( #69644, #14336, #76235, #45313, #92460, #46298 ),
 .UNSPECIFIED., .F., .F.,
 ( 4, 2, 4 ),
 ( 1.570755371634131319E-05, 0.001396183895866088404, 0.002776660238015835579 ),
 .UNSPECIFIED. ) ;
#90339 = ADVANCED_FACE ( 'NONE', ( #59850 ), #30749, .T. ) ;
#90340 = CARTESIAN_POINT ( 'NONE',  ( -71.52287095715007581, -24.64898659630528854, 1.056161002820824368 ) ) ;
#90341 = VECTOR ( 'NONE', #79004, 1000.000000000000114 ) ;
#90342 = LINE ( 'NONE', #5604, #73755 ) ;
#90343 = CARTESIAN_POINT ( 'NONE',  ( -16.61153998044026991, -15.06042057022924929, 11.49999999999999645 ) ) ;
#90344 = CARTESIAN_POINT ( 'NONE',  ( -74.62287095715005592, -24.64898659630367561, 1.056161002820824368 ) ) ;
#90345 = ORIENTED_EDGE ( 'NONE', *, *, #15917, .F. ) ;
#90346 = VECTOR ( 'NONE', #39602, 1000.000000000000114 ) ;
#90347 = CARTESIAN_POINT ( 'NONE',  ( -11.21218820807429140, -16.99972530465495169, 11.49999999999998934 ) ) ;
#90348 = EDGE_LOOP ( 'NONE', ( #27071, #89636, #5918, #6746 ) ) ;
#90349 = ADVANCED_FACE ( 'NONE', ( #29879 ), #7230, .T. ) ;
#90350 = CARTESIAN_POINT ( 'NONE',  ( 2.177599385301639323, -22.86303409451243596, -1.500000000000002220 ) ) ;
#90351 = LINE ( 'NONE', #45681, #97148 ) ;
#90352 = VERTEX_POINT ( 'NONE', #92273 ) ;
#90353 = CARTESIAN_POINT ( 'NONE',  ( -109.5228709571500758, -24.51283580621365488, 0.6167428607019762588 ) ) ;
#90354 = CARTESIAN_POINT ( 'NONE',  ( -116.5228709571500616, -23.48786465467241769, 11.44779295918253759 ) ) ;
#90355 = CARTESIAN_POINT ( 'NONE',  ( 282.9764569301858046, -6.475225279485573360, 20.79159422840526616 ) ) ;
#90357 = ORIENTED_EDGE ( 'NONE', *, *, #63224, .F. ) ;
#90356 = CARTESIAN_POINT ( 'NONE',  ( 9.297385241821217505, 19.04214385377821017, 11.49999999999999645 ) ) ;
#90358 = VERTEX_POINT ( 'NONE', #31382 ) ;
#90359 = CARTESIAN_POINT ( 'NONE',  ( -18.13406196532287140, 12.77545654309102474, -1.500000000000002220 ) ) ;
#90360 = CARTESIAN_POINT ( 'NONE',  ( 20.58124611042576646, 0.8182449333618511123, -1.500000000000002220 ) ) ;
#90361 = EDGE_LOOP ( 'NONE', ( #90393, #40593, #82837, #39783 ) ) ;
#90362 = ORIENTED_EDGE ( 'NONE', *, *, #84148, .T. ) ;
#90363 = DIRECTION ( 'NONE',  ( 0.000000000000000000, 2.173523156925980399E-06, -0.9999999999976378895 ) ) ;
#90364 = CARTESIAN_POINT ( 'NONE',  ( -39.11308345346323279, -25.25305377910670757, 3.767574040739871677 ) ) ;
#90365 = ORIENTED_EDGE ( 'NONE', *, *, #90686, .T. ) ;
#90366 = VERTEX_POINT ( 'NONE', #23255 ) ;
#90367 = VERTEX_POINT ( 'NONE', #16150 ) ;
#90368 = FACE_BOUND ( 'NONE', #17774, .T. ) ;
#90369 = PLANE ( 'NONE',  #92397 ) ;
#90370 = FACE_OUTER_BOUND ( 'NONE', #77457, .T. ) ;
#90371 = CARTESIAN_POINT ( 'NONE',  ( 10.28901978357889035, -18.02705789925236957, -1.500000000000002220 ) ) ;
#90372 = CARTESIAN_POINT ( 'NONE',  ( 11.36066313177254905, -18.55813952095733654, 11.49999999999999645 ) ) ;
#90373 = VERTEX_POINT ( 'NONE', #46116 ) ;
#90374 = DIRECTION ( 'NONE',  ( 0.000000000000000000, -0.9999999999976377785, -2.173523156925979975E-06 ) ) ;
#90375 = CARTESIAN_POINT ( 'NONE',  ( 27.53860345374771867, -5.356774720514425603, -9.482392034746242260 ) ) ;
#90376 = VECTOR ( 'NONE', #6272, 1000.000000000000114 ) ;
#90377 = CARTESIAN_POINT ( 'NONE',  ( -115.5138003424739850, -24.92564183028979130, 1.928384488918252870 ) ) ;
#90378 = CARTESIAN_POINT ( 'NONE',  ( -10.09097066620046235, 20.03973272787133553, -1.500000000000002220 ) ) ;
#90379 = DIRECTION ( 'NONE',  ( -0.9161084732596779245, -5.365801633547208359E-16, 0.4009304992412300872 ) ) ;
#90380 = CARTESIAN_POINT ( 'NONE',  ( -102.5228709571500900, -23.72773821059536559, 11.05748984161097503 ) ) ;
#90382 = ORIENTED_EDGE ( 'NONE', *, *, #61320, .F. ) ;
#90381 = ADVANCED_FACE ( 'NONE', ( #47121 ), #85163, .F. ) ;
#90383 = CARTESIAN_POINT ( 'NONE',  ( -71.70421716572423065, -25.26843853055491351, 6.074178405081902099 ) ) ;
#90384 = DIRECTION ( 'NONE',  ( -1.000000000000000000, 0.000000000000000000, 0.000000000000000000 ) ) ;
#90386 = B_SPLINE_SURFACE_WITH_KNOTS ( 'NONE', 3, 3, ( 
 ( #58482, #81801, #83788, #29497 ),
 ( #43254, #82792, #20885, #66610 ),
 ( #13272, #44248, #52849, #52354 ),
 ( #89914, #51357, #74194, #75176 ),
 ( #59975, #58975, #5670, #36620 ),
 ( #98004, #4687, #35635, #59469 ),
 ( #97520, #67589, #12276, #19890 ) ),
 .UNSPECIFIED., .F., .F., .F.,
 ( 4, 3, 4 ),
 ( 4, 4 ),
 ( 0.0004766839783845967446, 0.1029713700210911909, 0.2054660560637977806 ),
 ( 0.1795396690725346300, 0.1806352329019877689 ),
 .UNSPECIFIED. ) ;
#90385 = B_SPLINE_CURVE_WITH_KNOTS ( 'NONE', 3,
 ( #34707, #11367, #65186, #96595 ),
 .UNSPECIFIED., .F., .F.,
 ( 4, 4 ),
 ( 2.775557561562891351E-17, 0.0001000000000000167286 ),
 .UNSPECIFIED. ) ;
#90387 = VERTEX_POINT ( 'NONE', #30881 ) ;
#90388 = VERTEX_POINT ( 'NONE', #68945 ) ;
#90389 = CARTESIAN_POINT ( 'NONE',  ( -108.5228709571500616, -24.65952944569304961, 1.056160979905704123 ) ) ;
#90390 = EDGE_CURVE ( 'NONE', #21622, #74873, #21499, .T. ) ;
#90391 = ORIENTED_EDGE ( 'NONE', *, *, #78833, .T. ) ;
#90392 = CARTESIAN_POINT ( 'NONE',  ( -15.93125441714207646, -14.09135727244061265, -1.500000000000002220 ) ) ;
#90393 = ORIENTED_EDGE ( 'NONE', *, *, #54883, .F. ) ;
#90394 = DIRECTION ( 'NONE',  ( -0.000000000000000000, -1.000000000000000000, -0.000000000000000000 ) ) ;
#90395 = PRODUCT_DEFINITION_SHAPE ( 'NONE', 'NONE',  #100423 ) ;
#90396 = CARTESIAN_POINT ( 'NONE',  ( 21.05697796394607835, 5.830696701215154043, 11.49999999999998934 ) ) ;
#90397 = CARTESIAN_POINT ( 'NONE',  ( 1.542438661763949392, 0.000000000000000000, 0.000000000000000000 ) ) ;
#90398 = CARTESIAN_POINT ( 'NONE',  ( 13.52301212282245935, 18.22803923376396540, 11.49999999999998934 ) ) ;
#90399 = CARTESIAN_POINT ( 'NONE',  ( -40.93315603532715130, -25.28892444152159769, 3.395436525629587088 ) ) ;
#90400 = CARTESIAN_POINT ( 'NONE',  ( 10.46399479596398052, -3.316774720514422903, -27.03001098546561209 ) ) ;
#90401 = CARTESIAN_POINT ( 'NONE',  ( 12.42595048307055983, -18.10569578304522764, -1.500000000000002220 ) ) ;
#90402 = CARTESIAN_POINT ( 'NONE',  ( -39.52287095715006870, -24.65952944569304606, 1.056160979905691910 ) ) ;
#90403 = ORIENTED_EDGE ( 'NONE', *, *, #43275, .T. ) ;
#90404 = CARTESIAN_POINT ( 'NONE',  ( 29.72131469344797239, -6.278265095287072661, 26.95488797742164877 ) ) ;
#90405 = VERTEX_POINT ( 'NONE', #53232 ) ;
#90406 = CARTESIAN_POINT ( 'NONE',  ( -116.6228709571499991, -23.94994826722566117, -0.6494450866342701412 ) ) ;
#90407 = CARTESIAN_POINT ( 'NONE',  ( -130.5728709571500588, -24.47917135695840685, 9.440663514584114679 ) ) ;
#90408 = CARTESIAN_POINT ( 'NONE',  ( -10.27976737060564361, -22.47453952272712385, -0.4716817114508953246 ) ) ;
#90409 = CARTESIAN_POINT ( 'NONE',  ( -8.014198274750887308, -19.69740135394370384, 11.49999999999998934 ) ) ;
#90410 = DIRECTION ( 'NONE',  ( 0.000000000000000000, 0.000000000000000000, -1.000000000000000000 ) ) ;
#90411 = CARTESIAN_POINT ( 'NONE',  ( -40.01839366089613748, -25.29500187561385260, 5.509688069775453556 ) ) ;
#90412 = ADVANCED_FACE ( 'NONE', ( #7044 ), #60722, .T. ) ;
#90413 = DIRECTION ( 'NONE',  ( 0.000000000000000000, 0.9999999999976377785, 2.173523156925979975E-06 ) ) ;
#90414 = AXIS2_PLACEMENT_3D ( 'NONE', #79381, #27103, #40824 ) ;
#90415 = DIRECTION ( 'NONE',  ( 0.000000000000000000, -2.173523156925979552E-06, 0.9999999999976378895 ) ) ;
#90416 = CARTESIAN_POINT ( 'NONE',  ( -117.5209649390443758, -23.73791477778912551, 11.05961554403169878 ) ) ;
#90417 = ORIENTED_EDGE ( 'NONE', *, *, #87120, .F. ) ;
#90418 = CARTESIAN_POINT ( 'NONE',  ( -6.824658503225996320, 18.35159230250476270, 11.49999999999999645 ) ) ;
#90419 = CARTESIAN_POINT ( 'NONE',  ( -114.6228709571500559, -29.50248528299804818, 1.056150453629043584 ) ) ;
#90420 = VECTOR ( 'NONE', #72586, 1000.000000000000227 ) ;
#90421 = CARTESIAN_POINT ( 'NONE',  ( -115.6228709571500559, -29.50247984919015209, -1.443849546365046699 ) ) ;
#90422 = ORIENTED_EDGE ( 'NONE', *, *, #78158, .T. ) ;
#90423 = CARTESIAN_POINT ( 'NONE',  ( -88.60252819948608760, -23.48786465467241413, 11.44779295918254469 ) ) ;
#90424 = EDGE_CURVE ( 'NONE', #44949, #66931, #62690, .T. ) ;
#90425 = CARTESIAN_POINT ( 'NONE',  ( -100.5423878678571725, -25.03330743373828327, 7.561026521112214738 ) ) ;
#90426 = CARTESIAN_POINT ( 'NONE',  ( -9.278253834636473130, -6.376774720514426953, 21.78128695274316229 ) ) ;
#90427 = CARTESIAN_POINT ( 'NONE',  ( -50.33541908643975660, -25.12321947555366819, 7.100310136161304797 ) ) ;
#90428 = CARTESIAN_POINT ( 'NONE',  ( -5.312243195520525596, -18.98051080891723430, 11.49999999999998934 ) ) ;
#90429 = ORIENTED_EDGE ( 'NONE', *, *, #73998, .F. ) ;
#90430 = B_SPLINE_CURVE_WITH_KNOTS ( 'NONE', 3,
 ( #10230, #2630, #3136, #18836, #49817, #57430 ),
 .UNSPECIFIED., .F., .F.,
 ( 4, 2, 4 ),
 ( 6.384118678615735980E-06, 0.001386860460828379755, 0.002767336802978144061 ),
 .UNSPECIFIED. ) ;
#90431 = CARTESIAN_POINT ( 'NONE',  ( 33.00535138976592719, -3.570691370340881576, -12.97242311383975988 ) ) ;
#90432 = LINE ( 'NONE', #59001, #4237 ) ;
#90433 = B_SPLINE_CURVE_WITH_KNOTS ( 'NONE', 3,
 ( #19480, #2282, #41846, #9873, #42842, #18982, #56066, #50443, #35221, #95615, #17487, #34716, #95113, #49961, #73772, #33212, #58073, #72288, #18487 ),
 .UNSPECIFIED., .F., .F.,
 ( 4, 1, 1, 1, 1, 1, 1, 1, 1, 1, 1, 1, 1, 1, 1, 1, 4 ),
 ( 0.000000000000000000, 0.07059928943359200515, 0.1379009210036200861, 0.2031961978097334975, 0.2667897246502631270, 0.3291063872214231578, 0.3906535452348600668, 0.4526530569344815458, 0.5157480403003722458, 0.5779263408004527980, 0.6389300116184465361, 0.6983507176418213280, 0.7572960374442707643, 0.8163937673501530101, 0.8762669096141296743, 0.9368171089060820522, 1.000000000000000000 ),
 .UNSPECIFIED. ) ;
#90434 = CALENDAR_DATE ( 2026, 9, 10 ) ;
#90435 = EDGE_LOOP ( 'NONE', ( #32914, #22501, #70932, #51076 ) ) ;
#90436 = CARTESIAN_POINT ( 'NONE',  ( 9.071512145086501278, -0.9000000000000000222, 3.687490859131163479 ) ) ;
#90437 = CARTESIAN_POINT ( 'NONE',  ( -84.58953762381671027, -23.48783264082479150, -1.443836473390065489 ) ) ;
#90438 = DIRECTION ( 'NONE',  ( 0.000000000000000000, -1.000000000000000000, 0.000000000000000000 ) ) ;
#90439 = CARTESIAN_POINT ( 'NONE',  ( -62.92287095715004597, -23.47593901973090169, -1.443836447538997536 ) ) ;
#90440 = CARTESIAN_POINT ( 'NONE',  ( -7.326845193947049140, -6.376774720514417183, 20.33046051580616265 ) ) ;
#90441 = CARTESIAN_POINT ( 'NONE',  ( -99.62287095715004170, -23.73934037231757799, 11.05740245334328087 ) ) ;
#90442 = CARTESIAN_POINT ( 'NONE',  ( -3.737436867076076030, 13.63388347648318444, 2.100000000000000089 ) ) ;
#90444 = EDGE_CURVE ( 'NONE', #12272, #57426, #10043, .T. ) ;
#90443 = CARTESIAN_POINT ( 'NONE',  ( 17.47191945374660094, 9.613082372698542599, -1.500000000000002220 ) ) ;
#90445 = CARTESIAN_POINT ( 'NONE',  ( -28.98875734969026396, -5.965225279485572685, 7.870022800118625206 ) ) ;
#90446 = LINE ( 'NONE', #51897, #1481 ) ;
#90447 = VERTEX_POINT ( 'NONE', #94275 ) ;
#90448 = CARTESIAN_POINT ( 'NONE',  ( -101.7776484685884242, -25.26303730729093644, 3.986250639247583827 ) ) ;
#90449 = CARTESIAN_POINT ( 'NONE',  ( -1.358974358974357921, -5.876774720514419847, 20.75510817307693046 ) ) ;
#90450 = DIRECTION ( 'NONE',  ( 0.6755245625654127117, 0.4376337494475115442, 0.5934166046845339437 ) ) ;
#90451 = LINE ( 'NONE', #6208, #39463 ) ;
#90452 = LINE ( 'NONE', #66152, #12116 ) ;
#90453 = CARTESIAN_POINT ( 'NONE',  ( -39.66516719614519815, -23.48783264082476308, -1.443836473390098352 ) ) ;
#90454 = ADVANCED_FACE ( 'NONE', ( #49128 ), #71961, .T. ) ;
#90455 = CARTESIAN_POINT ( 'NONE',  ( -119.6228709571500559, -23.94994826722566117, -0.6494450866342695861 ) ) ;
#90456 = CARTESIAN_POINT ( 'NONE',  ( -51.66173670239771099, -25.31574316003434078, 4.265171533202613219 ) ) ;
#90457 = EDGE_LOOP ( 'NONE', ( #97475, #28240, #18109, #74166 ) ) ;
#90458 = B_SPLINE_SURFACE_WITH_KNOTS ( 'NONE', 3, 1, ( 
 ( #5393, #12503 ),
 ( #67812, #27736 ),
 ( #66318, #43468 ),
 ( #97739, #51576 ),
 ( #82509, #36347 ),
 ( #67303, #98226 ),
 ( #61691, #61198 ),
 ( #68794, #46450 ),
 ( #69791, #76384 ),
 ( #53583, #75891 ),
 ( #91123, #21596 ),
 ( #269, #7880 ),
 ( #52571, #30723 ),
 ( #44966, #76873 ),
 ( #83504, #60693 ),
 ( #13989, #31216 ),
 ( #45468, #100204 ),
 ( #6393, #68293 ),
 ( #92610, #92117 ),
 ( #84508, #69288 ),
 ( #23090, #8382 ),
 ( #29726, #91615 ),
 ( #62187, #39328 ),
 ( #22587, #70291 ),
 ( #37352, #99223 ),
 ( #93112, #6885 ),
 ( #22095, #54562 ) ),
 .UNSPECIFIED., .F., .F., .F.,
 ( 4, 1, 1, 1, 1, 1, 1, 1, 1, 1, 1, 1, 1, 1, 1, 1, 1, 1, 1, 1, 1, 1, 1, 1, 4 ),
 ( 2, 2 ),
 ( 0.000000000000000000, 0.03378714634699071101, 0.06662165772429405608, 0.09928487809597190406, 0.1313611650426508015, 0.1635851875953426293, 0.1961039269870683555, 0.2289022543238164731, 0.2621580559050077919, 0.2959912222583166441, 0.3302178457248000631, 0.3650598258919540706, 0.4009507373401078323, 0.4376203820767375907, 0.4757075294370922136, 0.5153806916250485148, 0.5564135414931642432, 0.5997648298727311644, 0.6464241555840872788, 0.6964314445175667778, 0.7497815178015574400, 0.8065733069755323115, 0.8674355315653993204, 0.9318867532508741114, 1.000000000000000000 ),
 ( 0.000000000000000000, 1.000000000000000000 ),
 .UNSPECIFIED. ) ;
#90459 = CARTESIAN_POINT ( 'NONE',  ( -29.49875734969026198, 5.965225279485572685, 10.11402280011862587 ) ) ;
#90460 = CARTESIAN_POINT ( 'NONE',  ( -127.5903464641895937, -23.73766607897670511, -1.055555164236447130 ) ) ;
#90461 = ORIENTED_EDGE ( 'NONE', *, *, #67491, .F. ) ;
#90462 = CARTESIAN_POINT ( 'NONE',  ( 19.74221769882431587, -4.499994434135383692, -1.500000000000002220 ) ) ;
#90463 = CARTESIAN_POINT ( 'NONE',  ( -70.27422298781921484, -25.31465149953924865, 4.851635142449610250 ) ) ;
#90464 = ADVANCED_FACE ( 'NONE', ( #2949 ), #2441, .F. ) ;
#90465 = CARTESIAN_POINT ( 'NONE',  ( -24.90875734969025501, -3.316774720514426456, 27.45402280011862572 ) ) ;
#90466 = AXIS2_PLACEMENT_3D ( 'NONE', #23668, #55649, #30285 ) ;
#90467 = EDGE_CURVE ( 'NONE', #92450, #26965, #65364, .T. ) ;
#90468 = CARTESIAN_POINT ( 'NONE',  ( -109.6228709571501128, -24.33832256526969218, 0.1851278514119941987 ) ) ;
#90469 = B_SPLINE_CURVE_WITH_KNOTS ( 'NONE', 3,
 ( #42305, #4217, #87956, #33666, #3727, #42790 ),
 .UNSPECIFIED., .F., .F.,
 ( 4, 2, 4 ),
 ( 6.384118678610730015E-06, 0.001386860460828374768, 0.002767336802978138856 ),
 .UNSPECIFIED. ) ;
#90470 = ORIENTED_EDGE ( 'NONE', *, *, #51036, .F. ) ;
#90471 = PLANE ( 'NONE',  #17678 ) ;
#90472 = CARTESIAN_POINT ( 'NONE',  ( -105.5562042904833930, -25.00158670708909980, 2.256160236439166411 ) ) ;
#90473 = CARTESIAN_POINT ( 'NONE',  ( 3.315226082619958881, 19.80964767386612380, -1.500000000000002220 ) ) ;
#90474 = CARTESIAN_POINT ( 'NONE',  ( 11.23609023086081038, -17.74952302366565604, 11.49999999999999645 ) ) ;
#90475 = DIRECTION ( 'NONE',  ( 0.000000000000000000, 0.000000000000000000, -1.000000000000000000 ) ) ;
#90476 = CARTESIAN_POINT ( 'NONE',  ( -70.49783793440687418, -24.52399227489127043, 9.353111116836524630 ) ) ;
#90477 = CARTESIAN_POINT ( 'NONE',  ( -12.21066354923914865, 18.40238043084326591, 11.49999999999998934 ) ) ;
#90478 = CARTESIAN_POINT ( 'NONE',  ( 17.35315496411208613, -10.91789592880838811, 11.49999999999998934 ) ) ;
#90479 = CARTESIAN_POINT ( 'NONE',  ( -46.92287095715006018, -23.47596703998600276, 11.44779298504227683 ) ) ;
#90480 = CARTESIAN_POINT ( 'NONE',  ( -70.62287095715004170, -23.48783264082478084, -1.443836473390067265 ) ) ;
#90481 = DIRECTION ( 'NONE',  ( 1.000000000000000000, 3.773278334444166432E-23, 8.201307841325785021E-29 ) ) ;
#90482 = ORIENTED_EDGE ( 'NONE', *, *, #5463, .F. ) ;
#90483 = CARTESIAN_POINT ( 'NONE',  ( -41.46611000704998418, -29.50249209050311094, 4.188164501617994695 ) ) ;
#90484 = B_SPLINE_CURVE_WITH_KNOTS ( 'NONE', 3,
 ( #83155, #53227, #13639, #75535 ),
 .UNSPECIFIED., .F., .F.,
 ( 4, 4 ),
 ( 1.387778780781445521E-17, 0.0004038461538461296518 ),
 .UNSPECIFIED. ) ;
#90485 = CYLINDRICAL_SURFACE ( 'NONE', #40516, 0.3000000000000016542 ) ;
#90486 = ORIENTED_EDGE ( 'NONE', *, *, #82767, .T. ) ;
#90487 = EDGE_LOOP ( 'NONE', ( #3936, #29245, #43138, #75181 ) ) ;
#90488 = CARTESIAN_POINT ( 'NONE',  ( -83.58953762381673869, -24.65952944569304606, 1.056160979905698794 ) ) ;
#90489 = DIRECTION ( 'NONE',  ( -3.773278334453079618E-23, 0.9999999999976377785, 2.173523156925979975E-06 ) ) ;
#90490 = CARTESIAN_POINT ( 'NONE',  ( -44.52287095715006160, -23.48786465467241058, 11.44779295918255180 ) ) ;
#90491 = CARTESIAN_POINT ( 'NONE',  ( -17.20787902393383462, -11.26661214947554157, -1.500000000000002220 ) ) ;
#90492 = CARTESIAN_POINT ( 'NONE',  ( 19.31049906410359895, -9.575588319827552652, 11.49999999999999645 ) ) ;
#90493 = ORIENTED_EDGE ( 'NONE', *, *, #3463, .T. ) ;
#90494 = CARTESIAN_POINT ( 'NONE',  ( -99.64934318012689118, -25.30535455722350591, 4.927356316503054501 ) ) ;
#90495 = CARTESIAN_POINT ( 'NONE',  ( 30.61643171304413613, 6.376774720514426953, 27.37433008668288181 ) ) ;
#90496 = CARTESIAN_POINT ( 'NONE',  ( 21.86734719908870872, 4.625976558377421277, 11.49999999999998934 ) ) ;
#90497 = CARTESIAN_POINT ( 'NONE',  ( -124.6228709571500417, -24.65952944569304606, 1.056160979905705011 ) ) ;
#90498 = LINE ( 'NONE', #45824, #59422 ) ;
#90499 = ORIENTED_EDGE ( 'NONE', *, *, #51458, .F. ) ;
#90500 = CARTESIAN_POINT ( 'NONE',  ( -94.52287095715006160, -24.65952944569304961, 1.056160979905700570 ) ) ;
#90501 = CARTESIAN_POINT ( 'NONE',  ( 3.045412351277957175, -5.876774720514421624, 20.90433128744512814 ) ) ;
#90502 = CARTESIAN_POINT ( 'NONE',  ( -13.97254113366623152, 15.51630364309664856, -1.500000000000002220 ) ) ;
#90503 = ORIENTED_EDGE ( 'NONE', *, *, #46029, .F. ) ;
#90505 = EDGE_LOOP ( 'NONE', ( #10128, #62640, #27721, #95579 ) ) ;
#90504 = CARTESIAN_POINT ( 'NONE',  ( -67.58020753937425695, -24.66019654487199730, 8.947790411086115725 ) ) ;
#90506 = ORIENTED_EDGE ( 'NONE', *, *, #65954, .F. ) ;
#90507 = ADVANCED_FACE ( 'NONE', ( #9042 ), #59892, .T. ) ;
#90508 = CARTESIAN_POINT ( 'NONE',  ( -100.6305594176849070, -24.40133493613050319, 9.663955038902802386 ) ) ;
#90509 = CARTESIAN_POINT ( 'NONE',  ( 16.66693084842116335, 13.01107939256401913, -1.500000000000002220 ) ) ;
#90510 = ORIENTED_EDGE ( 'NONE', *, *, #55909, .T. ) ;
#90511 = CARTESIAN_POINT ( 'NONE',  ( -60.62287095715004881, -24.99156045073392463, 7.747789690856161648 ) ) ;
#90512 = DIRECTION ( 'NONE',  ( 0.000000000000000000, 0.000000000000000000, 1.000000000000000000 ) ) ;
#90513 = DIRECTION ( 'NONE',  ( -1.000000000000000000, 0.000000000000000000, 0.000000000000000000 ) ) ;
#90514 = CARTESIAN_POINT ( 'NONE',  ( -76.55419120562295632, -23.96169478059713143, 10.65365249895718058 ) ) ;
#90515 = CARTESIAN_POINT ( 'NONE',  ( -40.52287095715005449, -24.99156044556202261, 7.747789690856173195 ) ) ;
#90516 = CARTESIAN_POINT ( 'NONE',  ( -21.04499429308205549, 5.405531755741471045, -1.500000000000002220 ) ) ;
#90517 = CARTESIAN_POINT ( 'NONE',  ( -71.70379718938951896, -25.31639723079672066, 6.052014632951667750 ) ) ;
#90519 = ORIENTED_EDGE ( 'NONE', *, *, #25063, .T. ) ;
#90518 = CARTESIAN_POINT ( 'NONE',  ( 18.98964132805693694, -11.70494588174365092, 11.49999999999999645 ) ) ;
#90520 = DIRECTION ( 'NONE',  ( 0.6599726524652353987, 0.000000000000000000, -0.7512896232465889890 ) ) ;
#90521 = CARTESIAN_POINT ( 'NONE',  ( 15.03452642382691629, 3.688048319827653021, -27.40128341529668887 ) ) ;
#90522 = PLANE ( 'NONE',  #248 ) ;
#90523 = ORIENTED_EDGE ( 'NONE', *, *, #13692, .F. ) ;
#90524 = ORIENTED_EDGE ( 'NONE', *, *, #9322, .T. ) ;
#90525 = VERTEX_POINT ( 'NONE', #73947 ) ;
#90526 = CARTESIAN_POINT ( 'NONE',  ( -56.62287095715008434, -23.47596703998600276, 11.44779298504227683 ) ) ;
#90527 = PLANE ( 'NONE',  #72478 ) ;
#90528 = CARTESIAN_POINT ( 'NONE',  ( 30.63256949310621735, -4.401217678701063285, 28.01131607762999565 ) ) ;
#90529 = DIRECTION ( 'NONE',  ( 0.9116753070387548785, -8.931253266735290907E-07, 0.4109113463205835703 ) ) ;
#90530 = EDGE_CURVE ( 'NONE', #28802, #74870, #81056, .T. ) ;
#90531 = CARTESIAN_POINT ( 'NONE',  ( -19.35591191756920892, -0.7100623379298715010, 11.49999999999998934 ) ) ;
#90532 = CARTESIAN_POINT ( 'NONE',  ( -31.52287095715006160, -24.66019654487198665, 8.947790411086131712 ) ) ;
#90533 = ORIENTED_EDGE ( 'NONE', *, *, #83908, .F. ) ;
#90534 = EDGE_CURVE ( 'NONE', #53606, #8243, #72961, .T. ) ;
#90535 = CARTESIAN_POINT ( 'NONE',  ( -13.40542139710017899, 13.98966777563825481, 11.49999999999999645 ) ) ;
#90536 = DIRECTION ( 'NONE',  ( -0.000000000000000000, -1.000000000000000000, -0.000000000000000000 ) ) ;
#90537 = ORIENTED_EDGE ( 'NONE', *, *, #93870, .F. ) ;
#90538 = CARTESIAN_POINT ( 'NONE',  ( -16.22218391600152643, -6.376774720514426953, -54.85883559227303863 ) ) ;
#90539 = CARTESIAN_POINT ( 'NONE',  ( 10.22845072388260768, 5.356774720514425603, -24.98266432381545954 ) ) ;
#90540 = EDGE_CURVE ( 'NONE', #99263, #13594, #3945, .T. ) ;
#90541 = CARTESIAN_POINT ( 'NONE',  ( -4.621320343559261801, 12.74999999999999645, 2.100000000000000089 ) ) ;
#90542 = AXIS2_PLACEMENT_3D ( 'NONE', #98731, #36346, #90625 ) ;
#90543 = EDGE_CURVE ( 'NONE', #78575, #11988, #33559, .T. ) ;
#90544 = CARTESIAN_POINT ( 'NONE',  ( -36.52287095715009002, -24.66019654487199730, 8.947790411086124607 ) ) ;
#90545 = CARTESIAN_POINT ( 'NONE',  ( 0.6594449095415070294, 19.62168050102039629, -1.500000000000002220 ) ) ;
#90546 = DIRECTION ( 'NONE',  ( 0.000000000000000000, 0.000000000000000000, 1.000000000000000000 ) ) ;
#90548 = ADVANCED_FACE ( 'NONE', ( #67337 ), #43004, .T. ) ;
#90547 = ORIENTED_EDGE ( 'NONE', *, *, #27228, .F. ) ;
#90549 = CARTESIAN_POINT ( 'NONE',  ( 21.55061338234859392, -0.003183148592148328428, 11.49999999999998934 ) ) ;
#90550 = AXIS2_PLACEMENT_3D ( 'NONE', #28805, #52149, #83076 ) ;
#90551 = CARTESIAN_POINT ( 'NONE',  ( 7.160000000000000142, -6.754662360505033547, 7.925641719537454222 ) ) ;
#90552 = DIRECTION ( 'NONE',  ( -1.000000000000000000, 0.000000000000000000, -7.994117400814786717E-16 ) ) ;
#90553 = DIRECTION ( 'NONE',  ( 0.000000000000000000, 0.000000000000000000, -1.000000000000000000 ) ) ;
#90554 = CARTESIAN_POINT ( 'NONE',  ( -100.0747864355570158, -25.18439346793923050, 3.344773611727388740 ) ) ;
#90555 = CARTESIAN_POINT ( 'NONE',  ( 22.51966570110743149, 4.691836548664650053, -1.500000000000002220 ) ) ;
#90556 = MECHANICAL_CONTEXT ( 'NONE', #16760, 'mechanical' ) ;
#90557 = FACE_OUTER_BOUND ( 'NONE', #91372, .T. ) ;
#90558 = CARTESIAN_POINT ( 'NONE',  ( -44.62287095715004881, -24.66019654487198665, 8.947790411086135265 ) ) ;
#90559 = CARTESIAN_POINT ( 'NONE',  ( -19.98115086844608612, 2.773124471107000666, 11.49999999999999645 ) ) ;
#90560 = CARTESIAN_POINT ( 'NONE',  ( -71.22287095715005023, -23.47593901973090169, -1.443836447538997536 ) ) ;
#90561 = CARTESIAN_POINT ( 'NONE',  ( -32.55272256901955075, -23.96169478059712787, 10.65365249895719124 ) ) ;
#90562 = VECTOR ( 'NONE', #15447, 1000.000000000000114 ) ;
#90563 = CARTESIAN_POINT ( 'NONE',  ( 13.74975846015576586, -6.475225279485573360, -27.72022515045486557 ) ) ;
#90564 = DIRECTION ( 'NONE',  ( -0.000000000000000000, 1.000000000000000000, -0.000000000000000000 ) ) ;
#90565 = CARTESIAN_POINT ( 'NONE',  ( -111.2787752023839971, -25.18425713224470996, 3.894639490442704410 ) ) ;
#90567 = EDGE_CURVE ( 'NONE', #74525, #74870, #89172, .T. ) ;
#90566 = CARTESIAN_POINT ( 'NONE',  ( -19.84341114293531305, -1.032944114202840824, 11.49999999999998934 ) ) ;
#90568 = CARTESIAN_POINT ( 'NONE',  ( -99.62287095715005592, -29.50250786944525672, 11.44777988621623166 ) ) ;
#90569 = CARTESIAN_POINT ( 'NONE',  ( -19.30086548479123465, -4.275078920326023990, -1.500000000000002220 ) ) ;
#90570 = CARTESIAN_POINT ( 'NONE',  ( 33.13288845015618023, 5.965225279485572685, -0.1650522222209214185 ) ) ;
#90571 = B_SPLINE_CURVE_WITH_KNOTS ( 'NONE', 3,
 ( #53798, #91343, #36555, #21818 ),
 .UNSPECIFIED., .F., .F.,
 ( 4, 4 ),
 ( 0.000000000000000000, 9.999999999999592548E-05 ),
 .UNSPECIFIED. ) ;
#90572 = CARTESIAN_POINT ( 'NONE',  ( -1.022535880784302353, -6.376774720514415407, 19.99258394656883908 ) ) ;
#90573 = LINE ( 'NONE', #60149, #32944 ) ;
#90574 = CARTESIAN_POINT ( 'NONE',  ( 18.79598114143782084, -8.675585332008726169, 11.49999999999999645 ) ) ;
#90575 = PLANE ( 'NONE',  #53217 ) ;
#90576 = ADVANCED_FACE ( 'NONE', ( #20640 ), #35394, .T. ) ;
#90577 = CARTESIAN_POINT ( 'NONE',  ( -97.58953762381672448, -24.64965694238407323, 8.947790433994651238 ) ) ;
#90578 = CARTESIAN_POINT ( 'NONE',  ( -49.52475239181693212, -25.31439355338475394, 5.557100884789670125 ) ) ;
#90579 = AXIS2_PLACEMENT_3D ( 'NONE', #91175, #14041, #37895 ) ;
#90580 = CARTESIAN_POINT ( 'NONE',  ( -14.94938274637043207, -17.11189489004485864, 11.49999999999999645 ) ) ;
#90581 = ORIENTED_EDGE ( 'NONE', *, *, #38839, .F. ) ;
#90582 = CARTESIAN_POINT ( 'NONE',  ( -0.4909855769230799249, -5.876774720514410077, 19.14743589743590491 ) ) ;
#90583 = EDGE_CURVE ( 'NONE', #29990, #14292, #93798, .T. ) ;
#90584 = CARTESIAN_POINT ( 'NONE',  ( 30.59430046144282400, 4.508643932895013862, 26.46466010020539272 ) ) ;
#90585 = FACE_OUTER_BOUND ( 'NONE', #83861, .T. ) ;
#90586 = EDGE_CURVE ( 'NONE', #18471, #46432, #98258, .T. ) ;
#90587 = CARTESIAN_POINT ( 'NONE',  ( 22.81105451610979173, 4.772774720514425972, -18.46691820600746681 ) ) ;
#90588 = EDGE_LOOP ( 'NONE', ( #66820, #9494, #31130, #18327 ) ) ;
#90589 = EDGE_CURVE ( 'NONE', #76855, #45940, #13024, .T. ) ;
#90590 = ORIENTED_EDGE ( 'NONE', *, *, #25418, .F. ) ;
#90591 = FACE_OUTER_BOUND ( 'NONE', #85610, .T. ) ;
#90592 = CARTESIAN_POINT ( 'NONE',  ( -14.01358469492184966, -18.07645309290061064, -1.500000000000002220 ) ) ;
#90594 = ADVANCED_FACE ( 'NONE', ( #57735 ), #43502, .T. ) ;
#90593 = CARTESIAN_POINT ( 'NONE',  ( -29.64367331884317025, -24.07992180899756107, -0.2315648265717072385 ) ) ;
#90595 = CARTESIAN_POINT ( 'NONE',  ( 20.55510029441247610, -6.647428040031946317, -1.500000000000002220 ) ) ;
#90596 = LINE ( 'NONE', #21075, #4231 ) ;
#90597 = LINE ( 'NONE', #44436, #61431 ) ;
#90598 = CARTESIAN_POINT ( 'NONE',  ( -13.16310354753345990, -18.33534949228788236, 11.49999999999999645 ) ) ;
#90599 = ORIENTED_EDGE ( 'NONE', *, *, #73822, .F. ) ;
#90600 = CARTESIAN_POINT ( 'NONE',  ( -70.00627666057835086, -25.31612425288418322, 4.873906333287980175 ) ) ;
#90601 = CARTESIAN_POINT ( 'NONE',  ( 14.26656746985186608, 16.74056184347216458, 11.49999999999998934 ) ) ;
#90602 = CARTESIAN_POINT ( 'NONE',  ( -105.5120787285895148, -24.52399227489126687, 9.353111116836517525 ) ) ;
#90603 = CARTESIAN_POINT ( 'NONE',  ( -40.99321688279000853, -25.10925790275778624, 2.933756721058497163 ) ) ;
#90604 = ORIENTED_EDGE ( 'NONE', *, *, #27244, .T. ) ;
#90605 = EDGE_CURVE ( 'NONE', #94223, #27910, #35879, .T. ) ;
#90606 = DIRECTION ( 'NONE',  ( 0.000000000000000000, -1.000000000000000000, 0.000000000000000000 ) ) ;
#90607 = CARTESIAN_POINT ( 'NONE',  ( -90.62931513133528938, -24.63419186844611275, 9.035850630976923981 ) ) ;
#90608 = ORIENTED_EDGE ( 'NONE', *, *, #98918, .F. ) ;
#90609 = CARTESIAN_POINT ( 'NONE',  ( -111.6228709571500559, -29.50247984919015209, -1.443849546365048253 ) ) ;
#90610 = VECTOR ( 'NONE', #28706, 1000.000000000000000 ) ;
#90611 = ORIENTED_EDGE ( 'NONE', *, *, #45542, .F. ) ;
#90612 = AXIS2_PLACEMENT_3D ( 'NONE', #14327, #13330, #75237 ) ;
#90613 = ORIENTED_EDGE ( 'NONE', *, *, #76134, .F. ) ;
#90614 = CYLINDRICAL_SURFACE ( 'NONE', #33972, 1.149999999999999911 ) ;
#90615 = CARTESIAN_POINT ( 'NONE',  ( -104.5228709571501184, -24.51283580621365132, 0.6167428607019820319 ) ) ;
#90616 = CARTESIAN_POINT ( 'NONE',  ( -57.58748390918375293, -24.34968618360933590, 0.1864209137778796155 ) ) ;
#90617 = CARTESIAN_POINT ( 'NONE',  ( 4.102729645046709450, 19.96921287702725323, -1.500000000000002220 ) ) ;
#90618 = ORIENTED_EDGE ( 'NONE', *, *, #37346, .T. ) ;
#90619 = CARTESIAN_POINT ( 'NONE',  ( -93.52287095715006160, -24.64965694238407323, 8.947790433994196491 ) ) ;
#90620 = VECTOR ( 'NONE', #28978, 1000.000000000000114 ) ;
#90621 = CARTESIAN_POINT ( 'NONE',  ( -30.61333094834724733, -24.36247485673954927, 0.01136689895587368430 ) ) ;
#90622 = LINE ( 'NONE', #75887, #96684 ) ;
#90623 = CARTESIAN_POINT ( 'NONE',  ( 8.160000000000000142, -10.15233964170348457, 0.003711184059992174607 ) ) ;
#90624 = EDGE_LOOP ( 'NONE', ( #77911, #68810, #32586, #109, #46817, #94595, #2938, #79728 ) ) ;
#90625 = DIRECTION ( 'NONE',  ( -1.000000000000000000, 0.000000000000000000, -0.000000000000000000 ) ) ;
#90626 = CIRCLE ( 'NONE', #35581, 252.4458649670781085 ) ;
#90627 = CARTESIAN_POINT ( 'NONE',  ( -60.95156673781919210, -25.21083105912962452, 3.409327675794633361 ) ) ;
#90628 = VECTOR ( 'NONE', #98945, 1000.000000000000114 ) ;
#90629 = CARTESIAN_POINT ( 'NONE',  ( -11.07951500695464553, -17.62175104703424466, -1.500000000000002220 ) ) ;
#90630 = VERTEX_POINT ( 'NONE', #40316 ) ;
#90632 = ORIENTED_EDGE ( 'NONE', *, *, #87701, .T. ) ;
#90631 = CARTESIAN_POINT ( 'NONE',  ( 30.09341516180546350, -4.772774720514425972, -11.39311774897855933 ) ) ;
#90633 = CARTESIAN_POINT ( 'NONE',  ( 0.000000000000000000, -5.356774720514425603, 0.000000000000000000 ) ) ;
#90634 = CARTESIAN_POINT ( 'NONE',  ( -56.52287095715006870, -23.47596703998600631, 11.44779298504228926 ) ) ;
#90635 = ORIENTED_EDGE ( 'NONE', *, *, #84601, .F. ) ;
#90636 = ORIENTED_EDGE ( 'NONE', *, *, #29430, .F. ) ;
#90637 = DIRECTION ( 'NONE',  ( 1.251281512149627050E-16, 0.000000000000000000, -1.000000000000000000 ) ) ;
#90638 = CARTESIAN_POINT ( 'NONE',  ( 11.05000000000000426, -14.50000000000000178, 12.73734666247252711 ) ) ;
#90639 = CARTESIAN_POINT ( 'NONE',  ( -49.52287095715006160, -29.50248528299804818, 1.056150453629033370 ) ) ;
#90640 = CARTESIAN_POINT ( 'NONE',  ( -70.46019744876114999, -25.31201591126554717, 5.316127909876582791 ) ) ;
#90642 = ORIENTED_EDGE ( 'NONE', *, *, #42343, .F. ) ;
#90641 = CARTESIAN_POINT ( 'NONE',  ( -21.04927197579530329, -6.814310187297170529, 11.49999999999999645 ) ) ;
#90643 = DIRECTION ( 'NONE',  ( -3.773278334453079618E-23, 0.9999999999976377785, 2.173523156925979975E-06 ) ) ;
#90644 = CARTESIAN_POINT ( 'NONE',  ( 21.16457415087624128, -7.944649954575952577, -1.500000000000002220 ) ) ;
#90646 = ORIENTED_EDGE ( 'NONE', *, *, #17339, .T. ) ;
#90645 = CARTESIAN_POINT ( 'NONE',  ( -46.52287095715005449, -23.96177878511308634, 10.65340807706331283 ) ) ;
#90647 = ORIENTED_EDGE ( 'NONE', *, *, #86230, .F. ) ;
#90648 = CARTESIAN_POINT ( 'NONE',  ( 26.73860345374794534, 1.477225279485574028, -7.113848178280766099 ) ) ;
#90649 = VECTOR ( 'NONE', #30534, 1000.000000000000000 ) ;
#90650 = ADVANCED_FACE ( 'NONE', ( #87994 ), #95599, .T. ) ;
#90651 = CARTESIAN_POINT ( 'NONE',  ( -16.19606052442943067, -11.93128464602566474, 11.49999999999998934 ) ) ;
#90652 = PRODUCT ( 'MAS-154', 'MAS-154', '', ( #97786 ) ) ;
#90653 = CARTESIAN_POINT ( 'NONE',  ( 28.30015606816038698, -1.682774720514426114, -13.13501953239208930 ) ) ;
#90654 = ORIENTED_EDGE ( 'NONE', *, *, #96315, .F. ) ;
#90655 = EDGE_CURVE ( 'NONE', #50270, #20514, #63970, .T. ) ;
#90656 = CARTESIAN_POINT ( 'NONE',  ( -107.6228709571500701, -24.64898659630368272, 1.056161002820831474 ) ) ;
#90657 = CARTESIAN_POINT ( 'NONE',  ( -22.23078454666273274, -1.437644496696519170, -1.500000000000002220 ) ) ;
#90658 = DIRECTION ( 'NONE',  ( 0.000000000000000000, 0.000000000000000000, 1.000000000000000000 ) ) ;
#90659 = EDGE_CURVE ( 'NONE', #78412, #30481, #90761, .T. ) ;
#90660 = ORIENTED_EDGE ( 'NONE', *, *, #99421, .F. ) ;
#90661 = CARTESIAN_POINT ( 'NONE',  ( -110.5562042904833930, -23.48786465467242479, 11.44779295918253936 ) ) ;
#90662 = FACE_OUTER_BOUND ( 'NONE', #77726, .T. ) ;
#90663 = CARTESIAN_POINT ( 'NONE',  ( -25.85456927314744391, -24.76652822093846140, 2.947631189768983528 ) ) ;
#90664 = ADVANCED_FACE ( 'NONE', ( #9355 ), #96107, .T. ) ;
#90665 = EDGE_CURVE ( 'NONE', #57717, #13722, #87487, .T. ) ;
#90666 = FACE_OUTER_BOUND ( 'NONE', #24721, .T. ) ;
#90667 = CARTESIAN_POINT ( 'NONE',  ( -44.52287095715006160, -23.47596703998600631, 11.44779298504229281 ) ) ;
#90668 = CARTESIAN_POINT ( 'NONE',  ( -13.79594968651775666, -13.80015156857029268, -1.500000000000002220 ) ) ;
#90669 = EDGE_CURVE ( 'NONE', #72641, #50584, #54247, .T. ) ;
#90670 = CARTESIAN_POINT ( 'NONE',  ( -19.33005188562793819, 9.364626179424670127, 11.49999999999998934 ) ) ;
#90671 = CARTESIAN_POINT ( 'NONE',  ( -25.68905881183481199, -24.57999888590886073, 3.430378900168168599 ) ) ;
#90672 = DIRECTION ( 'NONE',  ( 1.000000000000000000, 3.773278334444167608E-23, 8.201307833595939069E-29 ) ) ;
#90673 = CARTESIAN_POINT ( 'NONE',  ( -0.4909855769230799249, -6.376774720514410077, 19.14743589743590491 ) ) ;
#90674 = AXIS2_PLACEMENT_3D ( 'NONE', #27574, #73735, #22419 ) ;
#90675 = CARTESIAN_POINT ( 'NONE',  ( 10.87194125936840194, 20.03610521102953257, -1.500000000000002220 ) ) ;
#90676 = APPLICATION_PROTOCOL_DEFINITION ( 'international standard', 'config_control_design', 1994, #39445 ) ;
#90677 = CARTESIAN_POINT ( 'NONE',  ( -39.52287095715006870, -23.47593901973090524, -1.443836447538997092 ) ) ;
#90678 = CARTESIAN_POINT ( 'NONE',  ( -108.5228709571500616, -24.65952944569304961, 1.056160979905704123 ) ) ;
#90679 = CARTESIAN_POINT ( 'NONE',  ( -3.050325703546597822, 19.74810961616558913, 11.49999999999999645 ) ) ;
#90680 = DIRECTION ( 'NONE',  ( -3.773278334444167608E-23, 1.000000000000000000, 0.000000000000000000 ) ) ;
#90681 = AXIS2_PLACEMENT_3D ( 'NONE', #87628, #54804, #49078 ) ;
#90682 = CARTESIAN_POINT ( 'NONE',  ( -111.6228709571500559, -29.50250243563736774, 8.947779886222136270 ) ) ;
#90683 = FACE_OUTER_BOUND ( 'NONE', #82521, .T. ) ;
#90684 = ORIENTED_EDGE ( 'NONE', *, *, #54052, .F. ) ;
#90685 = CARTESIAN_POINT ( 'NONE',  ( -56.92287095715008860, -23.47593901973090524, -1.443836447538998202 ) ) ;
#90686 = EDGE_CURVE ( 'NONE', #34994, #63074, #80878, .T. ) ;
#90687 = CARTESIAN_POINT ( 'NONE',  ( -93.52287095715006160, -29.50250243563736774, 8.947779886222139822 ) ) ;
#90688 = CARTESIAN_POINT ( 'NONE',  ( 18.07971092720299922, 12.08445254275838465, -1.500000000000002220 ) ) ;
#90689 = CARTESIAN_POINT ( 'NONE',  ( -1.751198251822016161, 22.56127314141087581, 2.100000000000000089 ) ) ;
#90690 = AXIS2_PLACEMENT_3D ( 'NONE', #5783, #60594, #90520 ) ;
#90691 = CARTESIAN_POINT ( 'NONE',  ( -3.586273028688536257, -19.27814873881845514, -1.500000000000002220 ) ) ;
#90692 = CARTESIAN_POINT ( 'NONE',  ( 32.66876533700882845, 6.475225279485573360, -12.58926540598385557 ) ) ;
#90693 = EDGE_CURVE ( 'NONE', #71246, #14248, #64683, .T. ) ;
#90695 = ORIENTED_EDGE ( 'NONE', *, *, #88693, .T. ) ;
#90694 = CIRCLE ( 'NONE', #56751, 12.65241003308276113 ) ;
#90696 = DATE_AND_TIME ( #28296, #23159 ) ;
#90697 = VECTOR ( 'NONE', #12179, 1000.000000000000114 ) ;
#90698 = CARTESIAN_POINT ( 'NONE',  ( -91.62357784265581984, -24.66019654487199730, 8.947790411086115725 ) ) ;
#90699 = CARTESIAN_POINT ( 'NONE',  ( 2.677468215678941110, -6.376774720514418959, 20.83735685176740304 ) ) ;
#90700 = CARTESIAN_POINT ( 'NONE',  ( -3.437008290023895185, 20.19323497536227663, 11.49999999999999645 ) ) ;
#90701 = CARTESIAN_POINT ( 'NONE',  ( 10.64801255963128668, -6.475225279485572472, -27.03041135669327488 ) ) ;
#90702 = EDGE_CURVE ( 'NONE', #65855, #98879, #1466, .T. ) ;
#90703 = CARTESIAN_POINT ( 'NONE',  ( -8.160000000000000142, -10.65233964170348635, -1.621096496867198589 ) ) ;
#90704 = AXIS2_PLACEMENT_3D ( 'NONE', #82893, #12879, #49983 ) ;
#90705 = ORIENTED_EDGE ( 'NONE', *, *, #52540, .F. ) ;
#90706 = CARTESIAN_POINT ( 'NONE',  ( 24.71017632900191074, 3.356774720514427379, 1.647607965253217621 ) ) ;
#90707 = DIRECTION ( 'NONE',  ( -0.000000000000000000, 1.000000000000000000, -0.000000000000000000 ) ) ;
#90708 = LINE ( 'NONE', #82594, #33849 ) ;
#90709 = CARTESIAN_POINT ( 'NONE',  ( -110.9909297185884327, -25.15277794460069671, 6.986250878905948980 ) ) ;
#90710 = ORIENTED_EDGE ( 'NONE', *, *, #29663, .F. ) ;
#90711 = CARTESIAN_POINT ( 'NONE',  ( 5.993553214355093139, -6.376774720514417183, 20.20316077874593930 ) ) ;
#90712 = EDGE_CURVE ( 'NONE', #75862, #27531, #56053, .T. ) ;
#90713 = CARTESIAN_POINT ( 'NONE',  ( -3.733506833432379768, 22.73668382284982314, 11.49999999999999645 ) ) ;
#90714 = B_SPLINE_CURVE_WITH_KNOTS ( 'NONE', 3,
 ( #72128, #17319, #1608, #54894 ),
 .UNSPECIFIED., .F., .F.,
 ( 4, 4 ),
 ( 0.000000000000000000, 9.999999999998897304E-05 ),
 .UNSPECIFIED. ) ;
#90715 = CARTESIAN_POINT ( 'NONE',  ( -4.374245501123523283, 22.36648047097513725, -1.500000000000002220 ) ) ;
#90716 = CARTESIAN_POINT ( 'NONE',  ( -110.5947687508519692, -23.85049219812686516, 10.88485053497526955 ) ) ;
#90717 = DIRECTION ( 'NONE',  ( 1.000000000000000000, 0.000000000000000000, 0.000000000000000000 ) ) ;
#90718 = CARTESIAN_POINT ( 'NONE',  ( -50.29954090288276802, -25.19533727061342177, 3.296115780377149029 ) ) ;
#90719 = CARTESIAN_POINT ( 'NONE',  ( 23.57151214508650128, 3.870844576848782668E-15, 0.5000000000000000000 ) ) ;
#90720 = B_SPLINE_CURVE_WITH_KNOTS ( 'NONE', 3,
 ( #79647, #33479, #25870, #13127 ),
 .UNSPECIFIED., .F., .F.,
 ( 4, 4 ),
 ( 0.000000000000000000, 9.999999999999592548E-05 ),
 .UNSPECIFIED. ) ;
#90721 = CARTESIAN_POINT ( 'NONE',  ( -99.37735140507533060, -25.31582232917384800, 5.086082719468676849 ) ) ;
#90722 = ADVANCED_FACE ( 'NONE', ( #34704 ), #33197, .T. ) ;
#90723 = CARTESIAN_POINT ( 'NONE',  ( 21.14253370195585546, 5.708146584608840612, -1.500000000000002220 ) ) ;
#90724 = CARTESIAN_POINT ( 'NONE',  ( 7.176111537430461595, -5.876774720514424288, 21.53668079471899333 ) ) ;
#90725 = CARTESIAN_POINT ( 'NONE',  ( -87.63525289881717129, -23.96169478059713498, 10.65365249895718058 ) ) ;
#90726 = CARTESIAN_POINT ( 'NONE',  ( -33.52287095715007581, -24.51387760970725083, 9.387446482453428942 ) ) ;
#90727 = LINE ( 'NONE', #50176, #50897 ) ;
#90728 = LINE ( 'NONE', #21694, #88978 ) ;
#90729 = FACE_OUTER_BOUND ( 'NONE', #30617, .T. ) ;
#90730 = ORIENTED_EDGE ( 'NONE', *, *, #68506, .F. ) ;
#90731 = CARTESIAN_POINT ( 'NONE',  ( 17.75789855128238770, 10.12834119215567164, 11.49999999999998934 ) ) ;
#90732 = VERTEX_POINT ( 'NONE', #79366 ) ;
#90733 = EDGE_LOOP ( 'NONE', ( #29453, #32342, #22350, #40218 ) ) ;
#90734 = ORIENTED_EDGE ( 'NONE', *, *, #14481, .F. ) ;
#90735 = ORIENTED_EDGE ( 'NONE', *, *, #70845, .F. ) ;
#90736 = EDGE_CURVE ( 'NONE', #37215, #62489, #40810, .T. ) ;
#90737 = CARTESIAN_POINT ( 'NONE',  ( 22.18053613645642841, 6.281410551025238043, 11.49999999999998934 ) ) ;
#90738 = CARTESIAN_POINT ( 'NONE',  ( -61.53887241091420179, -24.51314013834316086, 0.6176544820404138436 ) ) ;
#90739 = CARTESIAN_POINT ( 'NONE',  ( 15.69265952521009488, -12.80212094623039576, -1.500000000000002220 ) ) ;
#90740 = VERTEX_POINT ( 'NONE', #71771 ) ;
#90741 = CARTESIAN_POINT ( 'NONE',  ( -90.58953762381671027, -25.00182538069145366, 7.747789668545099317 ) ) ;
#90742 = CARTESIAN_POINT ( 'NONE',  ( -41.18093725576135711, -25.30970379484010735, 5.386210342106713789 ) ) ;
#90743 = CARTESIAN_POINT ( 'NONE',  ( -95.58789998751944950, -24.63355581998386157, 0.9682620441943944334 ) ) ;
#90744 = CARTESIAN_POINT ( 'NONE',  ( 29.73860345376319358, -1.477225279485574028, -1.352392034746782823 ) ) ;
#90746 = VERTEX_POINT ( 'NONE', #64179 ) ;
#90745 = CARTESIAN_POINT ( 'NONE',  ( 17.68986881342592454, -12.14045624799103962, 11.49999999999999645 ) ) ;
#90747 = CARTESIAN_POINT ( 'NONE',  ( -100.5895376238167245, -23.47593901973091235, -1.443836447539001089 ) ) ;
#90748 = ORIENTED_EDGE ( 'NONE', *, *, #62758, .F. ) ;
#90749 = CARTESIAN_POINT ( 'NONE',  ( 16.32338804990218151, -12.73490195939593406, -1.500000000000002220 ) ) ;
#90750 = CIRCLE ( 'NONE', #29175, 251.9358649670780892 ) ;
#90751 = ORIENTED_EDGE ( 'NONE', *, *, #43311, .T. ) ;
#90752 = CARTESIAN_POINT ( 'NONE',  ( -113.6228709571500559, -24.65952944569304961, 1.056160979905706565 ) ) ;
#90753 = ORIENTED_EDGE ( 'NONE', *, *, #98592, .F. ) ;
#90754 = FACE_OUTER_BOUND ( 'NONE', #5771, .T. ) ;
#90755 = VECTOR ( 'NONE', #91474, 1000.000000000000000 ) ;
#90756 = ORIENTED_EDGE ( 'NONE', *, *, #35950, .F. ) ;
#90757 = CARTESIAN_POINT ( 'NONE',  ( -19.40599490818632233, 7.965113791304038848, -1.500000000000002220 ) ) ;
#90758 = CARTESIAN_POINT ( 'NONE',  ( -13.73438224071023761, 17.16576579689093762, 11.49999999999999645 ) ) ;
#90759 = CARTESIAN_POINT ( 'NONE',  ( -89.62358331694552760, -24.66019654487199730, 8.947790411086115725 ) ) ;
#90760 = CARTESIAN_POINT ( 'NONE',  ( -5.199590022849982063, -21.90925200621149571, 11.49999999999998934 ) ) ;
#90761 = CIRCLE ( 'NONE', #88953, 6.099999999999999645 ) ;
#90762 = CARTESIAN_POINT ( 'NONE',  ( 5.724939850241691275, 20.19279902153374096, -1.500000000000002220 ) ) ;
#90763 = CARTESIAN_POINT ( 'NONE',  ( 6.404294203292168142, -6.376774720514415407, 20.09052689972686423 ) ) ;
#90764 = CARTESIAN_POINT ( 'NONE',  ( -72.62287095715005592, -24.64898659630367916, 1.056161002820824368 ) ) ;
#90765 = CARTESIAN_POINT ( 'NONE',  ( 14.98985047787450320, -3.577630190450212577, -26.76169638709854226 ) ) ;
#90766 = ORIENTED_EDGE ( 'NONE', *, *, #65035, .T. ) ;
#90767 = CIRCLE ( 'NONE', #81065, 10.49999999999999112 ) ;
#90768 = B_SPLINE_CURVE_WITH_KNOTS ( 'NONE', 3,
 ( #21558, #84963, #99671, #23553, #45426, #52531 ),
 .UNSPECIFIED., .F., .F.,
 ( 4, 2, 4 ),
 ( 0.000000000000000000, 0.001380901958385383774, 0.002761803916770767548 ),
 .UNSPECIFIED. ) ;
#90769 = ORIENTED_EDGE ( 'NONE', *, *, #47715, .F. ) ;
#90770 = CIRCLE ( 'NONE', #64877, 1.020000000000000018 ) ;
#90771 = ORIENTED_EDGE ( 'NONE', *, *, #16312, .F. ) ;
#90772 = DIRECTION ( 'NONE',  ( -1.000000000000000000, 0.000000000000000000, 0.000000000000000000 ) ) ;
#90773 = CIRCLE ( 'NONE', #85920, 6.119803529381341534 ) ;
#90774 = CARTESIAN_POINT ( 'NONE',  ( 14.45597713831175035, -15.85640774750547344, -1.500000000000002220 ) ) ;
#90775 = EDGE_CURVE ( 'NONE', #65689, #46666, #95100, .T. ) ;
#90776 = LINE ( 'NONE', #43608, #32693 ) ;
#90777 = ORIENTED_EDGE ( 'NONE', *, *, #14933, .T. ) ;
#90778 = CARTESIAN_POINT ( 'NONE',  ( -9.620199658202244208, 18.81650055922726494, 11.49999999999998934 ) ) ;
#90779 = CARTESIAN_POINT ( 'NONE',  ( -93.62287095715004170, -23.48783264082478794, -1.443836473390063713 ) ) ;
#90780 = EDGE_CURVE ( 'NONE', #85400, #86130, #11618, .T. ) ;
#90781 = CARTESIAN_POINT ( 'NONE',  ( -64.58769910004320991, -24.34968618360933590, 0.1864209137778785330 ) ) ;
#90782 = DIRECTION ( 'NONE',  ( 0.7512896232465892110, 0.000000000000000000, 0.6599726524652352877 ) ) ;
#90783 = CARTESIAN_POINT ( 'NONE',  ( -54.52287095715006870, -29.50250243563736774, 8.947779886222146928 ) ) ;
#90784 = CARTESIAN_POINT ( 'NONE',  ( -99.12380231474227799, -25.26431306044052150, 4.001575155705512366 ) ) ;
#90785 = CARTESIAN_POINT ( 'NONE',  ( -7.320055889550622474, -20.87099576385019972, -1.500000000000002220 ) ) ;
#90786 = EDGE_CURVE ( 'NONE', #60457, #8399, #58058, .T. ) ;
#90787 = CARTESIAN_POINT ( 'NONE',  ( -30.49308942697465952, -23.47593901973084485, -1.443836476861628970 ) ) ;
#90788 = EDGE_CURVE ( 'NONE', #51587, #534, #40352, .T. ) ;
#90789 = CARTESIAN_POINT ( 'NONE',  ( -56.52287095715007581, -24.33927499327853994, 9.819080762295817166 ) ) ;
#90790 = CARTESIAN_POINT ( 'NONE',  ( -69.52287095715006160, -23.47593901973090169, -1.443836447538996870 ) ) ;
#90791 = CARTESIAN_POINT ( 'NONE',  ( 30.53060340732036693, 5.168534691225920241, 8.812171101699174613 ) ) ;
#90792 = EDGE_CURVE ( 'NONE', #15522, #87638, #55315, .T. ) ;
#90793 = CARTESIAN_POINT ( 'NONE',  ( -100.5540451804232589, -24.15503026093913874, -0.2815557561904538653 ) ) ;
#90794 = CARTESIAN_POINT ( 'NONE',  ( -18.32239908988104204, -6.426282940459683068, 11.49999999999998934 ) ) ;
#90795 = CARTESIAN_POINT ( 'NONE',  ( -2.881439591185620319, 21.19155266312798958, 11.49999999999998934 ) ) ;
#90796 = CARTESIAN_POINT ( 'NONE',  ( -66.58953762381672448, -23.48783264082478439, -1.443836473390067487 ) ) ;
#90797 = DIRECTION ( 'NONE',  ( -3.773278334453079618E-23, 0.9999999999976377785, 2.173523156925979975E-06 ) ) ;
#90798 = CARTESIAN_POINT ( 'NONE',  ( -123.5228709571500616, -23.72747288104470442, -1.053458166803224794 ) ) ;
#90799 = CARTESIAN_POINT ( 'NONE',  ( -60.62287095715005592, -23.48786465467241058, 11.44779295918254824 ) ) ;
#90800 = CARTESIAN_POINT ( 'NONE',  ( 13.37577147909557773, 18.27418014603220442, -1.500000000000002220 ) ) ;
#90801 = B_SPLINE_CURVE_WITH_KNOTS ( 'NONE', 3,
 ( #6543, #77535, #47115, #91762, #46613, #78028 ),
 .UNSPECIFIED., .F., .F.,
 ( 4, 2, 4 ),
 ( 1.570755371634415583E-05, 0.001396183895866091439, 0.002776660238015838614 ),
 .UNSPECIFIED. ) ;
#90802 = VERTEX_POINT ( 'NONE', #90480 ) ;
#90803 = LINE ( 'NONE', #13659, #51446 ) ;
#90804 = CARTESIAN_POINT ( 'NONE',  ( -61.59189125704995860, -29.50249900881161835, 7.371157290072014590 ) ) ;
#90805 = CARTESIAN_POINT ( 'NONE',  ( 6.388261542594571019, -18.74682169789839392, 11.49999999999999645 ) ) ;
#90806 = DIRECTION ( 'NONE',  ( -1.000000000000000000, 0.000000000000000000, 0.000000000000000000 ) ) ;
#90807 = CARTESIAN_POINT ( 'NONE',  ( 29.80070917940689412, -5.965225279485572685, 27.39560796525321607 ) ) ;
#90808 = VERTEX_POINT ( 'NONE', #60549 ) ;
#90809 = CARTESIAN_POINT ( 'NONE',  ( -5.891837592278976743, -6.376774720514418959, 20.62654306927474934 ) ) ;
#90810 = DIRECTION ( 'NONE',  ( -0.000000000000000000, 1.000000000000000000, -0.000000000000000000 ) ) ;
#90811 = CARTESIAN_POINT ( 'NONE',  ( -7.347880794884120722E-16, -5.356774720514425603, -6.000000000000000888 ) ) ;
#90812 = CARTESIAN_POINT ( 'NONE',  ( 14.26105141482337935, -16.23293960606763520, 11.49999999999998934 ) ) ;
#90813 = LINE ( 'NONE', #51257, #96637 ) ;
#90814 = CARTESIAN_POINT ( 'NONE',  ( 19.05472526407214673, 3.605321472892077050, -1.500000000000002220 ) ) ;
#90815 = CARTESIAN_POINT ( 'NONE',  ( 15.32643653063177958, -3.577630190450218350, -27.14485409495429380 ) ) ;
#90816 = CARTESIAN_POINT ( 'NONE',  ( 282.9764569301858046, 5.965225279485572685, 20.79159422840526616 ) ) ;
#90817 = CARTESIAN_POINT ( 'NONE',  ( 18.46520180437041603, 7.126043738416648843, 11.49999999999998934 ) ) ;
#90818 = ORIENTED_EDGE ( 'NONE', *, *, #10590, .F. ) ;
#90819 = CARTESIAN_POINT ( 'NONE',  ( 12.22771034161782566, -16.27230226814707947, 11.49999999999999645 ) ) ;
#90820 = CARTESIAN_POINT ( 'NONE',  ( 10.40220176116686979, 5.447062032237068863, -27.19353416079722763 ) ) ;
#90821 = AXIS2_PLACEMENT_3D ( 'NONE', #59199, #59702, #37358 ) ;
#90822 = DIRECTION ( 'NONE',  ( -1.000000000000000000, 0.000000000000000000, 0.000000000000000000 ) ) ;
#90823 = ORIENTED_EDGE ( 'NONE', *, *, #21678, .F. ) ;
#90824 = CARTESIAN_POINT ( 'NONE',  ( -30.59167141582165783, -24.92410949913933393, 1.600845668900849894 ) ) ;
#90825 = CARTESIAN_POINT ( 'NONE',  ( -106.6228709571500559, -23.47596703998600631, 11.44779298504227860 ) ) ;
#90826 = CARTESIAN_POINT ( 'NONE',  ( -105.6228709571500417, -29.50249982740957577, 7.747779886224967605 ) ) ;
#90827 = CARTESIAN_POINT ( 'NONE',  ( -82.62287095715005592, -23.48786465467241413, 11.44779295918254647 ) ) ;
#90828 = DIRECTION ( 'NONE',  ( 0.000000000000000000, 0.000000000000000000, -1.000000000000000000 ) ) ;
#90829 = CARTESIAN_POINT ( 'NONE',  ( 1.781536345648733199, 20.00535218256611358, -1.500000000000002220 ) ) ;
#90830 = CARTESIAN_POINT ( 'NONE',  ( -24.90875734969025501, -6.475225279485573360, 29.49402280011861777 ) ) ;
#90831 = VERTEX_POINT ( 'NONE', #4751 ) ;
#90832 = DIRECTION ( 'NONE',  ( 0.06486421869277853025, 0.000000000000000000, -0.9978940991575085961 ) ) ;
#90833 = AXIS2_PLACEMENT_3D ( 'NONE', #47872, #32633, #86920 ) ;
#90834 = CARTESIAN_POINT ( 'NONE',  ( -16.48365427610503886, -15.78576583860491489, 11.49999999999999645 ) ) ;
#90835 = CARTESIAN_POINT ( 'NONE',  ( -30.47287095715008576, -24.97456920234173339, 2.208563660530530992 ) ) ;
#90836 = FACE_OUTER_BOUND ( 'NONE', #12287, .T. ) ;
#90837 = LINE ( 'NONE', #58897, #80840 ) ;
#90838 = AXIS2_PLACEMENT_3D ( 'NONE', #520, #33468, #40089 ) ;
#90839 = CARTESIAN_POINT ( 'NONE',  ( -123.5228709571500616, -29.50250243563736774, 8.947779886222134493 ) ) ;
#90840 = EDGE_CURVE ( 'NONE', #41495, #58299, #50451, .T. ) ;
#90841 = AXIS2_PLACEMENT_3D ( 'NONE', #81572, #19158, #27778 ) ;
#90842 = DIRECTION ( 'NONE',  ( -0.000000000000000000, 1.000000000000000000, -0.000000000000000000 ) ) ;
#90843 = EDGE_CURVE ( 'NONE', #49731, #53050, #95397, .T. ) ;
#90844 = CARTESIAN_POINT ( 'NONE',  ( -51.53941112929729940, -25.30419751004783890, 5.186272124421679841 ) ) ;
#90845 = ORIENTED_EDGE ( 'NONE', *, *, #67948, .F. ) ;
#90846 = CARTESIAN_POINT ( 'NONE',  ( -13.67433444753018534, -15.09191755960682890, -1.500000000000002220 ) ) ;
#90847 = ORIENTED_EDGE ( 'NONE', *, *, #92513, .F. ) ;
#90848 = CARTESIAN_POINT ( 'NONE',  ( 22.25235761598246143, -5.642936543268669780, -1.500000000000002220 ) ) ;
#90849 = LINE ( 'NONE', #83729, #48561 ) ;
#90850 = ORIENTED_EDGE ( 'NONE', *, *, #87451, .F. ) ;
#90851 = CARTESIAN_POINT ( 'NONE',  ( -101.6228709571500701, -23.47596703998600631, 11.44779298504227683 ) ) ;
#90852 = CARTESIAN_POINT ( 'NONE',  ( -94.55620429048339304, -23.48783264082478084, -1.443836473390064157 ) ) ;
#90853 = CARTESIAN_POINT ( 'NONE',  ( -38.52287095715006870, -24.66019654487199730, 8.947790411086121054 ) ) ;
#90855 = ORIENTED_EDGE ( 'NONE', *, *, #74447, .F. ) ;
#90854 = CARTESIAN_POINT ( 'NONE',  ( 16.87399902462237478, -12.92443306546820736, 11.49999999999999645 ) ) ;
#90856 = ORIENTED_EDGE ( 'NONE', *, *, #27249, .T. ) ;
#90857 = CARTESIAN_POINT ( 'NONE',  ( -7.471142097702432316, -20.87072022463130239, -1.500000000000002220 ) ) ;
#90858 = CARTESIAN_POINT ( 'NONE',  ( -16.38011734009650411, 12.53836025512309149, -1.500000000000002220 ) ) ;
#90859 = ORIENTED_EDGE ( 'NONE', *, *, #59922, .T. ) ;
#90860 = ORIENTED_EDGE ( 'NONE', *, *, #16061, .T. ) ;
#90861 = DIRECTION ( 'NONE',  ( 1.000000000000000000, 3.773278334444166432E-23, 8.201307841325785021E-29 ) ) ;
#90862 = B_SPLINE_CURVE_WITH_KNOTS ( 'NONE', 3,
 ( #15282, #60490, #46245, #99511 ),
 .UNSPECIFIED., .F., .F.,
 ( 4, 4 ),
 ( 0.000000000000000000, 9.999999999998897304E-05 ),
 .UNSPECIFIED. ) ;
#90863 = CARTESIAN_POINT ( 'NONE',  ( -36.52287095715006870, -24.64898659630367916, 1.056161002820819261 ) ) ;
#90864 = VERTEX_POINT ( 'NONE', #97590 ) ;
#90865 = ORIENTED_EDGE ( 'NONE', *, *, #60326, .F. ) ;
#90866 = CARTESIAN_POINT ( 'NONE',  ( -76.52287095715007581, -29.50248528299804818, 1.056150453629038477 ) ) ;
#90868 = CARTESIAN_POINT ( 'NONE',  ( -41.57627760764538749, -24.66019654487199375, 8.947790411086122830 ) ) ;
#90867 = B_SPLINE_CURVE_WITH_KNOTS ( 'NONE', 3,
 ( #36849, #50574, #66818, #65820 ),
 .UNSPECIFIED., .F., .F.,
 ( 4, 4 ),
 ( 0.000000000000000000, 9.999999999998900014E-05 ),
 .UNSPECIFIED. ) ;
#90869 = CARTESIAN_POINT ( 'NONE',  ( -94.62287095715005592, -24.64965695001469115, 8.947790433994180503 ) ) ;
#90870 = CARTESIAN_POINT ( 'NONE',  ( -18.04518632387085830, 10.29925911722504317, -1.500000000000002220 ) ) ;
#90871 = CARTESIAN_POINT ( 'NONE',  ( -8.334044162642690878, 20.12857247364870616, 11.49999999999999645 ) ) ;
#90872 = CARTESIAN_POINT ( 'NONE',  ( -39.44865907921395376, -25.27406546170053048, 4.125344378457973527 ) ) ;
#90873 = CARTESIAN_POINT ( 'NONE',  ( -122.2228709571500787, -23.47593901973090169, -1.443836447538996426 ) ) ;
#90874 = DIRECTION ( 'NONE',  ( 0.000000000000000000, 0.000000000000000000, 1.000000000000000000 ) ) ;
#90875 = CARTESIAN_POINT ( 'NONE',  ( -21.57557905285345612, -6.117077608415351087, 11.49999999999998934 ) ) ;
#90876 = CARTESIAN_POINT ( 'NONE',  ( -51.29599548036032530, -25.31296608742942666, 4.016965581434211785 ) ) ;
#90877 = EDGE_CURVE ( 'NONE', #40078, #55078, #67349, .T. ) ;
#90878 = ORIENTED_EDGE ( 'NONE', *, *, #33047, .F. ) ;
#90879 = CARTESIAN_POINT ( 'NONE',  ( -98.52287095715006160, -24.64965694238575011, 8.947790433994194714 ) ) ;
#90880 = CARTESIAN_POINT ( 'NONE',  ( 32.54003107466018463, 4.047905215973556459, -1.500050581001865169 ) ) ;
#90881 = ORIENTED_EDGE ( 'NONE', *, *, #62270, .F. ) ;
#90882 = VERTEX_POINT ( 'NONE', #21445 ) ;
#90883 = AXIS2_PLACEMENT_3D ( 'NONE', #83039, #29264, #84050 ) ;
#90884 = CARTESIAN_POINT ( 'NONE',  ( -99.47252348226193419, -25.29900225115328283, 5.640920301989122976 ) ) ;
#90885 = VERTEX_POINT ( 'NONE', #82365 ) ;
#90886 = CARTESIAN_POINT ( 'NONE',  ( 21.14028111218437900, -2.610574537768086234, -1.500000000000002220 ) ) ;
#90887 = ORIENTED_EDGE ( 'NONE', *, *, #68543, .F. ) ;
#90888 = CARTESIAN_POINT ( 'NONE',  ( -6.275748223059703257, -5.876774720514411854, 19.59984006504824805 ) ) ;
#90889 = CARTESIAN_POINT ( 'NONE',  ( -11.20027426441765961, 17.80179601997297212, -1.500000000000002220 ) ) ;
#90890 = FACE_OUTER_BOUND ( 'NONE', #53697, .T. ) ;
#90891 = CARTESIAN_POINT ( 'NONE',  ( 22.03932947713327906, 5.445304565557160359, -1.500000000000002220 ) ) ;
#90892 = EDGE_CURVE ( 'NONE', #95924, #80254, #59991, .T. ) ;
#90893 = CARTESIAN_POINT ( 'NONE',  ( -113.5228709571500900, -23.72773821059536914, 11.05748984161097326 ) ) ;
#90894 = B_SPLINE_CURVE_WITH_KNOTS ( 'NONE', 3,
 ( #15954, #78350, #1748, #8851 ),
 .UNSPECIFIED., .F., .F.,
 ( 4, 4 ),
 ( 1.866604411097509178E-09, 0.0003958024117146408984 ),
 .UNSPECIFIED. ) ;
#90895 = DIRECTION ( 'NONE',  ( -0.1311553622875919756, 6.845827386180409975E-16, -0.9913618264504692190 ) ) ;
#90896 = CARTESIAN_POINT ( 'NONE',  ( -16.24880213243413607, 14.73142910551002238, -1.500000000000002220 ) ) ;
#90897 = CARTESIAN_POINT ( 'NONE',  ( -87.59864562871899807, -23.73766607897671221, -1.055555164236430032 ) ) ;
#90898 = ORIENTED_EDGE ( 'NONE', *, *, #2762, .F. ) ;
#90899 = CARTESIAN_POINT ( 'NONE',  ( -40.21512553332997442, -25.29405891411934348, 5.531795786000103021 ) ) ;
#90900 = ADVANCED_FACE ( 'NONE', ( #74259 ), #68147, .F. ) ;
#90901 = EDGE_CURVE ( 'NONE', #21450, #18000, #99073, .T. ) ;
#90902 = CARTESIAN_POINT ( 'NONE',  ( -84.50667423978107706, -24.35071581493543391, 9.817618358456027039 ) ) ;
#90903 = CIRCLE ( 'NONE', #3441, 0.2499999999997798983 ) ;
#90904 = EDGE_CURVE ( 'NONE', #13904, #89924, #42826, .T. ) ;
#90905 = CARTESIAN_POINT ( 'NONE',  ( -126.6228709571500843, -23.47596703998600631, 11.44779298504227860 ) ) ;
#90906 = APPROVAL_PERSON_ORGANIZATION ( #46503, #45738, #99761 ) ;
#90907 = DIRECTION ( 'NONE',  ( 0.000000000000000000, -2.173523156925980399E-06, 0.9999999999976378895 ) ) ;
#90908 = CARTESIAN_POINT ( 'NONE',  ( 13.65650298889772962, 16.33668418983593185, -1.500000000000002220 ) ) ;
#90909 = DIRECTION ( 'NONE',  ( -3.773278334453079030E-23, 0.9999999999976377785, 2.173523156925979128E-06 ) ) ;
#90910 = EDGE_CURVE ( 'NONE', #25882, #49692, #85471, .T. ) ;
#90911 = CARTESIAN_POINT ( 'NONE',  ( -81.48149462243459595, -29.50249666744127808, 6.293933732382250845 ) ) ;
#90912 = CARTESIAN_POINT ( 'NONE',  ( -85.62652016793876442, -24.83618233451450408, 1.606449574219535270 ) ) ;
#90913 = LINE ( 'NONE', #60483, #79977 ) ;
#90914 = CARTESIAN_POINT ( 'NONE',  ( -32.62287095715004881, -23.47593901973091235, -1.443836447539013301 ) ) ;
#90915 = ORIENTED_EDGE ( 'NONE', *, *, #61215, .F. ) ;
#90916 = CARTESIAN_POINT ( 'NONE',  ( -99.22308953234012563, -25.14696225287006826, 7.022768084356811435 ) ) ;
#90917 = CARTESIAN_POINT ( 'NONE',  ( 13.10555085358618221, -14.64361678476065087, 11.49999999999999645 ) ) ;
#90918 = CARTESIAN_POINT ( 'NONE',  ( -75.58953762381672448, -24.99156044556202616, 7.747789690856173195 ) ) ;
#90919 = CARTESIAN_POINT ( 'NONE',  ( 10.27515206207115739, -5.152774720514427642, -28.04856579873300149 ) ) ;
#90920 = EDGE_CURVE ( 'NONE', #24964, #28708, #40740, .T. ) ;
#90921 = EDGE_LOOP ( 'NONE', ( #64297, #88390, #21848, #91602 ) ) ;
#90922 = CARTESIAN_POINT ( 'NONE',  ( 0.000000000000000000, 1.530000000000000027, -0.3849999999999998979 ) ) ;
#90923 = DIRECTION ( 'NONE',  ( 0.000000000000000000, 0.000000000000000000, 1.000000000000000000 ) ) ;
#90924 = CARTESIAN_POINT ( 'NONE',  ( -25.53324729430006101, -24.92678253223225582, 5.128894466507167849 ) ) ;
#90925 = PLANE ( 'NONE',  #94741 ) ;
#90926 = CARTESIAN_POINT ( 'NONE',  ( 6.578723047037327909, -18.57437435983987584, -1.500000000000002220 ) ) ;
#90927 = ORIENTED_EDGE ( 'NONE', *, *, #3081, .F. ) ;
#90928 = LINE ( 'NONE', #89934, #61880 ) ;
#90929 = CARTESIAN_POINT ( 'NONE',  ( -70.62287095715002749, -23.85196035786900381, -0.8779234886474986954 ) ) ;
#90930 = COORDINATED_UNIVERSAL_TIME_OFFSET ( 0, 0, .AHEAD. ) ;
#90931 = ORIENTED_EDGE ( 'NONE', *, *, #55317, .F. ) ;
#90932 = DIRECTION ( 'NONE',  ( -1.000000000000000000, 0.000000000000000000, 0.000000000000000000 ) ) ;
#90933 = CARTESIAN_POINT ( 'NONE',  ( 33.96422015159436114, 5.965225279485572685, -7.233236000911337449 ) ) ;
#90934 = CARTESIAN_POINT ( 'NONE',  ( -81.88534077628074215, -25.23679622552714363, 6.293943003980942308 ) ) ;
#90935 = CARTESIAN_POINT ( 'NONE',  ( -118.6267481313898173, -23.96119346886881374, -0.6495511937832023630 ) ) ;
#90936 = CARTESIAN_POINT ( 'NONE',  ( -121.5895376238167245, -24.65952944569305316, 1.056160979905702790 ) ) ;
#90937 = CARTESIAN_POINT ( 'NONE',  ( -124.6228709571500559, -23.47593901973091235, -1.443836447538997536 ) ) ;
#90938 = CARTESIAN_POINT ( 'NONE',  ( -120.5895376238167103, -23.47593901973091235, -1.443836447538997536 ) ) ;
#90939 = CARTESIAN_POINT ( 'NONE',  ( 1.534201407001029027, 19.92515851932037663, -1.500000000000002220 ) ) ;
#90940 = EDGE_CURVE ( 'NONE', #61907, #18192, #66177, .T. ) ;
#90941 = CARTESIAN_POINT ( 'NONE',  ( -95.58953762381671027, -25.00182538069145366, 7.747789668545099317 ) ) ;
#90942 = CARTESIAN_POINT ( 'NONE',  ( -0.03668282068714227157, -22.57511205935180598, 1.639801994305458699 ) ) ;
#90943 = ORIENTED_EDGE ( 'NONE', *, *, #54831, .T. ) ;
#90944 = FACE_OUTER_BOUND ( 'NONE', #9889, .T. ) ;
#90945 = DIRECTION ( 'NONE',  ( -1.000000000000000000, -0.000000000000000000, 0.000000000000000000 ) ) ;
#90946 = EDGE_CURVE ( 'NONE', #76643, #49424, #26187, .T. ) ;
#90947 = PLANE ( 'NONE',  #11315 ) ;
#90948 = FACE_OUTER_BOUND ( 'NONE', #44443, .T. ) ;
#90949 = CARTESIAN_POINT ( 'NONE',  ( -28.52287095715005805, -24.48836230353387222, 1.056161703005638719 ) ) ;
#90950 = CARTESIAN_POINT ( 'NONE',  ( -107.5228709571501042, -24.66019654487199730, 8.947790411086115725 ) ) ;
#90951 = AXIS2_PLACEMENT_3D ( 'NONE', #46002, #97775, #5927 ) ;
#90952 = EDGE_CURVE ( 'NONE', #13162, #98350, #37192, .T. ) ;
#90953 = CARTESIAN_POINT ( 'NONE',  ( 19.75748517575715368, 0.3587747205144265483, 28.87153971905864580 ) ) ;
#90954 = CARTESIAN_POINT ( 'NONE',  ( -45.62287095715004881, -25.00182538069145011, 7.747789668545099317 ) ) ;
#90955 = VERTEX_POINT ( 'NONE', #58545 ) ;
#90956 = CARTESIAN_POINT ( 'NONE',  ( -100.6228709571500559, -29.50248528299804818, 1.056150453629042030 ) ) ;
#90957 = CARTESIAN_POINT ( 'NONE',  ( 5.864177746775673050, -6.376774720514426065, 21.69926562011473337 ) ) ;
#90958 = VERTEX_POINT ( 'NONE', #19963 ) ;
#90959 = CARTESIAN_POINT ( 'NONE',  ( -2.356373108420451334, 20.14613781377289214, -1.500000000000002220 ) ) ;
#90960 = LINE ( 'NONE', #68133, #38763 ) ;
#90961 = CARTESIAN_POINT ( 'NONE',  ( -49.62287095715003460, -24.51283580621364067, 0.6167428607019802556 ) ) ;
#90962 = FACE_OUTER_BOUND ( 'NONE', #40815, .T. ) ;
#90963 = VERTEX_POINT ( 'NONE', #81871 ) ;
#90964 = CARTESIAN_POINT ( 'NONE',  ( -77.52287095715004739, -23.95044443724992078, 10.65354141964649415 ) ) ;
#90965 = CARTESIAN_POINT ( 'NONE',  ( -105.6228709571500275, -25.00158670708909625, 2.256160236439166411 ) ) ;
#90966 = VECTOR ( 'NONE', #51377, 1000.000000000000000 ) ;
#90967 = CARTESIAN_POINT ( 'NONE',  ( 17.53424486177994623, -9.724335930198575895, -1.500000000000002220 ) ) ;
#90968 = CARTESIAN_POINT ( 'NONE',  ( 13.68530018921192060, -16.06810839794082924, 11.49999999999999645 ) ) ;
#90969 = LOCAL_TIME ( 0, 54, 15.00000000000000000, #61245 ) ;
#90970 = CARTESIAN_POINT ( 'NONE',  ( -28.70172027432288431, -24.98211893518114124, 7.134191928894627388 ) ) ;
#90971 = CARTESIAN_POINT ( 'NONE',  ( -70.54635493862706141, -24.40133493613049964, 9.663955038902802386 ) ) ;
#90972 = CARTESIAN_POINT ( 'NONE',  ( 15.76968270297436625, 15.47746201419723100, -1.500000000000002220 ) ) ;
#90974 = CARTESIAN_POINT ( 'NONE',  ( -6.383830130275963910, 19.51498944528526991, 11.49999999999998934 ) ) ;
#90973 = APPROVAL ( #81329, 'UNSPECIFIED' ) ;
#90975 = CARTESIAN_POINT ( 'NONE',  ( -50.52287095715006160, -29.50249982740957577, 7.747779886224967605 ) ) ;
#90976 = CARTESIAN_POINT ( 'NONE',  ( 31.20850673110457763, 5.144960210277549351, -4.610511713824573476 ) ) ;
#90977 = CARTESIAN_POINT ( 'NONE',  ( -114.5228709571500190, -24.66019654487200441, 8.947790411086110396 ) ) ;
#90978 = EDGE_LOOP ( 'NONE', ( #76915, #61161, #81827, #62420 ) ) ;
#90979 = LINE ( 'NONE', #12847, #94850 ) ;
#90980 = DIRECTION ( 'NONE',  ( 0.09824042138329590335, -4.470611911092166224E-17, 0.9951627101165079203 ) ) ;
#90981 = VERTEX_POINT ( 'NONE', #12349 ) ;
#90982 = ORIENTED_EDGE ( 'NONE', *, *, #45717, .T. ) ;
#90983 = CARTESIAN_POINT ( 'NONE',  ( -114.5228709571500616, -29.50247984919015209, -1.443849546365048253 ) ) ;
#90984 = FACE_OUTER_BOUND ( 'NONE', #52131, .T. ) ;
#90985 = CARTESIAN_POINT ( 'NONE',  ( -0.4362980769230789257, -6.376774720514411854, 19.46153846153846345 ) ) ;
#90986 = CARTESIAN_POINT ( 'NONE',  ( 18.07347782881280907, 9.871946371954690491, -1.500000000000002220 ) ) ;
#90987 = CARTESIAN_POINT ( 'NONE',  ( 17.62533924669398999, -12.40915598911231577, 11.49999999999999645 ) ) ;
#90988 = ORIENTED_EDGE ( 'NONE', *, *, #88043, .F. ) ;
#90989 = CARTESIAN_POINT ( 'NONE',  ( -110.5228709571500616, -29.50250243563736774, 8.947779886222136270 ) ) ;
#90990 = CARTESIAN_POINT ( 'NONE',  ( 282.9764569301858046, -4.540774720514427543, 20.79159422840526616 ) ) ;
#90991 = CARTESIAN_POINT ( 'NONE',  ( -2.124831620219566730, 22.23837930986240607, -1.500000000000002220 ) ) ;
#90992 = CARTESIAN_POINT ( 'NONE',  ( -80.05243144761681151, -25.27875073300474185, 7.021016647303503611 ) ) ;
#90993 = CARTESIAN_POINT ( 'NONE',  ( -84.55098283564281303, -24.15543982623907482, -0.2315651400026630391 ) ) ;
#90994 = ORIENTED_EDGE ( 'NONE', *, *, #65203, .F. ) ;
#90995 = FACE_OUTER_BOUND ( 'NONE', #66182, .T. ) ;
#90996 = CARTESIAN_POINT ( 'NONE',  ( -35.52137790958372676, -24.92592662359560407, 8.075495903017991139 ) ) ;
#90997 = CARTESIAN_POINT ( 'NONE',  ( -5.628781154649386664, 20.11113626451368219, -1.500000000000002220 ) ) ;
#90998 = ORIENTED_EDGE ( 'NONE', *, *, #79217, .F. ) ;
#91000 = ORIENTED_EDGE ( 'NONE', *, *, #13555, .F. ) ;
#90999 = CARTESIAN_POINT ( 'NONE',  ( -86.50456855957719426, -24.51314013834314665, 0.6176544820404149538 ) ) ;
#91001 = VERTEX_POINT ( 'NONE', #43322 ) ;
#91002 = AXIS2_PLACEMENT_3D ( 'NONE', #85521, #38352, #93626 ) ;
#91003 = DIRECTION ( 'NONE',  ( 0.000000000000000000, 0.9999999999976377785, 2.173523156925979128E-06 ) ) ;
#91004 = CARTESIAN_POINT ( 'NONE',  ( -19.14942259116913092, -8.910193081567555851, -1.500000000000002220 ) ) ;
#91005 = EDGE_LOOP ( 'NONE', ( #95345, #48209, #82029, #9034 ) ) ;
#91006 = CARTESIAN_POINT ( 'NONE',  ( -4.141025641025638748, -6.376774720514427841, 21.75000000000000355 ) ) ;
#91007 = LINE ( 'NONE', #61075, #6069 ) ;
#91008 = CARTESIAN_POINT ( 'NONE',  ( 20.45693200876408469, 7.529271608661172621, 11.49999999999998934 ) ) ;
#91009 = DIRECTION ( 'NONE',  ( -3.773278334453079618E-23, 0.9999999999976377785, 2.173523156925979975E-06 ) ) ;
#91010 = CARTESIAN_POINT ( 'NONE',  ( -29.49875734969025842, 0.3587747205144265483, 25.61802280011862720 ) ) ;
#91011 = DIRECTION ( 'NONE',  ( -4.448048651795319837E-16, -1.000000000000000000, -7.118365844322522408E-16 ) ) ;
#91012 = CARTESIAN_POINT ( 'NONE',  ( 2.995010171738120786, 21.53247193037183038, -1.500000000000002220 ) ) ;
#91013 = CARTESIAN_POINT ( 'NONE',  ( -71.56719770743626441, -25.24674200897194254, 5.535760866200059027 ) ) ;
#91014 = EDGE_CURVE ( 'NONE', #77171, #69183, #90338, .T. ) ;
#91016 = ORIENTED_EDGE ( 'NONE', *, *, #34618, .F. ) ;
#91015 = CARTESIAN_POINT ( 'NONE',  ( 3.885606641962014329, -21.97303888676646721, 11.49999999999999645 ) ) ;
#91017 = CARTESIAN_POINT ( 'NONE',  ( -27.15721599100127648, -5.965225279485572685, -10.22292133548836546 ) ) ;
#91018 = DIRECTION ( 'NONE',  ( 0.000000000000000000, 0.000000000000000000, -1.000000000000000000 ) ) ;
#91019 = LINE ( 'NONE', #13387, #78024 ) ;
#91020 = ORIENTED_EDGE ( 'NONE', *, *, #34440, .T. ) ;
#91021 = ORIENTED_EDGE ( 'NONE', *, *, #313, .F. ) ;
#91022 = EDGE_LOOP ( 'NONE', ( #59901, #41324, #90156, #34356, #79286, #76207, #20099, #40790 ) ) ;
#91023 = EDGE_CURVE ( 'NONE', #63208, #24140, #77725, .T. ) ;
#91024 = B_SPLINE_CURVE_WITH_KNOTS ( 'NONE', 3,
 ( #10132, #94366, #24853, #55827 ),
 .UNSPECIFIED., .F., .F.,
 ( 4, 4 ),
 ( 2.775557561562891351E-17, 0.0001000000000000167286 ),
 .UNSPECIFIED. ) ;
#91025 = FACE_OUTER_BOUND ( 'NONE', #55789, .T. ) ;
#91026 = AXIS2_PLACEMENT_3D ( 'NONE', #65270, #89574, #74346 ) ;
#91027 = CARTESIAN_POINT ( 'NONE',  ( -49.74369414166532266, -25.30543060587212167, 4.940877950953177944 ) ) ;
#91028 = ADVANCED_FACE ( 'NONE', ( #1131 ), #12906, .T. ) ;
#91029 = CARTESIAN_POINT ( 'NONE',  ( 30.59070867143730155, -4.540774708561928108, 26.30292506078689385 ) ) ;
#91030 = CARTESIAN_POINT ( 'NONE',  ( -43.62287095715005592, -23.72773821059535848, 11.05748984161097503 ) ) ;
#91031 = CARTESIAN_POINT ( 'NONE',  ( -5.798782886354239885, 18.49141925852020663, -1.500000000000002220 ) ) ;
#91032 = CARTESIAN_POINT ( 'NONE',  ( -46.52287095715006160, -23.47596703998600631, 11.44779298504229104 ) ) ;
#91033 = EDGE_LOOP ( 'NONE', ( #61952, #68281, #88851, #8789 ) ) ;
#91034 = CARTESIAN_POINT ( 'NONE',  ( 5.650214204171827070, -18.61605495904187535, 11.49999999999999645 ) ) ;
#91035 = LINE ( 'NONE', #36758, #95767 ) ;
#91036 = EDGE_CURVE ( 'NONE', #83384, #90167, #70135, .T. ) ;
#91037 = ORIENTED_EDGE ( 'NONE', *, *, #2219, .T. ) ;
#91038 = DIRECTION ( 'NONE',  ( -0.6599726524652352877, 0.000000000000000000, 0.7512896232465892110 ) ) ;
#91039 = CARTESIAN_POINT ( 'NONE',  ( 0.1645010273463769490, -1.417169167140626129, -0.3687607960183705291 ) ) ;
#91040 = CARTESIAN_POINT ( 'NONE',  ( -102.6228709571500843, -23.73907113216990794, -1.053371485793225482 ) ) ;
#91041 = DIRECTION ( 'NONE',  ( 0.000000000000000000, 0.000000000000000000, -1.000000000000000000 ) ) ;
#91042 = B_SPLINE_CURVE_WITH_KNOTS ( 'NONE', 3,
 ( #40867, #3820, #17528, #88548, #18525, #27147, #19024, #2320 ),
 .UNSPECIFIED., .F., .F.,
 ( 4, 2, 2, 4 ),
 ( 6.384118678612070021E-06, 0.002007151183507257120, 0.003007534715921578172, 0.004007918248335898791 ),
 .UNSPECIFIED. ) ;
#91043 = AXIS2_PLACEMENT_3D ( 'NONE', #20292, #51768, #98920 ) ;
#91044 = CARTESIAN_POINT ( 'NONE',  ( 16.84789977498956404, 10.09486508543780481, 11.49999999999998934 ) ) ;
#91045 = CARTESIAN_POINT ( 'NONE',  ( -81.62287095715005592, -29.50250243563736774, 8.947779886222141599 ) ) ;
#91047 = ORIENTED_EDGE ( 'NONE', *, *, #54772, .F. ) ;
#91046 = CC_DESIGN_APPROVAL ( #7222, ( #70488 ) ) ;
#91048 = CARTESIAN_POINT ( 'NONE',  ( 18.51311748589099082, 11.02308708543723270, 11.49999999999998934 ) ) ;
#91049 = DIRECTION ( 'NONE',  ( 0.1489078231574191002, 6.845827386180410961E-16, -0.9888510809027407644 ) ) ;
#91050 = DIRECTION ( 'NONE',  ( -0.000000000000000000, -1.000000000000000000, -0.000000000000000000 ) ) ;
#91051 = LINE ( 'NONE', #11934, #86490 ) ;
#91052 = CARTESIAN_POINT ( 'NONE',  ( -100.3381132846150052, -25.27473222076016768, 3.296131264066584077 ) ) ;
#91053 = CARTESIAN_POINT ( 'NONE',  ( 22.92345266703080142, -2.467471440992916154, -1.500000000000002220 ) ) ;
#91054 = APPROVAL_DATE_TIME ( #73839, #5419 ) ;
#91055 = DIRECTION ( 'NONE',  ( 1.000000000000000000, -0.000000000000000000, 0.000000000000000000 ) ) ;
#91056 = CARTESIAN_POINT ( 'NONE',  ( -49.53129519467806574, -24.65952944569304606, 1.056160979905696129 ) ) ;
#91057 = CARTESIAN_POINT ( 'NONE',  ( 7.141438900065890216, -18.84860497471923679, 11.49999999999999645 ) ) ;
#91058 = CARTESIAN_POINT ( 'NONE',  ( -45.62287095715004881, -24.91570333823099759, 8.075032458375549282 ) ) ;
#91059 = LINE ( 'NONE', #12929, #72629 ) ;
#91060 = CARTESIAN_POINT ( 'NONE',  ( -4.194375271223358403, -5.876774720514417183, 20.09898898868106087 ) ) ;
#91061 = DIRECTION ( 'NONE',  ( 0.000000000000000000, 2.173523156925980399E-06, -0.9999999999976378895 ) ) ;
#91062 = CARTESIAN_POINT ( 'NONE',  ( -110.8177083405623478, -25.29779178145291496, 3.398758112327336267 ) ) ;
#91063 = EDGE_CURVE ( 'NONE', #3935, #87407, #27454, .T. ) ;
#91064 = CARTESIAN_POINT ( 'NONE',  ( 19.48829924427396421, 3.997931079995220127, -1.500000000000002220 ) ) ;
#91065 = CARTESIAN_POINT ( 'NONE',  ( -113.5177925269431256, -24.15543982623907482, -0.2315651400026574047 ) ) ;
#91066 = CARTESIAN_POINT ( 'NONE',  ( 9.261118129494249729, -17.44851725036260248, -1.500000000000002220 ) ) ;
#91067 = DIRECTION ( 'NONE',  ( -0.000000000000000000, 1.000000000000000000, -0.000000000000000000 ) ) ;
#91068 = ADVANCED_FACE ( 'NONE', ( #62034 ), #100406, .T. ) ;
#91069 = CARTESIAN_POINT ( 'NONE',  ( -38.62287095715005592, -23.48786465467240703, 11.44779295918255180 ) ) ;
#91070 = CARTESIAN_POINT ( 'NONE',  ( -1.318699232124953324, -6.376774720514411854, 19.74039977944280722 ) ) ;
#91071 = CARTESIAN_POINT ( 'NONE',  ( -20.66316395829706209, -0.6310838753663271516, 11.49999999999999645 ) ) ;
#91072 = CARTESIAN_POINT ( 'NONE',  ( -111.6228709571500559, -24.64965695001468404, 8.947790433994176951 ) ) ;
#91073 = CARTESIAN_POINT ( 'NONE',  ( 31.51256023177338861, 4.716437395117331732, -1.484035900832843868 ) ) ;
#91074 = LINE ( 'NONE', #76336, #68435 ) ;
#91076 = EDGE_CURVE ( 'NONE', #17028, #86907, #80641, .T. ) ;
#91075 = CARTESIAN_POINT ( 'NONE',  ( 4.020035926878589905, 22.33396232419688587, 11.49999999999999645 ) ) ;
#91077 = ORIENTED_EDGE ( 'NONE', *, *, #65661, .T. ) ;
#91078 = B_SPLINE_SURFACE_WITH_KNOTS ( 'NONE', 3, 3, ( 
 ( #21567, #68267, #49311, #26466 ),
 ( #25452, #87348, #95463, #17848 ),
 ( #73140, #25954, #48809, #10735 ),
 ( #11231, #18345, #94963, #33572 ),
 ( #64550, #88359, #56426, #42208 ),
 ( #80748, #80242, #79734, #41189 ),
 ( #56926, #87857, #41700, #72643 ) ),
 .UNSPECIFIED., .F., .F., .F.,
 ( 4, 3, 4 ),
 ( 4, 4 ),
 ( 0.7945040050992232539, 0.8970133687736492334, 0.9995227324480751019 ),
 ( 0.02950149398476096044, 0.03052783838704493588 ),
 .UNSPECIFIED. ) ;
#91079 = CARTESIAN_POINT ( 'NONE',  ( -60.62287095715004881, -23.48783264082478439, -1.443836473390068820 ) ) ;
#91080 = CARTESIAN_POINT ( 'NONE',  ( 30.61138385796263606, 5.156104205939422869, 27.19700247792284031 ) ) ;
#91081 = CARTESIAN_POINT ( 'NONE',  ( -4.116507902937485142, 19.75820112358731251, -1.500000000000002220 ) ) ;
#91082 = CARTESIAN_POINT ( 'NONE',  ( 8.567893164715611576, -0.1262136116457373280, -3.707288619710387145 ) ) ;
#91083 = DIRECTION ( 'NONE',  ( 0.000000000000000000, -1.000000000000000000, 0.000000000000000000 ) ) ;
#91084 = ORIENTED_EDGE ( 'NONE', *, *, #43371, .F. ) ;
#91085 = EDGE_LOOP ( 'NONE', ( #13249, #60341, #42099, #58254, #304 ) ) ;
#91086 = DIRECTION ( 'NONE',  ( -1.000000000000000000, -0.000000000000000000, -0.000000000000000000 ) ) ;
#91087 = CARTESIAN_POINT ( 'NONE',  ( 11.15996004898972771, 19.99216496293481882, -1.500000000000002220 ) ) ;
#91088 = DIRECTION ( 'NONE',  ( -1.000000000000000000, 0.000000000000000000, -0.000000000000000000 ) ) ;
#91089 = CARTESIAN_POINT ( 'NONE',  ( -8.750087785235610482, 19.73178376063210138, -1.500000000000002220 ) ) ;
#91090 = CARTESIAN_POINT ( 'NONE',  ( -123.5900408317157400, -24.15543982623907482, -0.2315651400026560169 ) ) ;
#91091 = DIRECTION ( 'NONE',  ( -3.773278334453079618E-23, 0.9999999999976377785, 2.173523156925978705E-06 ) ) ;
#91092 = CARTESIAN_POINT ( 'NONE',  ( 19.01167203989450982, 12.12494712425435850, 11.49999999999999645 ) ) ;
#91093 = ORIENTED_EDGE ( 'NONE', *, *, #93681, .F. ) ;
#91094 = CARTESIAN_POINT ( 'NONE',  ( -86.92287095715005307, -23.47593901973090169, -1.443836447538996870 ) ) ;
#91095 = VECTOR ( 'NONE', #52385, 1000.000000000000000 ) ;
#91096 = CARTESIAN_POINT ( 'NONE',  ( 16.65356921002588919, 14.36988287374134821, 11.49999999999998934 ) ) ;
#91097 = B_SPLINE_CURVE_WITH_KNOTS ( 'NONE', 3,
 ( #55474, #39732, #17402, #80302, #41246, #48362 ),
 .UNSPECIFIED., .F., .F.,
 ( 4, 2, 4 ),
 ( 1.570755371633915156E-05, 0.001396183895866087753, 0.002776660238015836446 ),
 .UNSPECIFIED. ) ;
#91098 = EDGE_CURVE ( 'NONE', #45069, #90256, #42034, .T. ) ;
#91099 = LINE ( 'NONE', #22561, #905 ) ;
#91100 = CARTESIAN_POINT ( 'NONE',  ( -28.09930172958063466, -25.21724980323388010, 7.540557109994362683 ) ) ;
#91101 = ORIENTED_EDGE ( 'NONE', *, *, #71364, .T. ) ;
#91102 = CARTESIAN_POINT ( 'NONE',  ( 4.692776824272364422, -6.376774720514406525, 18.67160386110882442 ) ) ;
#91103 = CARTESIAN_POINT ( 'NONE',  ( -90.62774790572264294, -24.73531770709095312, 8.716586749053512051 ) ) ;
#91104 = VERTEX_POINT ( 'NONE', #26893 ) ;
#91105 = CARTESIAN_POINT ( 'NONE',  ( -72.59671265881189584, -23.96169478059713143, 10.65365249895718414 ) ) ;
#91106 = EDGE_CURVE ( 'NONE', #20975, #64208, #97402, .T. ) ;
#91107 = VERTEX_POINT ( 'NONE', #51231 ) ;
#91108 = VERTEX_POINT ( 'NONE', #18282 ) ;
#91109 = CARTESIAN_POINT ( 'NONE',  ( -49.31882137186372717, -25.28401378673735067, 5.880832581787514890 ) ) ;
#91110 = PLANE ( 'NONE',  #3268 ) ;
#91111 = CARTESIAN_POINT ( 'NONE',  ( -57.55356396053624479, -23.96119346886880663, -0.6495511937832122440 ) ) ;
#91112 = CARTESIAN_POINT ( 'NONE',  ( -15.93830457579706739, -12.76012858937699335, -1.500000000000002220 ) ) ;
#91113 = ORIENTED_EDGE ( 'NONE', *, *, #16259, .T. ) ;
#91114 = CARTESIAN_POINT ( 'NONE',  ( -0.6227173540047638012, -5.876774720514413630, 19.48351902941045211 ) ) ;
#91115 = EDGE_CURVE ( 'NONE', #4424, #24841, #79227, .T. ) ;
#91116 = CARTESIAN_POINT ( 'NONE',  ( -99.52287095715001897, -24.51387760970726504, 9.387446482453416507 ) ) ;
#91117 = EDGE_CURVE ( 'NONE', #33243, #56669, #10553, .T. ) ;
#91119 = CARTESIAN_POINT ( 'NONE',  ( -4.968349358974361252, -6.376774720514411854, 19.46153846153847056 ) ) ;
#91118 = VECTOR ( 'NONE', #60968, 1000.000000000000114 ) ;
#91120 = DIRECTION ( 'NONE',  ( 0.000000000000000000, -2.173523156925979552E-06, 0.9999999999976378895 ) ) ;
#91121 = ORIENTED_EDGE ( 'NONE', *, *, #52108, .T. ) ;
#91122 = DIRECTION ( 'NONE',  ( -0.9822594791677485837, 0.000000000000000000, 0.1875268396392986980 ) ) ;
#91123 = CARTESIAN_POINT ( 'NONE',  ( -28.90723246652128609, -25.26247981585383684, 7.813648767477532786 ) ) ;
#91124 = LOCAL_TIME ( 0, 54, 15.00000000000000000, #30528 ) ;
#91125 = CARTESIAN_POINT ( 'NONE',  ( -2.100290975465340271, -20.70549805216813510, -1.500000000000002220 ) ) ;
#91126 = ORIENTED_EDGE ( 'NONE', *, *, #5787, .F. ) ;
#91128 = ORIENTED_EDGE ( 'NONE', *, *, #66468, .F. ) ;
#91127 = CARTESIAN_POINT ( 'NONE',  ( 4.572862496014544753, -6.376774720514408301, 19.20224321281611068 ) ) ;
#91129 = CARTESIAN_POINT ( 'NONE',  ( 30.53060340732035982, -4.594240983522013266, 19.84760796525321425 ) ) ;
#91130 = ORIENTED_EDGE ( 'NONE', *, *, #51205, .T. ) ;
#91131 = VERTEX_POINT ( 'NONE', #2567 ) ;
#91132 = CARTESIAN_POINT ( 'NONE',  ( -120.6228709571500417, -23.47593901973091235, -1.443836447538997536 ) ) ;
#91133 = CARTESIAN_POINT ( 'NONE',  ( -11.16000000000000014, -10.15233964170348457, 0.003711184059992174607 ) ) ;
#91134 = AXIS2_PLACEMENT_3D ( 'NONE', #20485, #97615, #65702 ) ;
#91135 = CARTESIAN_POINT ( 'NONE',  ( -60.58953762381672448, -23.48786465467241058, 11.44779295918254824 ) ) ;
#91136 = DIRECTION ( 'NONE',  ( -3.773278334453079030E-23, 0.9999999999976377785, 2.173523156925979128E-06 ) ) ;
#91137 = ADVANCED_FACE ( 'NONE', ( #57865 ), #66348, .T. ) ;
#91139 = ORIENTED_EDGE ( 'NONE', *, *, #862, .F. ) ;
#91138 = CARTESIAN_POINT ( 'NONE',  ( 0.7503028313155074569, 22.12739137992853955, 11.49999999999999645 ) ) ;
#91140 = CARTESIAN_POINT ( 'NONE',  ( -72.62287095715005592, -24.65952944569304606, 1.056160979905698794 ) ) ;
#91141 = CARTESIAN_POINT ( 'NONE',  ( 21.95517018727266390, 5.574673621280945568, -1.500000000000002220 ) ) ;
#91143 = ORIENTED_EDGE ( 'NONE', *, *, #547, .F. ) ;
#91142 = CARTESIAN_POINT ( 'NONE',  ( -92.52287095715011844, -23.96127896942171276, -0.6493128930931688636 ) ) ;
#91144 = ORIENTED_EDGE ( 'NONE', *, *, #44533, .F. ) ;
#91145 = CARTESIAN_POINT ( 'NONE',  ( -10.18932761084327865, -5.341047792237469949, 29.75743496038930758 ) ) ;
#91146 = EDGE_CURVE ( 'NONE', #74381, #26531, #91287, .T. ) ;
#91147 = AXIS2_PLACEMENT_3D ( 'NONE', #48760, #95417, #32013 ) ;
#91148 = CARTESIAN_POINT ( 'NONE',  ( -18.22032804147677254, 8.545885342870345625, -1.500000000000002220 ) ) ;
#91149 = EDGE_CURVE ( 'NONE', #26606, #82230, #28889, .T. ) ;
#91150 = CARTESIAN_POINT ( 'NONE',  ( 32.66876533700883556, 5.965225279485572685, -12.58926540598386445 ) ) ;
#91151 = VERTEX_POINT ( 'NONE', #44618 ) ;
#91152 = CARTESIAN_POINT ( 'NONE',  ( -22.05275734969026047, -5.965225279485572685, 31.02402280011862246 ) ) ;
#91153 = CARTESIAN_POINT ( 'NONE',  ( -6.278373996654322831, -21.41630973362384083, -1.500000000000002220 ) ) ;
#91154 = EDGE_CURVE ( 'NONE', #67264, #76612, #35887, .T. ) ;
#91155 = ORIENTED_EDGE ( 'NONE', *, *, #11007, .T. ) ;
#91156 = ORIENTED_EDGE ( 'NONE', *, *, #36061, .T. ) ;
#91157 = CARTESIAN_POINT ( 'NONE',  ( 24.50000000000000000, -0.9000000000000000222, 1.103411337323757735 ) ) ;
#91158 = DIRECTION ( 'NONE',  ( 0.000000000000000000, 0.9999999999976377785, 2.173523156925979128E-06 ) ) ;
#91159 = FACE_OUTER_BOUND ( 'NONE', #41111, .T. ) ;
#91160 = CARTESIAN_POINT ( 'NONE',  ( -96.62287095715005592, -24.66019654487199730, 8.947790411086124607 ) ) ;
#91161 = ADVANCED_FACE ( 'NONE', ( #6049 ), #59853, .T. ) ;
#91162 = CARTESIAN_POINT ( 'NONE',  ( -44.22287095715005023, -23.47596703998600276, 11.44779298504227860 ) ) ;
#91163 = EDGE_CURVE ( 'NONE', #17845, #65436, #72202, .T. ) ;
#91164 = CARTESIAN_POINT ( 'NONE',  ( 14.28107258077893604, -13.35224110012613963, 11.49999999999998934 ) ) ;
#91165 = AXIS2_PLACEMENT_3D ( 'NONE', #34664, #10318, #27554 ) ;
#91166 = DIRECTION ( 'NONE',  ( 1.000000000000000000, -4.015954566446630556E-15, 0.000000000000000000 ) ) ;
#91167 = CARTESIAN_POINT ( 'NONE',  ( -14.42888051209446409, 15.91495273949476363, 11.49999999999998934 ) ) ;
#91168 = CARTESIAN_POINT ( 'NONE',  ( -25.89225704477708589, -24.92774936967245125, 2.873802147424679987 ) ) ;
#91169 = LINE ( 'NONE', #52613, #40588 ) ;
#91170 = LINE ( 'NONE', #90673, #2272 ) ;
#91171 = CARTESIAN_POINT ( 'NONE',  ( -13.85039312988123150, 18.09399583546626289, -1.500000000000002220 ) ) ;
#91172 = CARTESIAN_POINT ( 'NONE',  ( -96.54970709809541063, -24.35071581493543391, 9.817618358456023486 ) ) ;
#91173 = CARTESIAN_POINT ( 'NONE',  ( -91.62287095715004170, -29.50250786944525672, 11.44777988621623344 ) ) ;
#91174 = CARTESIAN_POINT ( 'NONE',  ( 19.59856454566043382, -3.714209461170434157, 11.49999999999999645 ) ) ;
#91175 = CARTESIAN_POINT ( 'NONE',  ( -59.62287095715004881, -29.50248528299804818, 1.056150453629034924 ) ) ;
#91176 = CARTESIAN_POINT ( 'NONE',  ( 21.57151214508649772, 3.625915217019311583E-15, 0.000000000000000000 ) ) ;
#91177 = CARTESIAN_POINT ( 'NONE',  ( 8.499999999999989342, 18.74999999999999645, 0.000000000000000000 ) ) ;
#91178 = ORIENTED_EDGE ( 'NONE', *, *, #24101, .F. ) ;
#91179 = DIRECTION ( 'NONE',  ( 3.773278334444166432E-23, -1.000000000000000000, 0.000000000000000000 ) ) ;
#91180 = DIRECTION ( 'NONE',  ( -0.000000000000000000, 1.000000000000000000, -0.000000000000000000 ) ) ;
#91181 = CARTESIAN_POINT ( 'NONE',  ( -19.66401359581072583, -9.230316601043258018, 11.49999999999998934 ) ) ;
#91182 = FACE_OUTER_BOUND ( 'NONE', #89738, .T. ) ;
#91183 = CARTESIAN_POINT ( 'NONE',  ( 14.99095386781537975, 12.61000069877385421, -1.500000000000002220 ) ) ;
#91184 = CARTESIAN_POINT ( 'NONE',  ( -80.62287095715005592, -24.99156045073393173, 7.747789690856161648 ) ) ;
#91185 = AXIS2_PLACEMENT_3D ( 'NONE', #45385, #61613, #75805 ) ;
#91186 = ORIENTED_EDGE ( 'NONE', *, *, #98501, .T. ) ;
#91187 = APPROVAL_ROLE ( '' ) ;
#91188 = PRODUCT_DEFINITION_FORMATION_WITH_SPECIFIED_SOURCE ( 'ANY', '', #51515, .NOT_KNOWN. ) ;
#91189 = CARTESIAN_POINT ( 'NONE',  ( 9.843544857143434967, -6.475225279485573360, -27.49819965379373343 ) ) ;
#91190 = CARTESIAN_POINT ( 'NONE',  ( -54.62287095715005592, -29.50248528299804818, 1.056150453629033370 ) ) ;
#91191 = CARTESIAN_POINT ( 'NONE',  ( 20.32696876622996029, 2.630761579057304900, 11.49999999999999645 ) ) ;
#91192 = CARTESIAN_POINT ( 'NONE',  ( -39.06125964696975217, -25.30336593734606510, 4.454089851809797551 ) ) ;
#91193 = B_SPLINE_CURVE_WITH_KNOTS ( 'NONE', 3,
 ( #68187, #84896, #76277, #14379, #30108, #45355, #61081, #92010, #61585, #78769, #39719, #9269, #16380, #40234, #55464 ),
 .UNSPECIFIED., .F., .F.,
 ( 4, 1, 1, 1, 1, 1, 1, 1, 1, 1, 1, 1, 4 ),
 ( 0.000000000000000000, 0.08415201884431637580, 0.1665323202984579920, 0.2488363311465297822, 0.3312461454872601685, 0.4129571090216147544, 0.4904942776695643825, 0.5661557919819225626, 0.6399873346864677348, 0.7167654882718510478, 0.8021439047100968889, 0.8958332007101900141, 1.000000000000000000 ),
 .UNSPECIFIED. ) ;
#91194 = CARTESIAN_POINT ( 'NONE',  ( -93.62287095715004170, -23.48783264082478794, -1.443836473390063713 ) ) ;
#91195 = CIRCLE ( 'NONE', #97717, 253.2618649670780826 ) ;
#91196 = VERTEX_POINT ( 'NONE', #45128 ) ;
#91197 = DIRECTION ( 'NONE',  ( 1.000000000000000000, -0.000000000000000000, -0.000000000000000000 ) ) ;
#91198 = DIRECTION ( 'NONE',  ( 1.000000000000000000, 3.773278334444167608E-23, 8.201307833595939069E-29 ) ) ;
#91199 = DIRECTION ( 'NONE',  ( 0.000000000000000000, 0.000000000000000000, 1.000000000000000000 ) ) ;
#91200 = AXIS2_PLACEMENT_3D ( 'NONE', #8516, #78004, #30850 ) ;
#91201 = DIRECTION ( 'NONE',  ( -3.773278334453080206E-23, 0.9999999999976377785, 2.173523156925979975E-06 ) ) ;
#91202 = ORIENTED_EDGE ( 'NONE', *, *, #20328, .T. ) ;
#91203 = CARTESIAN_POINT ( 'NONE',  ( 30.55234109742892912, 6.376774720514427841, 1.942002712049490487 ) ) ;
#91204 = CARTESIAN_POINT ( 'NONE',  ( 21.75825945658488436, -7.631246777643061030, 11.49999999999999645 ) ) ;
#91205 = CARTESIAN_POINT ( 'NONE',  ( -9.359374538088376383, 20.77767741201286711, -1.500000000000002220 ) ) ;
#91206 = CARTESIAN_POINT ( 'NONE',  ( 3.249631081431332280, -6.376774720514424288, 21.24682042713427776 ) ) ;
#91207 = B_SPLINE_SURFACE_WITH_KNOTS ( 'NONE', 3, 3, ( 
 ( #96594, #42829, #79368, #33199 ),
 ( #65185, #33707, #57559, #50432 ),
 ( #9862, #34213, #73760, #27597 ),
 ( #17979, #96109, #89487, #25587 ),
 ( #19966, #48940, #79868, #40812 ),
 ( #2768, #88495, #18971, #66180 ),
 ( #42339, #49949, #64181, #95102 ) ),
 .UNSPECIFIED., .F., .F., .F.,
 ( 4, 3, 4 ),
 ( 4, 4 ),
 ( 0.0004766839783816845776, 0.1029713700210893035, 0.2054660560637969202 ),
 ( 0.5796414481296850996, 0.5809216181848338989 ),
 .UNSPECIFIED. ) ;
#91208 = CARTESIAN_POINT ( 'NONE',  ( -105.6228709571500559, -23.47593901973091235, -1.443836447538999312 ) ) ;
#91209 = CARTESIAN_POINT ( 'NONE',  ( -2.948852648430471124, -14.44618168209107445, 0.000000000000000000 ) ) ;
#91210 = LINE ( 'NONE', #52160, #25246 ) ;
#91211 = DIRECTION ( 'NONE',  ( -0.000000000000000000, -0.000000000000000000, -1.000000000000000000 ) ) ;
#91212 = CARTESIAN_POINT ( 'NONE',  ( 11.25260618158950621, 18.78031238747207610, 11.49999999999998934 ) ) ;
#91213 = DIRECTION ( 'NONE',  ( 0.000000000000000000, -0.9999999999976377785, -2.173523156925979975E-06 ) ) ;
#91214 = ADVANCED_FACE ( 'NONE', ( #82671 ), #14150, .F. ) ;
#91215 = CARTESIAN_POINT ( 'NONE',  ( -50.62287095715007013, -24.52232992886362695, 0.6492154411906128075 ) ) ;
#91216 = CARTESIAN_POINT ( 'NONE',  ( -40.48073109628643351, -25.31533619740083196, 5.080591194951591838 ) ) ;
#91217 = CARTESIAN_POINT ( 'NONE',  ( -78.62361334277453295, -24.65952944569304606, 1.056160979905704789 ) ) ;
#91218 = CARTESIAN_POINT ( 'NONE',  ( -112.6228709571500559, -23.47593901973091235, -1.443836447538999312 ) ) ;
#91219 = CARTESIAN_POINT ( 'NONE',  ( -4.223504350552545361, -5.876774720514412742, 19.52341893546492813 ) ) ;
#91220 = ORIENTED_EDGE ( 'NONE', *, *, #23758, .F. ) ;
#91221 = CARTESIAN_POINT ( 'NONE',  ( -4.302178748239556150, -20.00421716419250373, 11.49999999999998934 ) ) ;
#91222 = ORIENTED_EDGE ( 'NONE', *, *, #75193, .F. ) ;
#91223 = ORIENTED_EDGE ( 'NONE', *, *, #79432, .F. ) ;
#91224 = EDGE_LOOP ( 'NONE', ( #56468, #44682, #12139, #10268 ) ) ;
#91225 = ORIENTED_EDGE ( 'NONE', *, *, #66202, .T. ) ;
#91226 = CARTESIAN_POINT ( 'NONE',  ( -20.34888222059871410, 10.79260868881566715, -1.500000000000002220 ) ) ;
#91227 = CARTESIAN_POINT ( 'NONE',  ( -35.52287095715006870, -24.52232992886611740, 0.6492154411976478467 ) ) ;
#91228 = CARTESIAN_POINT ( 'NONE',  ( -13.42616926349082895, -15.17935092467416069, -1.500000000000002220 ) ) ;
#91229 = CIRCLE ( 'NONE', #34535, 1.399999999999988143 ) ;
#91230 = ORIENTED_EDGE ( 'NONE', *, *, #90904, .T. ) ;
#91231 = EDGE_CURVE ( 'NONE', #100041, #82077, #65040, .T. ) ;
#91232 = CARTESIAN_POINT ( 'NONE',  ( -48.52287095715006160, -23.47596703998600631, 11.44779298504229104 ) ) ;
#91233 = EDGE_CURVE ( 'NONE', #80383, #14468, #21757, .T. ) ;
#91234 = CARTESIAN_POINT ( 'NONE',  ( -28.84663072490566194, -5.965225279485572685, 28.73989617533406715 ) ) ;
#91235 = EDGE_CURVE ( 'NONE', #38539, #64573, #45274, .T. ) ;
#91236 = CARTESIAN_POINT ( 'NONE',  ( -0.02075734969026423599, -5.965225279485572685, -28.54397719988136828 ) ) ;
#91237 = CARTESIAN_POINT ( 'NONE',  ( -70.56769351002753865, -23.48783264082477018, -1.443836473390095021 ) ) ;
#91239 = ORIENTED_EDGE ( 'NONE', *, *, #52797, .F. ) ;
#91238 = CARTESIAN_POINT ( 'NONE',  ( 20.52986552169224410, -6.224258026782483633, 11.49999999999999645 ) ) ;
#91240 = DIRECTION ( 'NONE',  ( 1.000000000000000000, 3.773278334444167608E-23, 8.201307833595939069E-29 ) ) ;
#91242 = CIRCLE ( 'NONE', #11849, 6.119803529381342422 ) ;
#91241 = CARTESIAN_POINT ( 'NONE',  ( 30.09341516180546350, 2.682774720514426559, -11.39311774897855756 ) ) ;
#91243 = EDGE_CURVE ( 'NONE', #90256, #31553, #44342, .T. ) ;
#91244 = ORIENTED_EDGE ( 'NONE', *, *, #17882, .F. ) ;
#91245 = CARTESIAN_POINT ( 'NONE',  ( -19.59449498831206782, -6.737714454370689054, -1.500000000000002220 ) ) ;
#91247 = ORIENTED_EDGE ( 'NONE', *, *, #91905, .T. ) ;
#91246 = DIRECTION ( 'NONE',  ( -0.000000000000000000, 1.000000000000000000, -0.000000000000000000 ) ) ;
#91248 = CARTESIAN_POINT ( 'NONE',  ( -28.51175871785264349, -23.57346878409127200, -1.055554491438110309 ) ) ;
#91249 = ORIENTED_EDGE ( 'NONE', *, *, #89819, .T. ) ;
#91250 = CARTESIAN_POINT ( 'NONE',  ( 4.403244164709623654, -5.876774720514402972, 18.35516266052912826 ) ) ;
#91251 = ORIENTED_EDGE ( 'NONE', *, *, #80510, .T. ) ;
#91252 = CARTESIAN_POINT ( 'NONE',  ( 2.184583272949580213, -20.89682302726931340, -1.500000000000002220 ) ) ;
#91253 = ADVANCED_FACE ( 'NONE', ( #83667 ), #6553, .F. ) ;
#91254 = CARTESIAN_POINT ( 'NONE',  ( 11.39931579351042679, 18.75040340349860557, 11.49999999999999645 ) ) ;
#91255 = DIRECTION ( 'NONE',  ( 0.000000000000000000, -0.000000000000000000, -1.000000000000000000 ) ) ;
#91256 = CARTESIAN_POINT ( 'NONE',  ( 18.83488669200175281, -12.41447709603701632, -1.500000000000002220 ) ) ;
#91257 = CARTESIAN_POINT ( 'NONE',  ( -12.80012119340476140, -16.60591428456014640, 11.49999999999998934 ) ) ;
#91258 = CARTESIAN_POINT ( 'NONE',  ( -89.62287095715004170, -24.64898659630529210, 1.056161002820827921 ) ) ;
#91259 = DIRECTION ( 'NONE',  ( -1.000000000000000000, -0.000000000000000000, -0.000000000000000000 ) ) ;
#91260 = AXIS2_PLACEMENT_3D ( 'NONE', #74109, #88336, #72617 ) ;
#91261 = CARTESIAN_POINT ( 'NONE',  ( -53.55620429048339304, -23.48786465467240347, 11.44779295918255002 ) ) ;
#91263 = ADVANCED_FACE ( 'NONE', ( #36496 ), #22254, .T. ) ;
#91262 = ORIENTED_EDGE ( 'NONE', *, *, #71322, .F. ) ;
#91264 = B_SPLINE_CURVE_WITH_KNOTS ( 'NONE', 3,
 ( #83661, #99868, #30375, #44612 ),
 .UNSPECIFIED., .F., .F.,
 ( 4, 4 ),
 ( 1.301246609561020917E-05, 0.002190852597862436284 ),
 .UNSPECIFIED. ) ;
#91265 = SECURITY_CLASSIFICATION ( '', '', #92184 ) ;
#91266 = EDGE_LOOP ( 'NONE', ( #14746, #93119, #8493, #6914 ) ) ;
#91267 = EDGE_LOOP ( 'NONE', ( #71498, #38336, #91976, #45110 ) ) ;
#91268 = DIRECTION ( 'NONE',  ( 1.000000000000000000, 0.000000000000000000, 0.000000000000000000 ) ) ;
#91269 = EDGE_CURVE ( 'NONE', #14852, #47263, #21311, .T. ) ;
#91270 = CARTESIAN_POINT ( 'NONE',  ( 15.57385778016992894, -14.83193121981731544, -1.500000000000002220 ) ) ;
#91271 = VECTOR ( 'NONE', #67754, 1000.000000000000000 ) ;
#91272 = CARTESIAN_POINT ( 'NONE',  ( 14.82775695341588573, 5.152774720514427642, -26.90408793620859385 ) ) ;
#91273 = ORIENTED_EDGE ( 'NONE', *, *, #75245, .T. ) ;
#91274 = CARTESIAN_POINT ( 'NONE',  ( 11.07546443054301655, -17.96822238807187233, -1.500000000000002220 ) ) ;
#91275 = CARTESIAN_POINT ( 'NONE',  ( -81.52287095715006160, -29.50247984919015209, -1.443849546365053582 ) ) ;
#91276 = CARTESIAN_POINT ( 'NONE',  ( -64.49572739054461579, -24.51314013834315730, 0.6176544820404094027 ) ) ;
#91277 = CARTESIAN_POINT ( 'NONE',  ( -49.62287095715005592, -23.48783264082478084, -1.443836473390070596 ) ) ;
#91278 = CARTESIAN_POINT ( 'NONE',  ( 2.100208336950355914, 0.000000000000000000, 0.000000000000000000 ) ) ;
#91279 = PLANE ( 'NONE',  #43834 ) ;
#91280 = CARTESIAN_POINT ( 'NONE',  ( -19.76278938440450617, -9.944092408650034187, -1.500000000000002220 ) ) ;
#91281 = AXIS2_PLACEMENT_3D ( 'NONE', #32125, #678, #63098 ) ;
#91282 = CARTESIAN_POINT ( 'NONE',  ( -81.54381818738237087, -24.51419770103159834, 9.386484678747182286 ) ) ;
#91283 = ADVANCED_FACE ( 'NONE', ( #9047 ), #50937, .T. ) ;
#91284 = VERTEX_POINT ( 'NONE', #39505 ) ;
#91285 = CARTESIAN_POINT ( 'NONE',  ( -2.959136224476847765, -6.376774720514413630, 19.53857357749110335 ) ) ;
#91286 = CARTESIAN_POINT ( 'NONE',  ( 12.67628326092776803, 4.091305608280291217, -27.97525530010125294 ) ) ;
#91287 = LINE ( 'NONE', #98385, #80909 ) ;
#91288 = EDGE_CURVE ( 'NONE', #12640, #25116, #57651, .T. ) ;
#91289 = CARTESIAN_POINT ( 'NONE',  ( -97.52287095715009002, -23.72773821059536914, 11.05748984161097503 ) ) ;
#91290 = CARTESIAN_POINT ( 'NONE',  ( 9.746180923669104601, -16.83516941858706417, -1.500000000000002220 ) ) ;
#91291 = CARTESIAN_POINT ( 'NONE',  ( -18.12654925440673637, -11.31956730046968751, -1.500000000000002220 ) ) ;
#91292 = CARTESIAN_POINT ( 'NONE',  ( -113.6228709571500559, -23.48786465467241769, 11.44779295918254114 ) ) ;
#91293 = CARTESIAN_POINT ( 'NONE',  ( -81.52287095715006160, -23.48786465467241058, 11.44779295918254469 ) ) ;
#91294 = CARTESIAN_POINT ( 'NONE',  ( -72.52287095715011844, -24.33927499327855770, 9.819080762295822495 ) ) ;
#91295 = CARTESIAN_POINT ( 'NONE',  ( -36.62287095715005592, -24.66019654487199020, 8.947790411086138818 ) ) ;
#91296 = CARTESIAN_POINT ( 'NONE',  ( -13.31036990564671818, -18.29084955798148471, -1.500000000000002220 ) ) ;
#91297 = B_SPLINE_SURFACE_WITH_KNOTS ( 'NONE', 3, 3, ( 
 ( #45892, #92052, #21038, #29158 ),
 ( #60132, #6814, #37278, #5322 ),
 ( #68727, #61123, #52507, #59129 ),
 ( #68229, #99158, #52007, #82937 ) ),
 .UNSPECIFIED., .F., .F., .F.,
 ( 4, 4 ),
 ( 4, 4 ),
 ( 0.3744551372274605994, 0.4812677536984230064 ),
 ( 0.7926673770166410282, 0.8107671855866930288 ),
 .UNSPECIFIED. ) ;
#91298 = ORIENTED_EDGE ( 'NONE', *, *, #50155, .F. ) ;
#91299 = CARTESIAN_POINT ( 'NONE',  ( -80.96226385320382235, -29.50248939449842922, 2.947779886236309377 ) ) ;
#91300 = CARTESIAN_POINT ( 'NONE',  ( -89.49044894935767047, -29.50248914370730091, 2.832395270851967073 ) ) ;
#91301 = CARTESIAN_POINT ( 'NONE',  ( -16.86558833231006460, 10.32443627698238409, 11.49999999999999645 ) ) ;
#91302 = CARTESIAN_POINT ( 'NONE',  ( -91.62287095715004170, -23.47593901973091235, -1.443836447539002865 ) ) ;
#91303 = ORIENTED_EDGE ( 'NONE', *, *, #89874, .F. ) ;
#91304 = DIRECTION ( 'NONE',  ( -3.773278334453079030E-23, 0.9999999999976377785, 2.173523156925979128E-06 ) ) ;
#91305 = AXIS2_PLACEMENT_3D ( 'NONE', #61829, #88039, #57599 ) ;
#91306 = CARTESIAN_POINT ( 'NONE',  ( 27.53860345374808105, 1.477225279485574028, 19.84760796525321425 ) ) ;
#91307 = CARTESIAN_POINT ( 'NONE',  ( 7.043455336710909620, -20.48365140995157674, 11.49999999999998934 ) ) ;
#91308 = CARTESIAN_POINT ( 'NONE',  ( -49.47157371846719087, -25.10935202069072858, 3.177618851823707402 ) ) ;
#91309 = CARTESIAN_POINT ( 'NONE',  ( 19.04819733361787470, -3.913502273677552878, -1.500000000000002220 ) ) ;
#91310 = DIRECTION ( 'NONE',  ( 1.000000000000000000, 0.000000000000000000, 0.000000000000000000 ) ) ;
#91311 = DIRECTION ( 'NONE',  ( -1.387778780781445429E-16, 1.000000000000000000, 0.000000000000000000 ) ) ;
#91312 = CARTESIAN_POINT ( 'NONE',  ( 18.78060722631472501, -6.265068672152646734, -1.500000000000002220 ) ) ;
#91313 = ORIENTED_EDGE ( 'NONE', *, *, #87456, .F. ) ;
#91314 = AXIS2_PLACEMENT_3D ( 'NONE', #82982, #99205, #69771 ) ;
#91315 = CARTESIAN_POINT ( 'NONE',  ( -20.26613141553852060, -1.498020344548873561, 11.49999999999999645 ) ) ;
#91316 = DIRECTION ( 'NONE',  ( 6.220620959342031946E-15, 0.000000000000000000, -1.000000000000000000 ) ) ;
#91317 = CARTESIAN_POINT ( 'NONE',  ( 33.64270623324222953, -3.650451339955370855, -11.69061897474703571 ) ) ;
#91318 = ORIENTED_EDGE ( 'NONE', *, *, #100404, .T. ) ;
#91319 = CARTESIAN_POINT ( 'NONE',  ( -102.6290224326610172, -24.15620529776628445, 10.23563542870660292 ) ) ;
#91320 = CARTESIAN_POINT ( 'NONE',  ( -116.4728709594060092, -25.40676080801055647, 8.000950338065035083 ) ) ;
#91321 = FACE_OUTER_BOUND ( 'NONE', #69278, .T. ) ;
#91322 = DIRECTION ( 'NONE',  ( -0.000000000000000000, 1.000000000000000000, -0.000000000000000000 ) ) ;
#91323 = CARTESIAN_POINT ( 'NONE',  ( -51.22478625508527728, -25.16632228261309123, 6.837805518550829298 ) ) ;
#91324 = CARTESIAN_POINT ( 'NONE',  ( 2.879247915899910470, -19.84986158617241614, 11.49999999999998934 ) ) ;
#91325 = LINE ( 'NONE', #21799, #24058 ) ;
#91326 = VERTEX_POINT ( 'NONE', #1450 ) ;
#91327 = CARTESIAN_POINT ( 'NONE',  ( -116.5228709571500616, -29.50247984919015209, -1.443849546365046699 ) ) ;
#91328 = CARTESIAN_POINT ( 'NONE',  ( -18.62658236799572720, 13.20813282334384553, 11.49999999999999645 ) ) ;
#91329 = CARTESIAN_POINT ( 'NONE',  ( -49.51279233427662518, -25.26258742029363447, 4.076580261917981396 ) ) ;
#91330 = LINE ( 'NONE', #67511, #89916 ) ;
#91331 = LINE ( 'NONE', #76098, #72734 ) ;
#91332 = CARTESIAN_POINT ( 'NONE',  ( 5.766314450391940127, -5.876774720514423400, 21.17177008079512035 ) ) ;
#91333 = CARTESIAN_POINT ( 'NONE',  ( -88.88918693012689687, -29.50249691823240994, 6.409318347766594037 ) ) ;
#91334 = VECTOR ( 'NONE', #99404, 1000.000000000000000 ) ;
#91335 = CARTESIAN_POINT ( 'NONE',  ( 30.09341516180546350, -1.477225279485574028, -11.39311774897855756 ) ) ;
#91336 = ORIENTED_EDGE ( 'NONE', *, *, #20786, .F. ) ;
#91337 = ADVANCED_FACE ( 'NONE', ( #16653, #78544 ), #77047, .T. ) ;
#91338 = CARTESIAN_POINT ( 'NONE',  ( -20.15914900662387055, -2.930279687489938389, -1.500000000000002220 ) ) ;
#91339 = VECTOR ( 'NONE', #28896, 1000.000000000000000 ) ;
#91341 = EDGE_CURVE ( 'NONE', #43797, #67869, #70960, .T. ) ;
#91340 = ORIENTED_EDGE ( 'NONE', *, *, #39984, .F. ) ;
#91342 = CARTESIAN_POINT ( 'NONE',  ( 16.23347398924790497, -16.23827457187686463, 11.49999999999998934 ) ) ;
#91343 = CARTESIAN_POINT ( 'NONE',  ( -37.55620429048340725, -24.65952944569304250, 1.056160979905692132 ) ) ;
#91344 = EDGE_CURVE ( 'NONE', #56484, #34878, #7548, .T. ) ;
#91345 = ORIENTED_EDGE ( 'NONE', *, *, #33502, .F. ) ;
#91346 = CARTESIAN_POINT ( 'NONE',  ( -108.5148028597040337, -24.35071581493544457, 9.817618358456016381 ) ) ;
#91347 = EDGE_CURVE ( 'NONE', #21600, #4176, #1530, .T. ) ;
#91348 = DIRECTION ( 'NONE',  ( -0.000000000000000000, 1.000000000000000000, -0.000000000000000000 ) ) ;
#91349 = CARTESIAN_POINT ( 'NONE',  ( -51.54139007992708343, -24.35071581493542681, 9.817618358456028815 ) ) ;
#91351 = ORIENTED_EDGE ( 'NONE', *, *, #69511, .T. ) ;
#91350 = CARTESIAN_POINT ( 'NONE',  ( 18.67678363807796416, 10.12720680154768971, 11.49999999999999645 ) ) ;
#91352 = ORIENTED_EDGE ( 'NONE', *, *, #23414, .T. ) ;
#91353 = CARTESIAN_POINT ( 'NONE',  ( 22.14152233036116257, 1.636640089565777334, 11.49999999999998934 ) ) ;
#91354 = CARTESIAN_POINT ( 'NONE',  ( -19.87711886888390822, 5.503898473480427711, -1.500000000000002220 ) ) ;
#91355 = EDGE_LOOP ( 'NONE', ( #13714, #22100, #57208, #20208 ) ) ;
#91356 = ORIENTED_EDGE ( 'NONE', *, *, #40780, .T. ) ;
#91357 = PLANE ( 'NONE',  #81966 ) ;
#91358 = B_SPLINE_CURVE_WITH_KNOTS ( 'NONE', 3,
 ( #52259, #58384, #50765, #12180 ),
 .UNSPECIFIED., .F., .F.,
 ( 4, 4 ),
 ( 0.000000000000000000, 9.999999999998900014E-05 ),
 .UNSPECIFIED. ) ;
#91359 = CARTESIAN_POINT ( 'NONE',  ( 3.113719597313231002, -5.876774720514426065, 21.58936759753562029 ) ) ;
#91360 = ORIENTED_EDGE ( 'NONE', *, *, #94882, .F. ) ;
#91361 = ORIENTED_EDGE ( 'NONE', *, *, #43474, .F. ) ;
#91362 = CARTESIAN_POINT ( 'NONE',  ( -0.02075734969026423599, 3.316774720514426456, -0.08597719988137648983 ) ) ;
#91363 = CARTESIAN_POINT ( 'NONE',  ( -41.62371469989763284, -24.66019654487199375, 8.947790411086122830 ) ) ;
#91364 = DIRECTION ( 'NONE',  ( -1.000000000000000000, 0.000000000000000000, 0.000000000000000000 ) ) ;
#91365 = CARTESIAN_POINT ( 'NONE',  ( 15.94631523246878579, 13.42178585792578360, -1.500000000000002220 ) ) ;
#91366 = CARTESIAN_POINT ( 'NONE',  ( 8.287826148123016878, -20.17477452812186201, 11.49999999999999645 ) ) ;
#91367 = VECTOR ( 'NONE', #4244, 1000.000000000000000 ) ;
#91368 = CARTESIAN_POINT ( 'NONE',  ( -40.62552394256396582, -25.27806136706950468, 5.067902527831130932 ) ) ;
#91369 = CARTESIAN_POINT ( 'NONE',  ( -52.52287095715005449, -23.47593901973090524, -1.443836447538997092 ) ) ;
#91370 = CARTESIAN_POINT ( 'NONE',  ( -20.53624283083718893, 9.024085183690161216, 11.49999999999998934 ) ) ;
#91371 = CARTESIAN_POINT ( 'NONE',  ( -50.88361436997121245, -25.26334723850860442, 4.608108886914586755 ) ) ;
#91372 = EDGE_LOOP ( 'NONE', ( #36742, #720, #68653, #8301 ) ) ;
#91373 = DIRECTION ( 'NONE',  ( 0.000000000000000000, 0.9999999999976377785, 2.173523156925979552E-06 ) ) ;
#91374 = CARTESIAN_POINT ( 'NONE',  ( -51.40669398549582780, -25.17894756043024884, 3.249225598437226470 ) ) ;
#91375 = AXIS2_PLACEMENT_3D ( 'NONE', #83483, #38806, #15467 ) ;
#91376 = ORIENTED_EDGE ( 'NONE', *, *, #3614, .F. ) ;
#91377 = ORIENTED_EDGE ( 'NONE', *, *, #91636, .T. ) ;
#91378 = CARTESIAN_POINT ( 'NONE',  ( 15.29947330337543754, -6.376774720514426953, -27.16854002387008649 ) ) ;
#91379 = EDGE_LOOP ( 'NONE', ( #26384, #19885, #13026, #31466 ) ) ;
#91380 = CARTESIAN_POINT ( 'NONE',  ( 2.936642053869352953, -21.15864249054145674, -1.500000000000002220 ) ) ;
#91381 = VERTEX_POINT ( 'NONE', #38502 ) ;
#91382 = LINE ( 'NONE', #65421, #56039 ) ;
#91383 = CARTESIAN_POINT ( 'NONE',  ( -20.73700405699343463, 3.470425206167693233, 11.49999999999998934 ) ) ;
#91384 = FACE_OUTER_BOUND ( 'NONE', #66828, .T. ) ;
#91385 = CARTESIAN_POINT ( 'NONE',  ( -111.3776484685884469, -25.29712067403330877, 4.332404411321261861 ) ) ;
#91386 = DIRECTION ( 'NONE',  ( -1.000000000000000000, -3.773278334444166432E-23, -8.201307841325785021E-29 ) ) ;
#91387 = CARTESIAN_POINT ( 'NONE',  ( 21.74639208212181529, -2.611101805624240768, -1.500000000000002220 ) ) ;
#91388 = CARTESIAN_POINT ( 'NONE',  ( -87.55130954339645655, -24.15543982623908192, -0.2315651400026449980 ) ) ;
#91389 = ORIENTED_EDGE ( 'NONE', *, *, #87373, .T. ) ;
#91390 = CARTESIAN_POINT ( 'NONE',  ( -122.5557265984356121, -23.96169478059714564, 10.65365249895717170 ) ) ;
#91391 = EDGE_CURVE ( 'NONE', #94778, #96462, #18991, .T. ) ;
#91392 = CARTESIAN_POINT ( 'NONE',  ( -84.54748922658383492, -24.35071581493543391, 9.817618358456027039 ) ) ;
#91393 = CARTESIAN_POINT ( 'NONE',  ( -130.5728709571501156, -24.04668586515359863, 10.47594215909544069 ) ) ;
#91394 = CARTESIAN_POINT ( 'NONE',  ( -0.05748996396964650701, -22.30574723846597607, 8.909134979017292011 ) ) ;
#91395 = CARTESIAN_POINT ( 'NONE',  ( 14.87313431965483801, 15.23822737908125902, 11.49999999999998934 ) ) ;
#91396 = CARTESIAN_POINT ( 'NONE',  ( -98.55007674334730439, -24.35071581493543391, 9.817618358456027039 ) ) ;
#91397 = CARTESIAN_POINT ( 'NONE',  ( -54.58953762381672448, -23.47593901973091235, -1.443836447539009749 ) ) ;
#91398 = ADVANCED_FACE ( 'NONE', ( #80481 ), #25695, .F. ) ;
#91399 = CARTESIAN_POINT ( 'NONE',  ( -60.62287095715004881, -23.47596703998600631, 11.44779298504227505 ) ) ;
#91400 = CARTESIAN_POINT ( 'NONE',  ( -33.66791791009761425, -23.48783264082477729, -1.443836473390078368 ) ) ;
#91401 = CARTESIAN_POINT ( 'NONE',  ( 17.77913403553526805, 13.70458096452923691, -1.500000000000002220 ) ) ;
#91402 = CARTESIAN_POINT ( 'NONE',  ( -60.52287095715006160, -25.00158670708908915, 2.256160236439166411 ) ) ;
#91403 = EDGE_LOOP ( 'NONE', ( #98986, #88604, #8624, #84420 ) ) ;
#91404 = CARTESIAN_POINT ( 'NONE',  ( -10.34999999999999254, 1.999999999999999112, 0.000000000000000000 ) ) ;
#91405 = CARTESIAN_POINT ( 'NONE',  ( -17.63651738508609412, 8.604534254076446231, 11.49999999999999645 ) ) ;
#91406 = LINE ( 'NONE', #84798, #68168 ) ;
#91407 = FACE_OUTER_BOUND ( 'NONE', #16263, .T. ) ;
#91408 = ORIENTED_EDGE ( 'NONE', *, *, #73141, .T. ) ;
#91409 = FACE_OUTER_BOUND ( 'NONE', #96847, .T. ) ;
#91410 = DIRECTION ( 'NONE',  ( -1.000000000000000000, -3.773278334444166432E-23, -8.201307841325785021E-29 ) ) ;
#91411 = CARTESIAN_POINT ( 'NONE',  ( -89.90088307144425528, -25.32379766982192493, 4.367815445636562544 ) ) ;
#91412 = B_SPLINE_CURVE_WITH_KNOTS ( 'NONE', 3,
 ( #11380, #18491, #66196, #73288, #59068, #27108 ),
 .UNSPECIFIED., .F., .F.,
 ( 4, 2, 4 ),
 ( 1.570755371634454886E-05, 0.001396183895866089488, 0.002776660238015834711 ),
 .UNSPECIFIED. ) ;
#91413 = CARTESIAN_POINT ( 'NONE',  ( 0.1645010273463760886, 1.417169167140627462, -0.3687607960183705846 ) ) ;
#91414 = CARTESIAN_POINT ( 'NONE',  ( -19.65353550717971487, 1.628721094194526486, -1.500000000000002220 ) ) ;
#91415 = ORIENTED_EDGE ( 'NONE', *, *, #30525, .T. ) ;
#91416 = FACE_OUTER_BOUND ( 'NONE', #3213, .T. ) ;
#91417 = DIRECTION ( 'NONE',  ( 0.000000000000000000, -0.9999999999976377785, -2.173523156925979128E-06 ) ) ;
#91418 = AXIS2_PLACEMENT_3D ( 'NONE', #26934, #96442, #65525 ) ;
#91419 = PERSON_AND_ORGANIZATION ( #70597, #27821 ) ;
#91420 = EDGE_LOOP ( 'NONE', ( #5509, #88930, #45183, #12751 ) ) ;
#91421 = DIRECTION ( 'NONE',  ( 0.000000000000000000, -0.9999999999976377785, -2.173523156925979975E-06 ) ) ;
#91422 = CARTESIAN_POINT ( 'NONE',  ( -84.62287095715005592, -23.48783264082479150, -1.443836473390065489 ) ) ;
#91423 = CARTESIAN_POINT ( 'NONE',  ( -55.53423014570002181, -24.73486907724917572, 1.287355809206960355 ) ) ;
#91424 = LINE ( 'NONE', #92924, #63949 ) ;
#91425 = CARTESIAN_POINT ( 'NONE',  ( -121.6228709571500417, -24.65952944569305316, 1.056160979905705677 ) ) ;
#91426 = CARTESIAN_POINT ( 'NONE',  ( -1.358974358974355257, -6.376774720514427841, 21.75000000000000711 ) ) ;
#91427 = CARTESIAN_POINT ( 'NONE',  ( -107.6297646753413346, -23.96119346886881374, -0.6495511937831857097 ) ) ;
#91428 = CARTESIAN_POINT ( 'NONE',  ( -19.24466553037914807, -5.328869878250761971, -1.500000000000002220 ) ) ;
#91429 = VECTOR ( 'NONE', #9872, 1000.000000000000114 ) ;
#91430 = CARTESIAN_POINT ( 'NONE',  ( -125.6228709571500559, -23.48786465467241769, 11.44779295918253403 ) ) ;
#91431 = CARTESIAN_POINT ( 'NONE',  ( -45.48069253931505784, -24.73531770709094957, 8.716586749053515604 ) ) ;
#91432 = VERTEX_POINT ( 'NONE', #32814 ) ;
#91433 = CARTESIAN_POINT ( 'NONE',  ( 4.653726706778644306, -6.376774720514415407, 20.04674869880385302 ) ) ;
#91434 = B_SPLINE_CURVE_WITH_KNOTS ( 'NONE', 3,
 ( #402, #55212, #70422, #63836 ),
 .UNSPECIFIED., .F., .F.,
 ( 4, 4 ),
 ( 0.9894921560719619480, 0.9904929031127274186 ),
 .UNSPECIFIED. ) ;
#91435 = CARTESIAN_POINT ( 'NONE',  ( -129.6228709571500417, -23.47596703998600631, 11.44779298504227683 ) ) ;
#91436 = CARTESIAN_POINT ( 'NONE',  ( -80.51502784577047578, -23.85049219812685806, 10.88485053497527311 ) ) ;
#91437 = CARTESIAN_POINT ( 'NONE',  ( 1.140932434931746582E-13, -6.376774720514426953, 21.78128695274321203 ) ) ;
#91438 = CARTESIAN_POINT ( 'NONE',  ( -39.62888266615128430, -24.51314013834315730, 0.6176544820404118452 ) ) ;
#91439 = DIRECTION ( 'NONE',  ( -0.000000000000000000, 0.000000000000000000, -1.000000000000000000 ) ) ;
#91440 = CARTESIAN_POINT ( 'NONE',  ( -1.845912073933368536, -5.876774720514408301, 19.53740760792477360 ) ) ;
#91441 = DIRECTION ( 'NONE',  ( -0.000000000000000000, 1.000000000000000000, -0.000000000000000000 ) ) ;
#91442 = DIRECTION ( 'NONE',  ( -3.773278334453079618E-23, 0.9999999999976377785, 2.173523156925979975E-06 ) ) ;
#91443 = EDGE_LOOP ( 'NONE', ( #13850, #30177, #56604, #93319 ) ) ;
#91444 = ADVANCED_FACE ( 'NONE', ( #72387 ), #14520, .T. ) ;
#91445 = CARTESIAN_POINT ( 'NONE',  ( -6.888417027594036846, 19.07602104198033643, -1.500000000000002220 ) ) ;
#91446 = B_SPLINE_CURVE_WITH_KNOTS ( 'NONE', 3,
 ( #25704, #56178, #17093, #48569, #88118, #87104 ),
 .UNSPECIFIED., .F., .F.,
 ( 4, 2, 4 ),
 ( 0.000000000000000000, 0.001380901958385395483, 0.002761803916770790967 ),
 .UNSPECIFIED. ) ;
#91447 = CARTESIAN_POINT ( 'NONE',  ( -69.83931149620484291, -25.31531697701531769, 4.914945103882936372 ) ) ;
#91448 = CARTESIAN_POINT ( 'NONE',  ( 14.92791587776674334, 5.037605299509791301, -27.26084882802267373 ) ) ;
#91449 = EDGE_CURVE ( 'NONE', #19254, #52189, #10470, .T. ) ;
#91450 = DIRECTION ( 'NONE',  ( 0.000000000000000000, 0.000000000000000000, -1.000000000000000000 ) ) ;
#91451 = EDGE_CURVE ( 'NONE', #81045, #38437, #15210, .T. ) ;
#91452 = ORIENTED_EDGE ( 'NONE', *, *, #51547, .T. ) ;
#91453 = CARTESIAN_POINT ( 'NONE',  ( -81.52287095715006160, -29.50248528299804818, 1.056150453629038477 ) ) ;
#91454 = CARTESIAN_POINT ( 'NONE',  ( -62.22287095715008576, -23.47596703998600276, 11.44779298504227683 ) ) ;
#91455 = CARTESIAN_POINT ( 'NONE',  ( 19.67429046578372365, -4.105084037421226739, -1.500000000000002220 ) ) ;
#91456 = EDGE_CURVE ( 'NONE', #62727, #4330, #58708, .T. ) ;
#91457 = CARTESIAN_POINT ( 'NONE',  ( -8.945158345017247825, -19.07159632999312393, 11.49999999999999645 ) ) ;
#91458 = AXIS2_PLACEMENT_3D ( 'NONE', #25290, #79579, #452 ) ;
#91459 = DIRECTION ( 'NONE',  ( 0.000000000000000000, 1.000000000000000000, 0.000000000000000000 ) ) ;
#91460 = CARTESIAN_POINT ( 'NONE',  ( -21.51168160490077952, -5.175097382202364926, 11.49999999999998934 ) ) ;
#91461 = EDGE_CURVE ( 'NONE', #30931, #5385, #28700, .T. ) ;
#91462 = CARTESIAN_POINT ( 'NONE',  ( 20.13950599927006735, 4.067174238878714654, 11.49999999999998934 ) ) ;
#91464 = CARTESIAN_POINT ( 'NONE',  ( 2.230654205607476293, -6.505213034913026604E-16, -0.1647943925233646134 ) ) ;
#91463 = B_SPLINE_CURVE_WITH_KNOTS ( 'NONE', 3,
 ( #67575, #5656, #59455, #7656 ),
 .UNSPECIFIED., .F., .F.,
 ( 4, 4 ),
 ( 0.03697762237835398869, 0.06648419838821313654 ),
 .UNSPECIFIED. ) ;
#91465 = CARTESIAN_POINT ( 'NONE',  ( -60.66488206965777863, -23.48783264082476308, -1.443836473390097686 ) ) ;
#91466 = ORIENTED_EDGE ( 'NONE', *, *, #59915, .T. ) ;
#91467 = PLANE ( 'NONE',  #68717 ) ;
#91468 = ORIENTED_EDGE ( 'NONE', *, *, #72066, .T. ) ;
#91469 = CARTESIAN_POINT ( 'NONE',  ( -35.52287095715008292, -24.15516710230293640, 10.28746687063726561 ) ) ;
#91470 = B_SPLINE_SURFACE_WITH_KNOTS ( 'NONE', 3, 3, ( 
 ( #8510, #55201, #1409, #1907 ),
 ( #31342, #32343, #63319, #94237 ),
 ( #69410, #24722, #77998, #55703 ),
 ( #48083, #25226, #79009, #54201 ),
 ( #54693, #40467, #63826, #23723 ),
 ( #71416, #38952, #100327, #32850 ),
 ( #23216, #94739, #56204, #62308 ),
 ( #17622, #85125, #48594, #7503 ),
 ( #15611, #77502, #93233, #16112 ),
 ( #39461, #70411, #897, #58684 ) ),
 .UNSPECIFIED., .F., .F., .F.,
 ( 4, 3, 3, 4 ),
 ( 4, 4 ),
 ( 0.0004766839783821102895, 0.1491231665100173909, 0.2234464077758350209, 0.2977696490416526509 ),
 ( 0.5495603723122651774, 0.5509005773147922502 ),
 .UNSPECIFIED. ) ;
#91471 = PLANE ( 'NONE',  #93942 ) ;
#91472 = ORIENTED_EDGE ( 'NONE', *, *, #30454, .T. ) ;
#91473 = ORIENTED_EDGE ( 'NONE', *, *, #6799, .F. ) ;
#91474 = DIRECTION ( 'NONE',  ( 0.7689940216596065081, -7.885106708985488048E-16, -0.6392559695863502256 ) ) ;
#91475 = CARTESIAN_POINT ( 'NONE',  ( -95.52287095715011844, -23.48783264082477373, -1.443836473390086139 ) ) ;
#91477 = ADVANCED_FACE ( 'NONE', ( #90591 ), #89103, .T. ) ;
#91476 = PLANE ( 'NONE',  #63345 ) ;
#91478 = CARTESIAN_POINT ( 'NONE',  ( -7.851838630353038972, -19.11370409007043847, -1.500000000000002220 ) ) ;
#91479 = CARTESIAN_POINT ( 'NONE',  ( -20.67203406374276398, -6.343553224398504220, 11.49999999999999645 ) ) ;
#91480 = ORIENTED_EDGE ( 'NONE', *, *, #41302, .F. ) ;
#91481 = CARTESIAN_POINT ( 'NONE',  ( -56.55620429048339304, -24.66019654487199020, 8.947790411086133489 ) ) ;
#91482 = DIRECTION ( 'NONE',  ( 0.000000000000000000, 1.000000000000000000, 0.000000000000000000 ) ) ;
#91483 = CARTESIAN_POINT ( 'NONE',  ( 12.52526618502215250, 18.50471055633022388, 11.49999999999998934 ) ) ;
#91484 = CARTESIAN_POINT ( 'NONE',  ( -79.68206046389329344, -25.12205741196211051, 6.776761561512239851 ) ) ;
#91485 = CARTESIAN_POINT ( 'NONE',  ( -61.52287095715006160, -24.64898659630367916, 1.056161002820822592 ) ) ;
#91486 = ORIENTED_EDGE ( 'NONE', *, *, #35464, .F. ) ;
#91487 = CARTESIAN_POINT ( 'NONE',  ( -43.58953762381672448, -23.47593901973091235, -1.443836447539011525 ) ) ;
#91488 = CARTESIAN_POINT ( 'NONE',  ( -49.53586925223535076, -24.51419770103158413, 9.386484678747189392 ) ) ;
#91489 = CARTESIAN_POINT ( 'NONE',  ( -19.40664508603899563, 7.695215611089875729, 11.49999999999998934 ) ) ;
#91490 = ORIENTED_EDGE ( 'NONE', *, *, #22814, .T. ) ;
#91491 = VECTOR ( 'NONE', #100283, 1000.000000000000114 ) ;
#91493 = ORIENTED_EDGE ( 'NONE', *, *, #40669, .T. ) ;
#91492 = CARTESIAN_POINT ( 'NONE',  ( -86.52215078430889150, -23.48783264082478084, -1.443836473390066377 ) ) ;
#91494 = B_SPLINE_CURVE_WITH_KNOTS ( 'NONE', 3,
 ( #61557, #22950, #46824, #84871, #69660, #137 ),
 .UNSPECIFIED., .F., .F.,
 ( 4, 2, 4 ),
 ( 0.000000000000000000, 0.001380764517853250986, 0.002761529035706501971 ),
 .UNSPECIFIED. ) ;
#91495 = ORIENTED_EDGE ( 'NONE', *, *, #27171, .F. ) ;
#91496 = CARTESIAN_POINT ( 'NONE',  ( -109.5167357964235322, -24.15620529776628445, 10.23563542870660115 ) ) ;
#91497 = CARTESIAN_POINT ( 'NONE',  ( 19.39439428382967634, -8.317090367284466268, -1.500000000000002220 ) ) ;
#91498 = ORIENTED_EDGE ( 'NONE', *, *, #73318, .F. ) ;
#91499 = CARTESIAN_POINT ( 'NONE',  ( -112.5228709571500332, -24.50321055353805377, 9.387540953477518713 ) ) ;
#91500 = CARTESIAN_POINT ( 'NONE',  ( -100.1979988280279201, -25.26221314647534300, 7.085054734328950943 ) ) ;
#91501 = CARTESIAN_POINT ( 'NONE',  ( -19.96617879207914825, 8.700599545123990808, 11.49999999999998934 ) ) ;
#91502 = LINE ( 'NONE', #98113, #95137 ) ;
#91503 = CARTESIAN_POINT ( 'NONE',  ( -35.55620429048340014, -24.99156044556202261, 7.747789690856173195 ) ) ;
#91504 = CARTESIAN_POINT ( 'NONE',  ( -80.18909136271707894, -25.13912158888506099, 7.067238146532562659 ) ) ;
#91505 = CARTESIAN_POINT ( 'NONE',  ( 1.937016913031804455, -21.67664703184077268, -1.500000000000002220 ) ) ;
#91506 = CARTESIAN_POINT ( 'NONE',  ( -78.95132930790050807, -25.25821045354187078, 6.187260761811991472 ) ) ;
#91508 = ORIENTED_EDGE ( 'NONE', *, *, #75096, .F. ) ;
#91507 = CARTESIAN_POINT ( 'NONE',  ( 12.52526618502215250, 18.50471055633022388, 11.49999999999999645 ) ) ;
#91509 = CARTESIAN_POINT ( 'NONE',  ( 0.3910256410256418014, -6.376774720514418959, 20.67377804487179915 ) ) ;
#91510 = CARTESIAN_POINT ( 'NONE',  ( -85.58094713038467205, -25.00182538069147142, 7.747789668545045139 ) ) ;
#91511 = EDGE_CURVE ( 'NONE', #31248, #64842, #94997, .T. ) ;
#91513 = CARTESIAN_POINT ( 'NONE',  ( 30.32108885906865936, -6.376774720514427841, 3.274824222184972822 ) ) ;
#91512 = B_SPLINE_CURVE_WITH_KNOTS ( 'NONE', 3,
 ( #1508, #32444, #24824, #71520, #25830, #37671 ),
 .UNSPECIFIED., .F., .F.,
 ( 4, 2, 4 ),
 ( 0.000000000000000000, 0.001380764517854760412, 0.002761529035709520824 ),
 .UNSPECIFIED. ) ;
#91514 = ORIENTED_EDGE ( 'NONE', *, *, #86545, .F. ) ;
#91515 = AXIS2_PLACEMENT_3D ( 'NONE', #24241, #54709, #1420 ) ;
#91516 = B_SPLINE_CURVE_WITH_KNOTS ( 'NONE', 3,
 ( #32167, #94067, #48411, #70239 ),
 .UNSPECIFIED., .F., .F.,
 ( 4, 4 ),
 ( 6.938893903907227607E-18, 9.999999999999593903E-05 ),
 .UNSPECIFIED. ) ;
#91517 = VERTEX_POINT ( 'NONE', #74367 ) ;
#91518 = EDGE_CURVE ( 'NONE', #35425, #79911, #66282, .T. ) ;
#91519 = B_SPLINE_CURVE_WITH_KNOTS ( 'NONE', 3,
 ( #84681, #54253, #85183, #15672, #8062, #18176 ),
 .UNSPECIFIED., .F., .F.,
 ( 4, 2, 4 ),
 ( 1.570755371633915156E-05, 0.001396183895866086452, 0.002776660238015833844 ),
 .UNSPECIFIED. ) ;
#91520 = ORIENTED_EDGE ( 'NONE', *, *, #84654, .T. ) ;
#91521 = CARTESIAN_POINT ( 'NONE',  ( 5.097264368846809113, -1.579225279485572342, -27.56135813788808875 ) ) ;
#91522 = CARTESIAN_POINT ( 'NONE',  ( -10.79823215447539653, -18.26288818932900071, 11.49999999999998934 ) ) ;
#91523 = LINE ( 'NONE', #67716, #2803 ) ;
#91524 = CARTESIAN_POINT ( 'NONE',  ( -79.10019335338344604, -25.03138112166652007, 6.701029380949082181 ) ) ;
#91525 = CARTESIAN_POINT ( 'NONE',  ( -63.52287095715006160, -29.50250243563736774, 8.947779886222145151 ) ) ;
#91526 = CARTESIAN_POINT ( 'NONE',  ( 32.87794144969610244, 3.622774687813811845, -13.08434676285136256 ) ) ;
#91527 = CARTESIAN_POINT ( 'NONE',  ( -1.480291460309441920, -19.30061035156251847, -1.500000000000002220 ) ) ;
#91528 = EDGE_CURVE ( 'NONE', #79185, #38725, #13457, .T. ) ;
#91529 = CARTESIAN_POINT ( 'NONE',  ( -51.89024320248035593, -25.28679719141751647, 5.841385604566403877 ) ) ;
#91530 = ORIENTED_EDGE ( 'NONE', *, *, #23680, .T. ) ;
#91531 = CARTESIAN_POINT ( 'NONE',  ( -4.672984603565591755, -18.88948546680484242, 11.49999999999999645 ) ) ;
#91532 = DIRECTION ( 'NONE',  ( -1.000000000000000000, 8.673617379884040402E-17, -6.938893903907232322E-16 ) ) ;
#91533 = EDGE_CURVE ( 'NONE', #80499, #33585, #50537, .T. ) ;
#91534 = ORIENTED_EDGE ( 'NONE', *, *, #55916, .F. ) ;
#91535 = CARTESIAN_POINT ( 'NONE',  ( 2.909586618535765723, -6.376774720514411854, 19.75512108203924200 ) ) ;
#91536 = CARTESIAN_POINT ( 'NONE',  ( 3.116263380642223968, -5.876774720514402084, 18.40799819116699609 ) ) ;
#91537 = DIRECTION ( 'NONE',  ( 0.000000000000000000, 0.9999999999976377785, 2.173523156925979975E-06 ) ) ;
#91538 = DIRECTION ( 'NONE',  ( 0.000000000000000000, -0.8403332392196035672, 0.5420701495772373146 ) ) ;
#91539 = CARTESIAN_POINT ( 'NONE',  ( 9.307004028210867475, 17.29072351678862418, 11.49999999999998934 ) ) ;
#91540 = CARTESIAN_POINT ( 'NONE',  ( -0.02075734969026423599, 3.316774720514426456, -0.08597719988137648983 ) ) ;
#91541 = VERTEX_POINT ( 'NONE', #57662 ) ;
#91542 = AXIS2_PLACEMENT_3D ( 'NONE', #71735, #65142, #89450 ) ;
#91543 = CARTESIAN_POINT ( 'NONE',  ( 10.28227983848843152, -18.94921665015282031, -1.500000000000002220 ) ) ;
#91544 = DIRECTION ( 'NONE',  ( 0.000000000000000000, 1.000000000000000000, 0.000000000000000000 ) ) ;
#91545 = CARTESIAN_POINT ( 'NONE',  ( -70.78633892220865675, -25.25639579675769752, 7.001279323389742792 ) ) ;
#91546 = CARTESIAN_POINT ( 'NONE',  ( -43.52287095715004739, -23.48783264083374078, -1.443836473376152840 ) ) ;
#91547 = CARTESIAN_POINT ( 'NONE',  ( -99.62727860833967952, -25.18439417509214096, 3.670122307788938887 ) ) ;
#91548 = CARTESIAN_POINT ( 'NONE',  ( 18.43541038833219758, -13.85303862407246811, -1.500000000000002220 ) ) ;
#91549 = CC_DESIGN_DATE_AND_TIME_ASSIGNMENT ( #50519, #25173, ( #3711 ) ) ;
#91550 = PERSON_AND_ORGANIZATION_ROLE ( 'creator' ) ;
#91551 = CARTESIAN_POINT ( 'NONE',  ( -93.59138681930647863, -24.15543982623907482, -0.2315651400026620677 ) ) ;
#91552 = CARTESIAN_POINT ( 'NONE',  ( -49.48509645508600840, -24.65952944569304606, 1.056160979905696129 ) ) ;
#91553 = CARTESIAN_POINT ( 'NONE',  ( 16.68447708738676383, -11.30049470069299922, 11.49999999999999645 ) ) ;
#91554 = CARTESIAN_POINT ( 'NONE',  ( -45.62287095715004881, -24.14406661707768720, 10.28769366152059739 ) ) ;
#91555 = DIRECTION ( 'NONE',  ( 0.000000000000000000, -2.173523156925979552E-06, 0.9999999999976378895 ) ) ;
#91556 = CARTESIAN_POINT ( 'NONE',  ( -94.55620429048340725, -23.48786465467241413, 11.44779295918254647 ) ) ;
#91557 = DIRECTION ( 'NONE',  ( 0.000000000000000000, -1.000000000000000000, 0.000000000000000000 ) ) ;
#91558 = CARTESIAN_POINT ( 'NONE',  ( -110.4389802415574309, -25.29779155955683478, 3.296667605415470881 ) ) ;
#91559 = CARTESIAN_POINT ( 'NONE',  ( 11.24879072547334324, 16.40116332625411033, -1.500000000000002220 ) ) ;
#91560 = DIRECTION ( 'NONE',  ( -0.000000000000000000, -1.000000000000000000, -0.000000000000000000 ) ) ;
#91561 = CARTESIAN_POINT ( 'NONE',  ( -16.30015253881794379, -11.17962500214296639, -1.500000000000002220 ) ) ;
#91562 = CARTESIAN_POINT ( 'NONE',  ( -126.5891254613743797, -24.66019654487200796, 8.947790411086103290 ) ) ;
#91563 = CARTESIAN_POINT ( 'NONE',  ( -0.7067007548136460260, -6.376774720514410077, 19.51517878119693350 ) ) ;
#91564 = CARTESIAN_POINT ( 'NONE',  ( -2.196420576317535289, -6.376774720514410077, 19.14926908420044782 ) ) ;
#91565 = CARTESIAN_POINT ( 'NONE',  ( 20.68991284688621946, 0.5745778482356619365, 11.49999999999999645 ) ) ;
#91566 = PLANE ( 'NONE',  #7849 ) ;
#91567 = VECTOR ( 'NONE', #53636, 1000.000000000000000 ) ;
#91568 = CARTESIAN_POINT ( 'NONE',  ( 31.50451260799805198, 4.115674466082359650, -1.392914706732841790 ) ) ;
#91569 = CARTESIAN_POINT ( 'NONE',  ( -50.26765004257320868, -25.25138673217113094, 5.200244656635645946 ) ) ;
#91570 = CARTESIAN_POINT ( 'NONE',  ( 13.52301212282245935, 18.22803923376396540, 11.49999999999999645 ) ) ;
#91571 = VERTEX_POINT ( 'NONE', #58160 ) ;
#91572 = LINE ( 'NONE', #68749, #23592 ) ;
#91573 = CARTESIAN_POINT ( 'NONE',  ( -70.32380231474228083, -25.12298712672050982, 7.101635559041870494 ) ) ;
#91574 = CARTESIAN_POINT ( 'NONE',  ( -12.46103870137906711, 15.87156016069071462, 11.49999999999998934 ) ) ;
#91575 = ADVANCED_FACE ( 'NONE', ( #80988 ), #20078, .F. ) ;
#91576 = CARTESIAN_POINT ( 'NONE',  ( 8.971512145086503409, -0.9869079657328782007, -3.741933919974615552 ) ) ;
#91577 = VECTOR ( 'NONE', #80407, 1000.000000000000000 ) ;
#91578 = CARTESIAN_POINT ( 'NONE',  ( -41.40661852069504079, -25.29534531538531894, 4.500433469842812784 ) ) ;
#91579 = ORIENTED_EDGE ( 'NONE', *, *, #65277, .T. ) ;
#91580 = AXIS2_PLACEMENT_3D ( 'NONE', #46302, #85868, #70641 ) ;
#91581 = VERTEX_POINT ( 'NONE', #88605 ) ;
#91582 = DIRECTION ( 'NONE',  ( 1.000000000000000000, 3.773278334444167608E-23, 8.201307833595939069E-29 ) ) ;
#91583 = CARTESIAN_POINT ( 'NONE',  ( -17.51315278866654879, 14.73147661606379621, -1.500000000000002220 ) ) ;
#91584 = CARTESIAN_POINT ( 'NONE',  ( -111.3711097089617965, -25.28332809916757640, 4.263977541267919058 ) ) ;
#91585 = CARTESIAN_POINT ( 'NONE',  ( 16.85579979752674618, 13.57973486276658903, -1.500000000000002220 ) ) ;
#91586 = CARTESIAN_POINT ( 'NONE',  ( -30.57287095715006942, -23.48213395187224606, 11.44779283644488999 ) ) ;
#91587 = CARTESIAN_POINT ( 'NONE',  ( -114.6228709571500559, -23.47593901973091235, -1.443836447538999312 ) ) ;
#91588 = ADVANCED_FACE ( 'NONE', ( #81491 ), #67997, .T. ) ;
#91589 = CARTESIAN_POINT ( 'NONE',  ( -9.975069251262826953, -18.38325097723136992, 11.49999999999999645 ) ) ;
#91590 = VERTEX_POINT ( 'NONE', #98697 ) ;
#91591 = CARTESIAN_POINT ( 'NONE',  ( -87.22287095715009286, -23.47593901973090880, -1.443836447538997314 ) ) ;
#91592 = CARTESIAN_POINT ( 'NONE',  ( -4.682628417673765142, 21.48327871026360114, 11.49999999999998934 ) ) ;
#91593 = EDGE_CURVE ( 'NONE', #17901, #39863, #87342, .T. ) ;
#91594 = CARTESIAN_POINT ( 'NONE',  ( -105.5497123930152270, -24.63419186844610920, 9.035850630976920428 ) ) ;
#91595 = CARTESIAN_POINT ( 'NONE',  ( -41.86772617331516955, -25.29087320296346775, 4.147750017007223455 ) ) ;
#91596 = ORIENTED_EDGE ( 'NONE', *, *, #68767, .F. ) ;
#91597 = CARTESIAN_POINT ( 'NONE',  ( -73.58953762381672448, -23.47593901973091235, -1.443836447539006196 ) ) ;
#91598 = DIRECTION ( 'NONE',  ( 1.000000000000000000, 3.773278334444167608E-23, 8.201307833595939069E-29 ) ) ;
#91599 = ORIENTED_EDGE ( 'NONE', *, *, #19087, .T. ) ;
#91600 = DIRECTION ( 'NONE',  ( 0.000000000000000000, -1.000000000000000000, 0.000000000000000000 ) ) ;
#91601 = ORIENTED_EDGE ( 'NONE', *, *, #30538, .F. ) ;
#91602 = ORIENTED_EDGE ( 'NONE', *, *, #19862, .F. ) ;
#91603 = CARTESIAN_POINT ( 'NONE',  ( 33.13288845015618023, -5.965225279485572685, -0.1650522222209214185 ) ) ;
#91604 = CARTESIAN_POINT ( 'NONE',  ( -101.5937515207030657, -25.10935946579351352, 3.495447590598027787 ) ) ;
#91606 = ADVANCED_FACE ( 'NONE', ( #15949 ), #45926, .T. ) ;
#91605 = CARTESIAN_POINT ( 'NONE',  ( -102.9228709571500957, -23.47593901973090524, -1.443836447538997314 ) ) ;
#91607 = CARTESIAN_POINT ( 'NONE',  ( 12.15263457413992576, -16.39098610538439615, -1.500000000000002220 ) ) ;
#91608 = ORIENTED_EDGE ( 'NONE', *, *, #99905, .F. ) ;
#91609 = CARTESIAN_POINT ( 'NONE',  ( -2.806649551956928335, -6.376774720514411854, 19.35116211686183618 ) ) ;
#91610 = CARTESIAN_POINT ( 'NONE',  ( -30.63234162661936111, -23.86952536761622667, -1.017619990082605952 ) ) ;
#91611 = LINE ( 'NONE', #92113, #52942 ) ;
#91612 = LINE ( 'NONE', #6882, #69111 ) ;
#91613 = ORIENTED_EDGE ( 'NONE', *, *, #52799, .F. ) ;
#91614 = CARTESIAN_POINT ( 'NONE',  ( -28.98875734969026041, -5.965225279485572685, 17.86602280011862476 ) ) ;
#91615 = CARTESIAN_POINT ( 'NONE',  ( -29.74590468580106872, -24.63645583638522751, 6.038517363561788365 ) ) ;
#91616 = VECTOR ( 'NONE', #42807, 1000.000000000000114 ) ;
#91617 = CARTESIAN_POINT ( 'NONE',  ( 17.70469293622815243, 10.90570606759641592, -1.500000000000002220 ) ) ;
#91618 = ORIENTED_EDGE ( 'NONE', *, *, #417, .T. ) ;
#91620 = ORIENTED_EDGE ( 'NONE', *, *, #6075, .T. ) ;
#91619 = CARTESIAN_POINT ( 'NONE',  ( -106.6228709571500559, -24.66019654487199730, 8.947790411086122830 ) ) ;
#91621 = CARTESIAN_POINT ( 'NONE',  ( -28.62287095715005947, -24.18537418825495777, 9.819270430423445717 ) ) ;
#91622 = ORIENTED_EDGE ( 'NONE', *, *, #73868, .T. ) ;
#91623 = VERTEX_POINT ( 'NONE', #23559 ) ;
#91624 = DIRECTION ( 'NONE',  ( 0.000000000000000000, 0.000000000000000000, 1.000000000000000000 ) ) ;
#91625 = CARTESIAN_POINT ( 'NONE',  ( -92.62287095715005592, -24.35013146730204170, 9.818937971375108376 ) ) ;
#91626 = CARTESIAN_POINT ( 'NONE',  ( -60.62287095715004881, -23.47596703998600631, 11.44779298504227505 ) ) ;
#91627 = CARTESIAN_POINT ( 'NONE',  ( -100.5925999562403490, -25.25419553508370285, 7.559861005836696179 ) ) ;
#91628 = DIRECTION ( 'NONE',  ( -7.185047449708836111E-16, -0.000000000000000000, -1.000000000000000000 ) ) ;
#91629 = DIRECTION ( 'NONE',  ( 0.000000000000000000, 0.000000000000000000, 1.000000000000000000 ) ) ;
#91631 = VERTEX_POINT ( 'NONE', #54042 ) ;
#91630 = CARTESIAN_POINT ( 'NONE',  ( 4.260453091581613450, -21.75001586557718980, 11.49999999999999645 ) ) ;
#91632 = DIRECTION ( 'NONE',  ( 0.000000000000000000, 0.000000000000000000, -1.000000000000000000 ) ) ;
#91633 = CARTESIAN_POINT ( 'NONE',  ( 3.867644355387967359, 22.30990608135428488, 11.49999999999998934 ) ) ;
#91635 = ORIENTED_EDGE ( 'NONE', *, *, #56687, .T. ) ;
#91634 = CARTESIAN_POINT ( 'NONE',  ( -20.27875734969026311, -4.776774720514394446, 24.00402280011862288 ) ) ;
#91636 = EDGE_CURVE ( 'NONE', #45450, #64237, #43614, .T. ) ;
#91637 = B_SPLINE_CURVE_WITH_KNOTS ( 'NONE', 3,
 ( #9234, #85869, #70140, #86858, #95481, #32074 ),
 .UNSPECIFIED., .F., .F.,
 ( 4, 2, 4 ),
 ( 0.000000000000000000, 0.001380901958385393315, 0.002761803916770786630 ),
 .UNSPECIFIED. ) ;
#91638 = ORIENTED_EDGE ( 'NONE', *, *, #9576, .F. ) ;
#91639 = CARTESIAN_POINT ( 'NONE',  ( 31.01539214510847486, 4.736880496761964210, -2.146553774717884444 ) ) ;
#91640 = EDGE_CURVE ( 'NONE', #92630, #1389, #76348, .T. ) ;
#91641 = AXIS2_PLACEMENT_3D ( 'NONE', #34828, #96715, #27216 ) ;
#91642 = B_SPLINE_CURVE_WITH_KNOTS ( 'NONE', 3,
 ( #17968, #87476, #48928, #87984 ),
 .UNSPECIFIED., .F., .F.,
 ( 4, 4 ),
 ( 0.7393053958805789749, 0.7403061429213444455 ),
 .UNSPECIFIED. ) ;
#91643 = CARTESIAN_POINT ( 'NONE',  ( 1.915021276000606454, 20.04344799065331628, 11.49999999999998934 ) ) ;
#91644 = LINE ( 'NONE', #58712, #65181 ) ;
#91645 = ORIENTED_EDGE ( 'NONE', *, *, #12466, .F. ) ;
#91646 = DIRECTION ( 'NONE',  ( 0.000000000000000000, 0.000000000000000000, -1.000000000000000000 ) ) ;
#91647 = CARTESIAN_POINT ( 'NONE',  ( 19.44376294880228428, 11.01865886811674677, -1.500000000000002220 ) ) ;
#91648 = VECTOR ( 'NONE', #88425, 1000.000000000000000 ) ;
#91649 = AXIS2_PLACEMENT_3D ( 'NONE', #84669, #23260, #9049 ) ;
#91650 = VERTEX_POINT ( 'NONE', #62152 ) ;
#91651 = ORIENTED_EDGE ( 'NONE', *, *, #9367, .T. ) ;
#91652 = CARTESIAN_POINT ( 'NONE',  ( 16.00000000000000000, 0.000000000000000000, 0.000000000000000000 ) ) ;
#91653 = CARTESIAN_POINT ( 'NONE',  ( -80.93694966678978631, -25.04514726203225550, 7.505594008164218067 ) ) ;
#91654 = CARTESIAN_POINT ( 'NONE',  ( 6.600000000000001421, 0.000000000000000000, 0.000000000000000000 ) ) ;
#91655 = FACE_OUTER_BOUND ( 'NONE', #89102, .T. ) ;
#91656 = AXIS2_PLACEMENT_3D ( 'NONE', #7591, #15202, #84208 ) ;
#91657 = CARTESIAN_POINT ( 'NONE',  ( -25.92875734969025814, 3.316774720514426456, 0.7300228001186309656 ) ) ;
#91658 = CARTESIAN_POINT ( 'NONE',  ( -12.10551386448753064, 15.32171617432465816, 11.49999999999998934 ) ) ;
#91659 = CARTESIAN_POINT ( 'NONE',  ( -47.52287095715004739, -24.34917612407052090, 0.1852690917482640864 ) ) ;
#91660 = CARTESIAN_POINT ( 'NONE',  ( 7.480126432006339421, -20.11416664461015458, -1.500000000000002220 ) ) ;
#91661 = CARTESIAN_POINT ( 'NONE',  ( -2.188401442307694289, -5.876774720514410077, 19.46153846153846700 ) ) ;
#91662 = CARTESIAN_POINT ( 'NONE',  ( -111.5228709571500616, -29.50248528299804818, 1.056150453629043584 ) ) ;
#91663 = CARTESIAN_POINT ( 'NONE',  ( -111.3776484685884185, -25.28710546256126079, 4.332404433089555695 ) ) ;
#91664 = CARTESIAN_POINT ( 'NONE',  ( 9.198035947750891950, -20.93187084735588144, -1.500000000000002220 ) ) ;
#91665 = EDGE_CURVE ( 'NONE', #62568, #21835, #99676, .T. ) ;
#91666 = CARTESIAN_POINT ( 'NONE',  ( -106.6300409130544580, -23.96169478059714564, 10.65365249895717170 ) ) ;
#91667 = DIRECTION ( 'NONE',  ( 0.000000000000000000, 2.173523156925980399E-06, -0.9999999999976378895 ) ) ;
#91668 = CARTESIAN_POINT ( 'NONE',  ( 0.05828707793547563409, -19.95834144014285272, 11.49999999999999645 ) ) ;
#91669 = CARTESIAN_POINT ( 'NONE',  ( -50.52287095715005449, -24.92579138211018019, 1.929029949965659352 ) ) ;
#91670 = PLANE ( 'NONE',  #13291 ) ;
#91671 = CARTESIAN_POINT ( 'NONE',  ( -44.52287095715006160, -23.47593901973090169, -1.443836447538997092 ) ) ;
#91672 = VERTEX_POINT ( 'NONE', #76837 ) ;
#91673 = CARTESIAN_POINT ( 'NONE',  ( -83.52287095715009002, -24.35013146730203815, 9.818937971375104823 ) ) ;
#91674 = CARTESIAN_POINT ( 'NONE',  ( -52.62287095715004170, -23.47596703998600276, 11.44779298504227505 ) ) ;
#91675 = CARTESIAN_POINT ( 'NONE',  ( -16.45766974254678061, 14.19212061201335473, 11.49999999999998934 ) ) ;
#91676 = EDGE_CURVE ( 'NONE', #73818, #42982, #92197, .T. ) ;
#91677 = CYLINDRICAL_SURFACE ( 'NONE', #10738, 3.060000000000000053 ) ;
#91678 = CARTESIAN_POINT ( 'NONE',  ( 3.528372621398383924, 19.26332229581237598, -1.500000000000002220 ) ) ;
#91679 = CARTESIAN_POINT ( 'NONE',  ( -99.96323870662324396, -25.14579874352854816, 7.028128672497866880 ) ) ;
#91680 = ORIENTED_EDGE ( 'NONE', *, *, #9226, .T. ) ;
#91681 = CALENDAR_DATE ( 2026, 9, 10 ) ;
#91682 = DIRECTION ( 'NONE',  ( -0.000000000000000000, 1.000000000000000000, -0.000000000000000000 ) ) ;
#91683 = CARTESIAN_POINT ( 'NONE',  ( 2.933277810221831761, -5.876774720514424288, 21.39432064584807947 ) ) ;
#91684 = CARTESIAN_POINT ( 'NONE',  ( -13.28352777634190396, 15.58691228024164310, 11.49999999999999645 ) ) ;
#91685 = FACE_OUTER_BOUND ( 'NONE', #2974, .T. ) ;
#91687 = B_SPLINE_CURVE_WITH_KNOTS ( 'NONE', 3,
 ( #76866, #23080, #46441, #54071, #32205, #763, #7873, #55062, #86000, #86995, #42352, #49458, #65691, #3288, #41333, #88506 ),
 .UNSPECIFIED., .F., .F.,
 ( 4, 2, 2, 2, 2, 2, 2, 4 ),
 ( -2.132270449955935040E-05, 0.0007770955584725032679, 0.001176304689958539498, 0.001575513821444575729, 0.001974722952930611959, 0.002373932084416648623, 0.002773141215902684420, 0.003172350347388721084 ),
 .UNSPECIFIED. ) ;
#91686 = DIRECTION ( 'NONE',  ( 0.000000000000000000, -0.000000000000000000, -1.000000000000000000 ) ) ;
#91688 = EDGE_LOOP ( 'NONE', ( #91971, #100176 ) ) ;
#91689 = CARTESIAN_POINT ( 'NONE',  ( 31.18725089179298138, -4.540774720514433760, 2.579558749741450718 ) ) ;
#91690 = FACE_OUTER_BOUND ( 'NONE', #63107, .T. ) ;
#91691 = CARTESIAN_POINT ( 'NONE',  ( -69.34303308397305443, -25.25559839591755207, 6.209207386190695566 ) ) ;
#91692 = ADVANCED_FACE ( 'NONE', ( #38294 ), #77345, .T. ) ;
#91693 = CARTESIAN_POINT ( 'NONE',  ( -61.62287095715002749, -23.72747288104441665, -1.053458166803662666 ) ) ;
#91694 = DIRECTION ( 'NONE',  ( 0.000000000000000000, -1.000000000000000000, 0.000000000000000000 ) ) ;
#91695 = VECTOR ( 'NONE', #84568, 1000.000000000000114 ) ;
#91696 = CARTESIAN_POINT ( 'NONE',  ( -5.126879528927636542, -22.49243673399587351, 11.49999999999999645 ) ) ;
#91697 = CARTESIAN_POINT ( 'NONE',  ( 20.43669262517703800, -10.12641136740851699, 11.49999999999998934 ) ) ;
#91698 = CARTESIAN_POINT ( 'NONE',  ( 10.54059822343757702, -6.376774720514426953, 17.17691942396159988 ) ) ;
#91699 = CARTESIAN_POINT ( 'NONE',  ( -28.62287095715004881, -24.49608681932686949, 1.056161686216224860 ) ) ;
#91700 = CARTESIAN_POINT ( 'NONE',  ( -63.92287095715007439, -23.47593901973090524, -1.443836447538998202 ) ) ;
#91701 = DIRECTION ( 'NONE',  ( 1.000000000000000000, 3.773278334444166432E-23, 8.201307841325785021E-29 ) ) ;
#91702 = CARTESIAN_POINT ( 'NONE',  ( -110.5895385589013955, -24.52300882791530512, 0.6510814631126382590 ) ) ;
#91703 = CARTESIAN_POINT ( 'NONE',  ( 20.64021973274467570, 7.317367941133321452, 11.49999999999998934 ) ) ;
#91704 = EDGE_CURVE ( 'NONE', #69556, #15899, #97132, .T. ) ;
#91705 = CARTESIAN_POINT ( 'NONE',  ( -43.62287095715004881, -24.65952944569304606, 1.056160979905692576 ) ) ;
#91706 = AXIS2_PLACEMENT_3D ( 'NONE', #36317, #59666, #67277 ) ;
#91707 = CARTESIAN_POINT ( 'NONE',  ( -50.62287095715006302, -24.63287334234178871, 0.9662140553045418523 ) ) ;
#91708 = DIRECTION ( 'NONE',  ( -1.000000000000000000, 0.000000000000000000, 0.000000000000000000 ) ) ;
#91709 = EDGE_CURVE ( 'NONE', #96497, #5853, #93075, .T. ) ;
#91710 = CARTESIAN_POINT ( 'NONE',  ( -28.98875734969026396, -3.316774720514426456, -0.08597719988137648983 ) ) ;
#91711 = LINE ( 'NONE', #37936, #93822 ) ;
#91712 = DIRECTION ( 'NONE',  ( -0.000000000000000000, 2.173523156925979552E-06, -0.9999999999976378895 ) ) ;
#91713 = EDGE_LOOP ( 'NONE', ( #18892, #81381, #44712, #91037 ) ) ;
#91714 = AXIS2_PLACEMENT_3D ( 'NONE', #61958, #23363, #70058 ) ;
#91715 = CARTESIAN_POINT ( 'NONE',  ( 5.749347661499963458, 19.61174949527739386, -1.500000000000002220 ) ) ;
#91716 = ORIENTED_EDGE ( 'NONE', *, *, #63941, .F. ) ;
#91717 = AXIS2_PLACEMENT_3D ( 'NONE', #49010, #80949, #79942 ) ;
#91718 = VERTEX_POINT ( 'NONE', #16957 ) ;
#91719 = ORIENTED_EDGE ( 'NONE', *, *, #6148, .F. ) ;
#91720 = VERTEX_POINT ( 'NONE', #87983 ) ;
#91721 = CARTESIAN_POINT ( 'NONE',  ( -3.733506833432379768, 22.73668382284982314, -1.500000000000002220 ) ) ;
#91723 = EDGE_CURVE ( 'NONE', #88666, #22199, #17544, .T. ) ;
#91722 = CARTESIAN_POINT ( 'NONE',  ( 29.68479148105951992, 1.682774720514426114, -9.431263391055118461 ) ) ;
#91724 = CARTESIAN_POINT ( 'NONE',  ( 8.375906630400100639, -18.44307005126401933, -1.500000000000002220 ) ) ;
#91725 = AXIS2_PLACEMENT_3D ( 'NONE', #71710, #64119, #25529 ) ;
#91726 = ORIENTED_EDGE ( 'NONE', *, *, #25014, .T. ) ;
#91727 = CARTESIAN_POINT ( 'NONE',  ( -29.26545924526617881, -25.19927926512142591, 4.027978703335532096 ) ) ;
#91728 = CARTESIAN_POINT ( 'NONE',  ( -87.62287095715011276, -24.35013146730204525, 9.818937971375108376 ) ) ;
#91729 = AXIS2_PLACEMENT_3D ( 'NONE', #40796, #77836, #48924 ) ;
#91730 = ADVANCED_FACE ( 'NONE', ( #734 ), #95588, .F. ) ;
#91731 = CARTESIAN_POINT ( 'NONE',  ( -51.62287095715005592, -24.64965695001468404, 8.947790433994185832 ) ) ;
#91732 = CARTESIAN_POINT ( 'NONE',  ( -70.64339238044932756, -24.15503026093916006, -0.2815557561904372674 ) ) ;
#91734 = ORIENTED_EDGE ( 'NONE', *, *, #42286, .T. ) ;
#91733 = CARTESIAN_POINT ( 'NONE',  ( 21.23773461148298836, -3.020459416520930862, 11.49999999999999645 ) ) ;
#91735 = DIRECTION ( 'NONE',  ( -3.773278334453079030E-23, 0.9999999999976377785, 2.173523156925979128E-06 ) ) ;
#91736 = CARTESIAN_POINT ( 'NONE',  ( -61.64238508986091603, -23.96169478059713143, 10.65365249895718591 ) ) ;
#91737 = ORIENTED_EDGE ( 'NONE', *, *, #38383, .T. ) ;
#91738 = CARTESIAN_POINT ( 'NONE',  ( -6.500255983836059848, -19.66680810221124887, -1.500000000000002220 ) ) ;
#91740 = ORIENTED_EDGE ( 'NONE', *, *, #53796, .F. ) ;
#91739 = DIRECTION ( 'NONE',  ( 0.000000000000000000, 0.000000000000000000, 1.000000000000000000 ) ) ;
#91741 = CARTESIAN_POINT ( 'NONE',  ( -29.49875734969026198, -0.3587747205144265483, 2.362022800118626531 ) ) ;
#91742 = VERTEX_POINT ( 'NONE', #47921 ) ;
#91743 = CARTESIAN_POINT ( 'NONE',  ( 4.967620699791259753, -5.876774720514413630, 19.94530485585548973 ) ) ;
#91744 = ORIENTED_EDGE ( 'NONE', *, *, #32145, .F. ) ;
#91745 = B_SPLINE_CURVE_WITH_KNOTS ( 'NONE', 3,
 ( #38973, #41361, #77026, #412, #39482, #920, #31872, #50472, #35750, #73314, #59591, #36247, #35252, #90029, #74304, #3810, #58100, #12394, #20501 ),
 .UNSPECIFIED., .F., .F.,
 ( 4, 1, 1, 1, 1, 1, 1, 1, 1, 1, 1, 1, 1, 1, 1, 1, 4 ),
 ( 0.000000000000000000, 0.07059928943359200515, 0.1379009210036200861, 0.2031961978097334975, 0.2667897246502631270, 0.3291063872214231578, 0.3906535452348600668, 0.4526530569344815458, 0.5157480403003722458, 0.5779263408004527980, 0.6389300116184465361, 0.6983507176418213280, 0.7572960374442707643, 0.8163937673501530101, 0.8762669096141296743, 0.9368171089060820522, 1.000000000000000000 ),
 .UNSPECIFIED. ) ;
#91746 = CARTESIAN_POINT ( 'NONE',  ( 0.1985894851802381678, 21.93841921393417849, 11.49999999999999645 ) ) ;
#91747 = CARTESIAN_POINT ( 'NONE',  ( -37.64896865082437216, -23.96169478059712432, 10.65365249895718591 ) ) ;
#91748 = CARTESIAN_POINT ( 'NONE',  ( 22.54279463279464579, 0.6884863543687869125, 11.49999999999998934 ) ) ;
#91749 = VECTOR ( 'NONE', #31229, 1000.000000000000000 ) ;
#91750 = CARTESIAN_POINT ( 'NONE',  ( -18.08314111433443827, -10.61732331186343004, -1.500000000000002220 ) ) ;
#91751 = CARTESIAN_POINT ( 'NONE',  ( -108.9545715455114987, -25.28708312187852414, 4.170144817753115518 ) ) ;
#91752 = CARTESIAN_POINT ( 'NONE',  ( -53.52287095715006870, -23.48786465467241058, 11.44779295918255002 ) ) ;
#91753 = VERTEX_POINT ( 'NONE', #39795 ) ;
#91754 = ORIENTED_EDGE ( 'NONE', *, *, #98073, .T. ) ;
#91755 = ORIENTED_EDGE ( 'NONE', *, *, #6045, .F. ) ;
#91756 = CARTESIAN_POINT ( 'NONE',  ( -66.64657122283996671, -23.73766607897669800, -1.055555164236460897 ) ) ;
#91757 = CARTESIAN_POINT ( 'NONE',  ( 18.51311748589099082, 11.02308708543723270, -1.500000000000002220 ) ) ;
#91758 = ADVANCED_FACE ( 'NONE', ( #70753 ), #79354, .T. ) ;
#91759 = CARTESIAN_POINT ( 'NONE',  ( 0.3910256410256418014, -5.876774720514418959, 20.67377804487179915 ) ) ;
#91760 = ORIENTED_EDGE ( 'NONE', *, *, #23112, .T. ) ;
#91761 = CARTESIAN_POINT ( 'NONE',  ( -2.902382693073098707, -20.91247731031871382, -1.500000000000002220 ) ) ;
#91762 = CARTESIAN_POINT ( 'NONE',  ( -126.6228709571499991, -23.96127896941632685, -0.6493128931037731588 ) ) ;
#91763 = DIRECTION ( 'NONE',  ( 0.000000000000000000, 0.000000000000000000, 1.000000000000000000 ) ) ;
#91764 = CARTESIAN_POINT ( 'NONE',  ( -100.5228709571500332, -24.15431212366390668, -0.2830839119429366946 ) ) ;
#91765 = FACE_OUTER_BOUND ( 'NONE', #45662, .T. ) ;
#91766 = DIRECTION ( 'NONE',  ( 1.000000000000000000, 2.567145104884906770E-18, 5.579749332669698856E-24 ) ) ;
#91767 = CARTESIAN_POINT ( 'NONE',  ( -12.04397493737346991, 18.63154960201688226, -1.500000000000002220 ) ) ;
#91768 = CARTESIAN_POINT ( 'NONE',  ( -71.58791429090274505, -24.34968618360933945, 0.1864209137778822800 ) ) ;
#91769 = ORIENTED_EDGE ( 'NONE', *, *, #58309, .F. ) ;
#91770 = CARTESIAN_POINT ( 'NONE',  ( -82.52287095715006160, -23.47596703998600631, 11.44779298504228571 ) ) ;
#91771 = CARTESIAN_POINT ( 'NONE',  ( -33.62287095715005592, -23.47593901973091235, -1.443836447539013301 ) ) ;
#91772 = DIRECTION ( 'NONE',  ( 0.000000000000000000, 0.000000000000000000, -1.000000000000000000 ) ) ;
#91773 = AXIS2_PLACEMENT_3D ( 'NONE', #63751, #9426, #71846 ) ;
#91774 = LINE ( 'NONE', #6050, #88480 ) ;
#91775 = CARTESIAN_POINT ( 'NONE',  ( -17.86923650574433609, -7.721772263035739492, 11.49999999999998934 ) ) ;
#91776 = CARTESIAN_POINT ( 'NONE',  ( -11.99125074976391048, 17.70416384622758343, -1.500000000000002220 ) ) ;
#91777 = CARTESIAN_POINT ( 'NONE',  ( -62.56626437149660802, -23.48783264082476308, -1.443836473390090580 ) ) ;
#91778 = B_SPLINE_CURVE_WITH_KNOTS ( 'NONE', 3,
 ( #48355, #80800, #34630, #86900, #65599, #17898, #27011, #88916 ),
 .UNSPECIFIED., .F., .F.,
 ( 4, 2, 2, 4 ),
 ( -0.001224873891641428247, -0.0002244903592271104472, 0.0007758931731872069186, 0.002776660238015841217 ),
 .UNSPECIFIED. ) ;
#91779 = CARTESIAN_POINT ( 'NONE',  ( -106.5228709571500332, -23.48783264082477018, -1.443836473390085695 ) ) ;
#91780 = B_SPLINE_CURVE_WITH_KNOTS ( 'NONE', 3,
 ( #94295, #1970, #48145, #9566 ),
 .UNSPECIFIED., .F., .F.,
 ( 4, 4 ),
 ( 0.3400287306710966240, 0.3490351619432120467 ),
 .UNSPECIFIED. ) ;
#91781 = CARTESIAN_POINT ( 'NONE',  ( -123.5228709571500474, -23.94994826722565406, -0.6494450866342700301 ) ) ;
#91782 = DIRECTION ( 'NONE',  ( -3.773278334453079030E-23, 0.9999999999976377785, 2.173523156925979128E-06 ) ) ;
#91783 = CARTESIAN_POINT ( 'NONE',  ( -12.01393383709116947, -19.22582291892495121, -1.500000000000002220 ) ) ;
#91784 = VECTOR ( 'NONE', #64514, 1000.000000000000114 ) ;
#91785 = EDGE_CURVE ( 'NONE', #38852, #16349, #43088, .T. ) ;
#91786 = ORIENTED_EDGE ( 'NONE', *, *, #45422, .F. ) ;
#91787 = AXIS2_PLACEMENT_3D ( 'NONE', #15724, #93341, #23324 ) ;
#91788 = DIRECTION ( 'NONE',  ( -3.773278334453079618E-23, 0.9999999999976377785, 2.173523156925979975E-06 ) ) ;
#91789 = FACE_OUTER_BOUND ( 'NONE', #66310, .T. ) ;
#91790 = CARTESIAN_POINT ( 'NONE',  ( -18.99895575154661742, -5.639348582513488140, 11.49999999999999645 ) ) ;
#91791 = AXIS2_PLACEMENT_3D ( 'NONE', #31586, #69661, #100071 ) ;
#91792 = EDGE_CURVE ( 'NONE', #51194, #11608, #32179, .T. ) ;
#91793 = DIRECTION ( 'NONE',  ( -1.000000000000000000, -3.773278334444166432E-23, -8.201307841325785021E-29 ) ) ;
#91794 = ORIENTED_EDGE ( 'NONE', *, *, #8182, .T. ) ;
#91795 = CARTESIAN_POINT ( 'NONE',  ( -68.62287095715004170, -24.66019654487199020, 8.947790411086131712 ) ) ;
#91797 = EDGE_CURVE ( 'NONE', #94885, #12627, #86555, .T. ) ;
#91796 = DIRECTION ( 'NONE',  ( -3.773278334453079618E-23, 0.9999999999976377785, 2.173523156925979975E-06 ) ) ;
#91798 = CARTESIAN_POINT ( 'NONE',  ( -10.14273968512601520, 19.10955606681249463, 11.49999999999998934 ) ) ;
#91799 = EDGE_CURVE ( 'NONE', #95525, #96621, #70251, .T. ) ;
#91800 = CARTESIAN_POINT ( 'NONE',  ( -49.59577668750772972, -25.10935179600810230, 3.074246299446597774 ) ) ;
#91802 = AXIS2_PLACEMENT_3D ( 'NONE', #5347, #44420, #44920 ) ;
#91801 = CARTESIAN_POINT ( 'NONE',  ( 11.34002819025610087, 15.78594478779102950, -1.500000000000002220 ) ) ;
#91803 = SHAPE_REPRESENTATION ( 'Hook Pin_Varsay\X2\0131\X0\lan', ( #37391 ), #19636 ) ;
#91804 = EDGE_CURVE ( 'NONE', #14758, #5846, #99834, .T. ) ;
#91805 = CARTESIAN_POINT ( 'NONE',  ( -82.52287095715004739, -24.35013146730204525, 9.818937971375101270 ) ) ;
#91806 = CARTESIAN_POINT ( 'NONE',  ( 5.550000000000004263, -2.000000000000001776, 24.00000000000000000 ) ) ;
#91807 = CARTESIAN_POINT ( 'NONE',  ( 18.95923836289803788, 5.684714004613049987, -1.500000000000002220 ) ) ;
#91808 = ORIENTED_EDGE ( 'NONE', *, *, #82881, .F. ) ;
#91809 = EDGE_CURVE ( 'NONE', #908, #44968, #62654, .T. ) ;
#91810 = CARTESIAN_POINT ( 'NONE',  ( 11.02309159617336221, -17.05227643984133934, 11.49999999999999645 ) ) ;
#91811 = CARTESIAN_POINT ( 'NONE',  ( -80.60234417792803185, -23.85016227208580020, -0.8807180028928338622 ) ) ;
#91812 = FACE_OUTER_BOUND ( 'NONE', #1408, .T. ) ;
#91813 = ORIENTED_EDGE ( 'NONE', *, *, #48878, .T. ) ;
#91814 = CARTESIAN_POINT ( 'NONE',  ( -102.5221944888360497, -23.48786465467241058, 11.44779295918254292 ) ) ;
#91815 = CARTESIAN_POINT ( 'NONE',  ( -119.4728709594060376, -25.40676080801054937, 8.000950335809053016 ) ) ;
#91816 = CARTESIAN_POINT ( 'NONE',  ( -96.62287095715005592, -24.50321055353805377, 9.387540953477525818 ) ) ;
#91817 = CARTESIAN_POINT ( 'NONE',  ( -40.65333657091576924, -24.15602025860895097, 10.28564288303536856 ) ) ;
#91818 = CARTESIAN_POINT ( 'NONE',  ( -108.5228709571500616, -29.50248528299804818, 1.056150453629043584 ) ) ;
#91819 = CARTESIAN_POINT ( 'NONE',  ( -16.95507112718987486, -10.73317591066004084, 11.49999999999998934 ) ) ;
#91820 = EDGE_CURVE ( 'NONE', #65974, #50219, #7962, .T. ) ;
#91821 = EDGE_CURVE ( 'NONE', #99101, #84023, #74522, .T. ) ;
#91822 = CARTESIAN_POINT ( 'NONE',  ( -27.96875734969026084, -6.475225279485573360, 26.43402280011862615 ) ) ;
#91823 = ORIENTED_EDGE ( 'NONE', *, *, #34556, .T. ) ;
#91824 = CARTESIAN_POINT ( 'NONE',  ( -129.6228709571500417, -23.47593901973091235, -1.443836447538995760 ) ) ;
#91825 = AXIS2_PLACEMENT_3D ( 'NONE', #76001, #85624, #22209 ) ;
#91826 = CARTESIAN_POINT ( 'NONE',  ( 22.81499323874321661, -2.031749852351878882, 11.49999999999999645 ) ) ;
#91827 = CARTESIAN_POINT ( 'NONE',  ( 4.564784964189898098, -22.25151590922551748, -1.500000000000002220 ) ) ;
#91828 = DIRECTION ( 'NONE',  ( 0.000000000000000000, -1.000000000000000000, 0.000000000000000000 ) ) ;
#91829 = DIRECTION ( 'NONE',  ( 0.000000000000000000, -0.000000000000000000, -1.000000000000000000 ) ) ;
#91830 = CARTESIAN_POINT ( 'NONE',  ( -38.64173386164763713, -24.15620529776627379, 10.23563542870660825 ) ) ;
#91831 = AXIS2_PLACEMENT_3D ( 'NONE', #95654, #80927, #34261 ) ;
#91832 = CARTESIAN_POINT ( 'NONE',  ( -43.55620429048340014, -24.64965694238574656, 8.947790433994203596 ) ) ;
#91833 = EDGE_CURVE ( 'NONE', #56809, #82122, #32682, .T. ) ;
#91834 = CARTESIAN_POINT ( 'NONE',  ( -32.22287095715005023, -23.47593901973090169, -1.443836447538997980 ) ) ;
#91835 = CARTESIAN_POINT ( 'NONE',  ( 22.65031661608482594, 1.684774720501991618, -20.71116937900383448 ) ) ;
#91836 = ORIENTED_EDGE ( 'NONE', *, *, #21970, .F. ) ;
#91837 = CARTESIAN_POINT ( 'NONE',  ( -20.10423522397153562, 3.301153050299447056, -1.500000000000002220 ) ) ;
#91838 = ORIENTED_EDGE ( 'NONE', *, *, #10382, .T. ) ;
#91839 = CARTESIAN_POINT ( 'NONE',  ( 14.22603995551189371, 18.00578905361294346, 11.49999999999998934 ) ) ;
#91840 = EDGE_CURVE ( 'NONE', #23326, #95426, #25574, .T. ) ;
#91841 = CARTESIAN_POINT ( 'NONE',  ( -53.52287095715006160, -23.73934037231757088, 11.05740245334329153 ) ) ;
#91842 = ORIENTED_EDGE ( 'NONE', *, *, #25952, .T. ) ;
#91843 = CARTESIAN_POINT ( 'NONE',  ( -108.5907114367411879, -24.15620529776629155, 10.23563542870659404 ) ) ;
#91844 = TOROIDAL_SURFACE ( 'NONE', #77200, 253.2618649670780826, 1.835999999999999854 ) ;
#91845 = ADVANCED_FACE ( 'NONE', ( #71254 ), #41306, .T. ) ;
#91846 = CARTESIAN_POINT ( 'NONE',  ( -77.62997961999919028, -24.35071581493544102, 9.817618358456021710 ) ) ;
#91847 = EDGE_CURVE ( 'NONE', #64651, #9578, #14472, .T. ) ;
#91848 = CARTESIAN_POINT ( 'NONE',  ( -51.63317546500711330, -24.35071581493543036, 9.817618358456028815 ) ) ;
#91850 = VERTEX_POINT ( 'NONE', #42817 ) ;
#91849 = CARTESIAN_POINT ( 'NONE',  ( -1.624102159174229731, 21.17438964843747584, 11.49999999999999645 ) ) ;
#91851 = ORIENTED_EDGE ( 'NONE', *, *, #4906, .F. ) ;
#91852 = CARTESIAN_POINT ( 'NONE',  ( 17.07819277939130842, -14.19623557145530057, 11.49999999999998934 ) ) ;
#91853 = CARTESIAN_POINT ( 'NONE',  ( -16.41017380093149214, -12.48182641202616416, -1.500000000000002220 ) ) ;
#91854 = ORIENTED_EDGE ( 'NONE', *, *, #62012, .F. ) ;
#91855 = ORIENTED_EDGE ( 'NONE', *, *, #11907, .F. ) ;
#91856 = CARTESIAN_POINT ( 'NONE',  ( 22.02124265030973760, -6.143225279485574397, 16.20402280011862217 ) ) ;
#91857 = ADVANCED_FACE ( 'NONE', ( #58535 ), #42327, .F. ) ;
#91858 = CARTESIAN_POINT ( 'NONE',  ( -39.04644334225289271, -25.28415765582125729, 4.123731396711104225 ) ) ;
#91859 = ORIENTED_EDGE ( 'NONE', *, *, #21145, .F. ) ;
#91860 = VECTOR ( 'NONE', #78750, 1000.000000000000000 ) ;
#91861 = CARTESIAN_POINT ( 'NONE',  ( -91.63120794989035289, -24.15543982623907837, -0.2315651400026614848 ) ) ;
#91862 = AXIS2_PLACEMENT_3D ( 'NONE', #74663, #60466, #97008 ) ;
#91863 = ORIENTED_EDGE ( 'NONE', *, *, #21288, .T. ) ;
#91864 = CARTESIAN_POINT ( 'NONE',  ( 30.57258140252915979, 5.759614247572967471, 25.39586761113762137 ) ) ;
#91865 = LINE ( 'NONE', #22336, #34139 ) ;
#91866 = CARTESIAN_POINT ( 'NONE',  ( 20.57277012135545036, 3.371850554975475145, -1.500000000000002220 ) ) ;
#91867 = CARTESIAN_POINT ( 'NONE',  ( 18.19902423439809525, 11.99547645517801442, 11.49999999999999645 ) ) ;
#91868 = DIRECTION ( 'NONE',  ( -1.000000000000000000, 9.637352644315600173E-17, 0.000000000000000000 ) ) ;
#91869 = FACE_OUTER_BOUND ( 'NONE', #65931, .T. ) ;
#91870 = CARTESIAN_POINT ( 'NONE',  ( 15.63351008929417318, -16.12541905121107177, 11.49999999999998934 ) ) ;
#91871 = FACE_OUTER_BOUND ( 'NONE', #15677, .T. ) ;
#91872 = ORIENTED_EDGE ( 'NONE', *, *, #84034, .F. ) ;
#91873 = CARTESIAN_POINT ( 'NONE',  ( 26.37445894957760828, -1.477225279485574028, -11.69480419648520986 ) ) ;
#91874 = CARTESIAN_POINT ( 'NONE',  ( -29.49875734969025842, 0.3587747205144265483, 25.61802280011862720 ) ) ;
#91875 = VERTEX_POINT ( 'NONE', #36191 ) ;
#91876 = ORIENTED_EDGE ( 'NONE', *, *, #43413, .F. ) ;
#91877 = CARTESIAN_POINT ( 'NONE',  ( -46.52204127861840277, -23.48786465467240703, 11.44779295918255180 ) ) ;
#91878 = EDGE_LOOP ( 'NONE', ( #78239, #13970, #57070, #40217 ) ) ;
#91879 = CARTESIAN_POINT ( 'NONE',  ( 18.88549913130557556, 9.949676122998861061, -1.500000000000002220 ) ) ;
#91880 = EDGE_LOOP ( 'NONE', ( #81885, #36483, #43784, #5304 ) ) ;
#91881 = CARTESIAN_POINT ( 'NONE',  ( -6.845587600281468177, 19.88882266644084496, -1.500000000000002220 ) ) ;
#91882 = DIRECTION ( 'NONE',  ( -3.773278334444167608E-23, 1.000000000000000000, 0.000000000000000000 ) ) ;
#91883 = CARTESIAN_POINT ( 'NONE',  ( -100.2189343329491464, -25.18669221479178333, 3.306178502990604340 ) ) ;
#91884 = CARTESIAN_POINT ( 'NONE',  ( 8.219458839706481612, -3.316774720514422015, -27.11006393991256758 ) ) ;
#91885 = CARTESIAN_POINT ( 'NONE',  ( -15.43752342082821905, -15.63289427301443801, -1.500000000000002220 ) ) ;
#91886 = CARTESIAN_POINT ( 'NONE',  ( -87.51796580416235827, -23.73766607897671932, -1.055555164236430032 ) ) ;
#91887 = ORIENTED_EDGE ( 'NONE', *, *, #78875, .F. ) ;
#91888 = CARTESIAN_POINT ( 'NONE',  ( -80.52287095715006160, -29.50248528299804818, 1.056150453629038477 ) ) ;
#91889 = VECTOR ( 'NONE', #65462, 1000.000000000000000 ) ;
#91890 = CARTESIAN_POINT ( 'NONE',  ( -84.58538098145766071, -24.51419770103157347, 9.386484678747175181 ) ) ;
#91891 = B_SPLINE_CURVE_WITH_KNOTS ( 'NONE', 3,
 ( #13057, #75449, #37415, #66875, #99774, #99293 ),
 .UNSPECIFIED., .F., .F.,
 ( 4, 2, 4 ),
 ( 6.384118694783952546E-06, 0.001386860460836456845, 0.002767336802978129749 ),
 .UNSPECIFIED. ) ;
#91892 = CARTESIAN_POINT ( 'NONE',  ( -128.5228709571501611, -24.34917612407044629, 0.1852690917480327160 ) ) ;
#91893 = VECTOR ( 'NONE', #26658, 1000.000000000000114 ) ;
#91894 = CARTESIAN_POINT ( 'NONE',  ( -10.25843596179259265, -22.80680519657271788, 9.703205396196688426 ) ) ;
#91895 = CARTESIAN_POINT ( 'NONE',  ( 7.794017451908327843, -19.83292067980804774, 11.49999999999998934 ) ) ;
#91896 = CARTESIAN_POINT ( 'NONE',  ( -98.63812701921389703, -23.48786465467241058, 11.44779295918254114 ) ) ;
#91897 = CARTESIAN_POINT ( 'NONE',  ( -107.5944981716039024, -23.73791477778912196, 11.05961554403169700 ) ) ;
#91898 = CARTESIAN_POINT ( 'NONE',  ( 14.43441819135840376, -3.316774720514426456, -28.36222020317694970 ) ) ;
#91899 = CARTESIAN_POINT ( 'NONE',  ( -33.62923966249122287, -24.51314013834315375, 0.6176544820404119562 ) ) ;
#91900 = CARTESIAN_POINT ( 'NONE',  ( -18.88510386880526326, 12.19974334031638641, -1.500000000000002220 ) ) ;
#91901 = EDGE_CURVE ( 'NONE', #85237, #53220, #88984, .T. ) ;
#91902 = B_SPLINE_SURFACE_WITH_KNOTS ( 'NONE', 3, 1, ( 
 ( #10661, #27876 ),
 ( #72075, #26882 ),
 ( #4555, #73070 ),
 ( #41621, #34500 ),
 ( #27385, #97391 ),
 ( #25883, #18759 ),
 ( #11153, #57852 ) ),
 .UNSPECIFIED., .F., .F., .F.,
 ( 4, 1, 1, 1, 4 ),
 ( 2, 2 ),
 ( 0.000000000000000000, 0.2193543708254379609, 0.4566051594240264633, 0.7164051918613062453, 1.000000000000000000 ),
 ( 0.000000000000000000, 1.000000000000000000 ),
 .UNSPECIFIED. ) ;
#91903 = DIRECTION ( 'NONE',  ( 0.000000000000000000, 2.173523156925980399E-06, -0.9999999999976378895 ) ) ;
#91904 = ORIENTED_EDGE ( 'NONE', *, *, #45911, .F. ) ;
#91905 = EDGE_CURVE ( 'NONE', #11783, #21736, #33364, .T. ) ;
#91906 = PLANE ( 'NONE',  #54717 ) ;
#91907 = CARTESIAN_POINT ( 'NONE',  ( 0.9049686737998731134, -19.58615294826029540, 11.49999999999999645 ) ) ;
#91908 = CARTESIAN_POINT ( 'NONE',  ( -72.62287095715005592, -29.50250786944525672, 11.44777988621623699 ) ) ;
#91909 = EDGE_CURVE ( 'NONE', #52078, #62568, #56396, .T. ) ;
#91910 = DIRECTION ( 'NONE',  ( -3.773278334444167608E-23, 1.000000000000000000, 0.000000000000000000 ) ) ;
#91911 = EDGE_LOOP ( 'NONE', ( #50448, #53296, #10818, #45344 ) ) ;
#91912 = EDGE_CURVE ( 'NONE', #98224, #73156, #90158, .T. ) ;
#91913 = CARTESIAN_POINT ( 'NONE',  ( -50.62287095715004170, -23.48783264082478084, -1.443836473390070596 ) ) ;
#91914 = CARTESIAN_POINT ( 'NONE',  ( -124.6623029623788312, -25.38371629874578161, 5.756521249355254000 ) ) ;
#91915 = CARTESIAN_POINT ( 'NONE',  ( -100.6814946224345846, -25.25095776846604068, 5.197789127044065260 ) ) ;
#91916 = EDGE_CURVE ( 'NONE', #59954, #11920, #87829, .T. ) ;
#91917 = VECTOR ( 'NONE', #81060, 1000.000000000000000 ) ;
#91918 = FACE_OUTER_BOUND ( 'NONE', #95034, .T. ) ;
#91919 = EDGE_CURVE ( 'NONE', #59914, #76224, #96274, .T. ) ;
#91920 = B_SPLINE_CURVE_WITH_KNOTS ( 'NONE', 3,
 ( #43761, #15678, #19908, #67113, #5189, #29021, #59993, #82313 ),
 .UNSPECIFIED., .F., .F.,
 ( 4, 2, 2, 4 ),
 ( 0.000000000000000000, 0.002001079623178219757, 0.003001619434767328985, 0.004002159246356438646 ),
 .UNSPECIFIED. ) ;
#91921 = CARTESIAN_POINT ( 'NONE',  ( -6.535591236171724105, 18.61618873491671877, -1.500000000000002220 ) ) ;
#91922 = ORIENTED_EDGE ( 'NONE', *, *, #68747, .F. ) ;
#91923 = CARTESIAN_POINT ( 'NONE',  ( -109.3646889549745111, -25.28083575590260068, 4.081544306722298288 ) ) ;
#91924 = DIRECTION ( 'NONE',  ( 0.000000000000000000, -0.000000000000000000, -1.000000000000000000 ) ) ;
#91925 = VECTOR ( 'NONE', #82504, 1000.000000000000114 ) ;
#91926 = DATE_AND_TIME ( #7184, #86270 ) ;
#91927 = B_SPLINE_CURVE_WITH_KNOTS ( 'NONE', 3,
 ( #66866, #52129, #13546, #44515 ),
 .UNSPECIFIED., .F., .F.,
 ( 4, 4 ),
 ( 0.000000000000000000, 9.999999999998897304E-05 ),
 .UNSPECIFIED. ) ;
#91928 = ORIENTED_EDGE ( 'NONE', *, *, #63421, .T. ) ;
#91929 = CARTESIAN_POINT ( 'NONE',  ( -49.62287095715005592, -29.50250243563736774, 8.947779886222146928 ) ) ;
#91930 = CARTESIAN_POINT ( 'NONE',  ( -103.6228709571500843, -24.35013146730204525, 9.818937971375111928 ) ) ;
#91931 = CARTESIAN_POINT ( 'NONE',  ( -55.54397260187641194, -24.40034930558990922, 0.3402023900116048494 ) ) ;
#91932 = CARTESIAN_POINT ( 'NONE',  ( -98.89534031563961491, -25.03144876920082496, 6.173963160515893556 ) ) ;
#91933 = CARTESIAN_POINT ( 'NONE',  ( -1.345681049247692940, -5.876774720514410077, 19.69174559449348294 ) ) ;
#91934 = AXIS2_PLACEMENT_3D ( 'NONE', #68198, #43377, #99128 ) ;
#91935 = FACE_OUTER_BOUND ( 'NONE', #33253, .T. ) ;
#91936 = B_SPLINE_CURVE_WITH_KNOTS ( 'NONE', 3,
 ( #70161, #32597, #31593, #63574, #48842, #24978, #40716, #2169 ),
 .UNSPECIFIED., .F., .F.,
 ( 4, 2, 2, 4 ),
 ( -0.001224554619866335221, -0.0002241820295893557757, 0.0007761905606876236697, 0.002776935741241578874 ),
 .UNSPECIFIED. ) ;
#91937 = CARTESIAN_POINT ( 'NONE',  ( -107.6317610820995725, -23.73766607897672642, -1.055555164236427590 ) ) ;
#91938 = CARTESIAN_POINT ( 'NONE',  ( -11.50144725928494438, 16.33591932373696665, -1.500000000000002220 ) ) ;
#91939 = EDGE_CURVE ( 'NONE', #15956, #14129, #22370, .T. ) ;
#91940 = CARTESIAN_POINT ( 'NONE',  ( -125.6228709571500559, -24.15516710230296482, 10.28746687063724607 ) ) ;
#91941 = CARTESIAN_POINT ( 'NONE',  ( -45.47188313039849561, -25.00182538069146787, 7.747789668545044250 ) ) ;
#91942 = EDGE_LOOP ( 'NONE', ( #38318, #19727, #43393, #52525 ) ) ;
#91943 = EDGE_CURVE ( 'NONE', #17321, #31540, #13830, .T. ) ;
#91944 = CARTESIAN_POINT ( 'NONE',  ( 7.155387812436688755, -5.321161431766062044, -25.57627477809911198 ) ) ;
#91945 = CARTESIAN_POINT ( 'NONE',  ( -80.58514661375853905, -24.73531770709095312, 8.716586749053508498 ) ) ;
#91946 = CARTESIAN_POINT ( 'NONE',  ( -58.52287095715006870, -24.51387760970724372, 9.387446482453404073 ) ) ;
#91947 = CARTESIAN_POINT ( 'NONE',  ( -81.51736575286189179, -23.73766607897671221, -1.055555164236432919 ) ) ;
#91948 = FACE_OUTER_BOUND ( 'NONE', #84665, .T. ) ;
#91949 = CARTESIAN_POINT ( 'NONE',  ( -51.19681519762799127, -25.31574444707050731, 4.857314373449191258 ) ) ;
#91950 = CARTESIAN_POINT ( 'NONE',  ( -118.6228709571500559, -29.50247984919015209, -1.443849546365046699 ) ) ;
#91951 = FACE_OUTER_BOUND ( 'NONE', #68912, .T. ) ;
#91952 = ORIENTED_EDGE ( 'NONE', *, *, #51179, .F. ) ;
#91953 = CARTESIAN_POINT ( 'NONE',  ( -19.72078065558051208, -4.686549088087978099, -1.500000000000002220 ) ) ;
#91954 = CARTESIAN_POINT ( 'NONE',  ( -77.52287095715006160, -23.47596703998600631, 11.44779298504228571 ) ) ;
#91955 = LINE ( 'NONE', #13826, #1544 ) ;
#91956 = AXIS2_PLACEMENT_3D ( 'NONE', #86780, #48234, #17272 ) ;
#91957 = PLANE ( 'NONE',  #26562 ) ;
#91959 = ORIENTED_EDGE ( 'NONE', *, *, #4195, .T. ) ;
#91958 = ADVANCED_FACE ( 'NONE', ( #77219 ), #90471, .T. ) ;
#91960 = CARTESIAN_POINT ( 'NONE',  ( -19.38764004357182813, 6.376774720514426953, -21.62823517627351322 ) ) ;
#91961 = CARTESIAN_POINT ( 'NONE',  ( 0.1645010273463760886, -0.3687607960183749145, 1.417169167140625907 ) ) ;
#91962 = CARTESIAN_POINT ( 'NONE',  ( 15.80722972286721983, -12.41807379269815215, -1.500000000000002220 ) ) ;
#91963 = CARTESIAN_POINT ( 'NONE',  ( -10.38599875782317206, -18.32754119035049101, 11.49999999999999645 ) ) ;
#91964 = VECTOR ( 'NONE', #14169, 1000.000000000000000 ) ;
#91965 = CARTESIAN_POINT ( 'NONE',  ( -99.55620429048337883, -24.64965694238574656, 8.947790433994192938 ) ) ;
#91966 = CARTESIAN_POINT ( 'NONE',  ( -19.76278938440450617, -9.944092408650034187, -1.500000000000002220 ) ) ;
#91967 = EDGE_CURVE ( 'NONE', #58907, #95525, #21435, .T. ) ;
#91968 = CARTESIAN_POINT ( 'NONE',  ( -6.383830130275963910, 19.51498944528526991, -1.500000000000002220 ) ) ;
#91969 = CARTESIAN_POINT ( 'NONE',  ( -39.44984910185593208, -25.31589155146792791, 4.278338758482362891 ) ) ;
#91970 = CARTESIAN_POINT ( 'NONE',  ( -60.58907311184719902, -24.52300882791528380, 0.6510814631126233820 ) ) ;
#91971 = ORIENTED_EDGE ( 'NONE', *, *, #5096, .F. ) ;
#91972 = DIRECTION ( 'NONE',  ( -0.000000000000000000, 1.000000000000000000, -0.000000000000000000 ) ) ;
#91973 = EDGE_LOOP ( 'NONE', ( #35642, #91220, #17880, #17966 ) ) ;
#91974 = CARTESIAN_POINT ( 'NONE',  ( -35.52287095715006870, -24.52323809116984421, 9.355190652339436141 ) ) ;
#91975 = PLANE ( 'NONE',  #33988 ) ;
#91976 = ORIENTED_EDGE ( 'NONE', *, *, #98789, .T. ) ;
#91977 = ORIENTED_EDGE ( 'NONE', *, *, #89518, .F. ) ;
#91978 = VERTEX_POINT ( 'NONE', #52413 ) ;
#91979 = DIRECTION ( 'NONE',  ( -0.2488812114211667037, 0.000000000000000000, -0.9685340172660599212 ) ) ;
#91980 = CARTESIAN_POINT ( 'NONE',  ( -71.62287095715009855, -24.33927499327855060, 9.819080762295815390 ) ) ;
#91981 = CARTESIAN_POINT ( 'NONE',  ( -77.52287095715006160, -24.65952944569304606, 1.056160979905698794 ) ) ;
#91982 = CARTESIAN_POINT ( 'NONE',  ( 20.52162115075873672, 2.272738508513782119, -1.500000000000002220 ) ) ;
#91983 = CARTESIAN_POINT ( 'NONE',  ( -5.517532219241116032, 20.92096086382833064, 11.49999999999999645 ) ) ;
#91984 = VERTEX_POINT ( 'NONE', #52917 ) ;
#91985 = DIRECTION ( 'NONE',  ( 0.000000000000000000, -2.173523156925979552E-06, 0.9999999999976378895 ) ) ;
#91986 = CARTESIAN_POINT ( 'NONE',  ( 6.499999999999992895, -1.784922709757266047E-15, -2.500000000000001332 ) ) ;
#91987 = CARTESIAN_POINT ( 'NONE',  ( -21.65924713590726469, 5.634197536097032888, 11.49999999999998934 ) ) ;
#91988 = CARTESIAN_POINT ( 'NONE',  ( -80.37464638460068045, -25.27875090142109826, 7.098502068079202587 ) ) ;
#91989 = CARTESIAN_POINT ( 'NONE',  ( -84.59179061558366186, -24.15543982623907482, -0.2315651400026629836 ) ) ;
#91990 = VERTEX_POINT ( 'NONE', #30054 ) ;
#91991 = CARTESIAN_POINT ( 'NONE',  ( 31.84105487026594261, -5.152774720514426754, -11.95870468328485003 ) ) ;
#91992 = CARTESIAN_POINT ( 'NONE',  ( -49.62369280273893679, -24.66019654487198665, 8.947790411086131712 ) ) ;
#91993 = CARTESIAN_POINT ( 'NONE',  ( -20.67734376658059858, -3.193854526364364954, 11.49999999999998934 ) ) ;
#91994 = EDGE_LOOP ( 'NONE', ( #6496, #55875, #76009, #20593 ) ) ;
#91996 = EDGE_LOOP ( 'NONE', ( #29478, #39464, #98609, #91534 ) ) ;
#91995 = CARTESIAN_POINT ( 'NONE',  ( -86.56264050182306846, -23.48783264082478084, -1.443836473390066377 ) ) ;
#91997 = CIRCLE ( 'NONE', #57991, 84.48086791635432746 ) ;
#91998 = ORIENTED_EDGE ( 'NONE', *, *, #11289, .T. ) ;
#91999 = CARTESIAN_POINT ( 'NONE',  ( -109.5201641829940797, -23.73791477778912551, 11.05961554403169878 ) ) ;
#92000 = CARTESIAN_POINT ( 'NONE',  ( 4.708956132399880978, 20.65895737721473679, -1.500000000000002220 ) ) ;
#92001 = VERTEX_POINT ( 'NONE', #22432 ) ;
#92002 = DIRECTION ( 'NONE',  ( 0.000000000000000000, 1.000000000000000000, 0.000000000000000000 ) ) ;
#92003 = CARTESIAN_POINT ( 'NONE',  ( -99.53757426446047418, -25.12215597945658985, 6.745911859225921070 ) ) ;
#92004 = CARTESIAN_POINT ( 'NONE',  ( 13.71991279636371175, 16.93377936151356877, -1.500000000000002220 ) ) ;
#92005 = CARTESIAN_POINT ( 'NONE',  ( -7.243541020599075786, -6.376774720514408301, 19.27798293355755632 ) ) ;
#92006 = AXIS2_PLACEMENT_3D ( 'NONE', #34142, #49373, #11788 ) ;
#92007 = CARTESIAN_POINT ( 'NONE',  ( 5.314386400780318986, -0.3587747205143965723, -28.55951656536880989 ) ) ;
#92008 = DIRECTION ( 'NONE',  ( 0.000000000000000000, 1.000000000000000000, 0.000000000000000000 ) ) ;
#92009 = CARTESIAN_POINT ( 'NONE',  ( 6.829227106855087825, -20.66181959361685827, -1.500000000000002220 ) ) ;
#92010 = CARTESIAN_POINT ( 'NONE',  ( -0.9988807608215116707, -6.376774720514410077, 19.30497968945844889 ) ) ;
#92012 = VERTEX_POINT ( 'NONE', #44310 ) ;
#92011 = CARTESIAN_POINT ( 'NONE',  ( -18.97848940637192428, 11.77069306843248064, 11.49999999999999645 ) ) ;
#92013 = CARTESIAN_POINT ( 'NONE',  ( -77.52287095715010423, -23.47593901973090524, -1.443836447538997092 ) ) ;
#92014 = CARTESIAN_POINT ( 'NONE',  ( -123.5228709571500616, -24.65952944569304961, 1.056160979905705899 ) ) ;
#92015 = CARTESIAN_POINT ( 'NONE',  ( 31.41423154468143153, -2.682774720514426559, -0.3119954678742140053 ) ) ;
#92016 = EDGE_LOOP ( 'NONE', ( #2153, #20436, #93922, #87535 ) ) ;
#92017 = ORIENTED_EDGE ( 'NONE', *, *, #31925, .T. ) ;
#92018 = ORIENTED_EDGE ( 'NONE', *, *, #82199, .T. ) ;
#92019 = B_SPLINE_CURVE_WITH_KNOTS ( 'NONE', 3,
 ( #28164, #75320, #60624, #16296 ),
 .UNSPECIFIED., .F., .F.,
 ( 4, 4 ),
 ( 0.000000000000000000, 0.0001000000000000028644 ),
 .UNSPECIFIED. ) ;
#92020 = CARTESIAN_POINT ( 'NONE',  ( -124.5895376238167529, -24.66019654487200441, 8.947790411086115725 ) ) ;
#92021 = CARTESIAN_POINT ( 'NONE',  ( 16.79009078985406234, 12.93418496121567252, 11.49999999999998934 ) ) ;
#92022 = FACE_OUTER_BOUND ( 'NONE', #52151, .T. ) ;
#92023 = CARTESIAN_POINT ( 'NONE',  ( -95.62287095714997065, -24.51254535404256885, 9.355368623467656519 ) ) ;
#92024 = LINE ( 'NONE', #91525, #72974 ) ;
#92025 = CARTESIAN_POINT ( 'NONE',  ( -30.57287095715006231, -23.47596702059239604, 11.43887032355635647 ) ) ;
#92026 = CARTESIAN_POINT ( 'NONE',  ( -19.23900614489824079, 2.250179475969715348, 11.49999999999998934 ) ) ;
#92027 = EDGE_CURVE ( 'NONE', #39863, #96596, #33905, .T. ) ;
#92028 = CARTESIAN_POINT ( 'NONE',  ( -70.10894464503664381, -25.31100528015419826, 5.336487379620773019 ) ) ;
#92029 = ORIENTED_EDGE ( 'NONE', *, *, #99713, .F. ) ;
#92030 = ADVANCED_FACE ( 'NONE', ( #61533 ), #82846, .T. ) ;
#92031 = CARTESIAN_POINT ( 'NONE',  ( -2.795030477444873540, 19.22867370847827573, 11.49999999999999645 ) ) ;
#92032 = CARTESIAN_POINT ( 'NONE',  ( 22.81105451610979173, 8.475225279485572472, -18.46691820600746681 ) ) ;
#92033 = ORIENTED_EDGE ( 'NONE', *, *, #29948, .T. ) ;
#92034 = EDGE_CURVE ( 'NONE', #10131, #72641, #45304, .T. ) ;
#92035 = CARTESIAN_POINT ( 'NONE',  ( 2.834823996951755465, -5.876774720514407413, 18.76222163777333307 ) ) ;
#92036 = CARTESIAN_POINT ( 'NONE',  ( 18.22465585706453339, 0.000000000000000000, -2.153101996372891236 ) ) ;
#92037 = ADVANCED_FACE ( 'NONE', ( #69124 ), #76714, .T. ) ;
#92038 = CARTESIAN_POINT ( 'NONE',  ( -130.5728709571500872, -23.78087380709146359, 10.97511746239721653 ) ) ;
#92039 = CARTESIAN_POINT ( 'NONE',  ( -3.832734262880480358, 19.25313627021017382, 11.49999999999998934 ) ) ;
#92040 = B_SPLINE_SURFACE_WITH_KNOTS ( 'NONE', 3, 1, ( 
 ( #63280, #62781 ),
 ( #15572, #100289 ),
 ( #71382, #38417 ),
 ( #93697, #30807 ),
 ( #7964, #94195 ),
 ( #61773, #32305 ),
 ( #47544, #85586 ),
 ( #40426, #63788 ),
 ( #8967, #92691 ),
 ( #23175, #54163 ),
 ( #38918, #69871 ),
 ( #70882, #354 ),
 ( #62269, #1371 ),
 ( #24681, #47043 ),
 ( #77958, #8470 ),
 ( #55665, #11467 ),
 ( #4367, #42933 ),
 ( #18082, #40922 ),
 ( #9969, #34313 ),
 ( #33809, #73376 ),
 ( #11964, #64792 ),
 ( #2368, #35317 ),
 ( #88600, #95708 ),
 ( #58156, #26196 ),
 ( #10973, #72880 ),
 ( #3874, #65290 ),
 ( #72383, #64286 ) ),
 .UNSPECIFIED., .F., .F., .F.,
 ( 4, 1, 1, 1, 1, 1, 1, 1, 1, 1, 1, 1, 1, 1, 1, 1, 1, 1, 1, 1, 1, 1, 1, 1, 4 ),
 ( 2, 2 ),
 ( 0.000000000000000000, 0.06506328961727912696, 0.1267731664665228686, 0.1855157632260792111, 0.2407646791677150733, 0.2929797960235981935, 0.3422503727797673867, 0.3889192861856604622, 0.4327756640583106384, 0.4746284326311178137, 0.5147746906379535581, 0.5536058934984424695, 0.5914264064311730573, 0.6280281199460679975, 0.6638036341103209503, 0.6989843361316647741, 0.7335914893067051468, 0.7676284691511403580, 0.8012083477865920011, 0.8342638397266241013, 0.8669806947287761467, 0.8997197415181606983, 0.9327019124985390652, 0.9661758834327494050, 1.000000000000000000 ),
 ( 0.000000000000000000, 1.000000000000000000 ),
 .UNSPECIFIED. ) ;
#92041 = EDGE_CURVE ( 'NONE', #89848, #29762, #7725, .T. ) ;
#92042 = CARTESIAN_POINT ( 'NONE',  ( -39.62287095715005592, -24.66019654487199020, 8.947790411086135265 ) ) ;
#92043 = ORIENTED_EDGE ( 'NONE', *, *, #50242, .T. ) ;
#92044 = CARTESIAN_POINT ( 'NONE',  ( 14.33184905138074683, -16.10332302735202958, 11.49999999999998934 ) ) ;
#92045 = CARTESIAN_POINT ( 'NONE',  ( -85.92287095715005307, -23.47596703998600631, 11.44779298504227860 ) ) ;
#92046 = ADVANCED_FACE ( 'NONE', ( #60538 ), #67649, .T. ) ;
#92047 = DIRECTION ( 'NONE',  ( -3.773278334453079618E-23, 0.9999999999976377785, 2.173523156925979975E-06 ) ) ;
#92048 = DIRECTION ( 'NONE',  ( -0.000000000000000000, 1.000000000000000000, -0.000000000000000000 ) ) ;
#92049 = CARTESIAN_POINT ( 'NONE',  ( -18.14924840124409045, -14.16824886576183040, -1.500000000000002220 ) ) ;
#92050 = DATE_AND_TIME ( #22023, #61945 ) ;
#92051 = CARTESIAN_POINT ( 'NONE',  ( -127.2228709571500360, -23.47593901973090524, -1.443836447538996204 ) ) ;
#92052 = CARTESIAN_POINT ( 'NONE',  ( -50.70677674236874566, -25.18370859199909972, 3.285367768258824483 ) ) ;
#92053 = CARTESIAN_POINT ( 'NONE',  ( -20.14672940031187665, -1.731937678239350298, 11.49999999999999645 ) ) ;
#92054 = CARTESIAN_POINT ( 'NONE',  ( -121.5205767367703373, -23.96169478059713853, 10.65365249895717525 ) ) ;
#92055 = DIRECTION ( 'NONE',  ( -0.000000000000000000, -1.000000000000000000, -0.000000000000000000 ) ) ;
#92056 = CARTESIAN_POINT ( 'NONE',  ( -111.6050501299251323, -25.10921541419112302, 3.602892040021733688 ) ) ;
#92057 = CARTESIAN_POINT ( 'NONE',  ( 8.160000000000000142, -2.890508098367099432, -0.2344417481469836528 ) ) ;
#92058 = CARTESIAN_POINT ( 'NONE',  ( -110.5404475696186779, -25.29779158700655728, 3.309296744833758908 ) ) ;
#92059 = CARTESIAN_POINT ( 'NONE',  ( 19.57267778704439820, -3.578973306870405047, 11.49999999999998934 ) ) ;
#92060 = B_SPLINE_CURVE_WITH_KNOTS ( 'NONE', 3,
 ( #54645, #344, #100278, #14567, #92683, #38908, #6960, #23163, #22664, #53652 ),
 .UNSPECIFIED., .F., .F.,
 ( 4, 2, 2, 2, 4 ),
 ( 0.000000000000000000, 0.0004833345490728424001, 0.0009666690981456848002, 0.001450003647218527092, 0.001933338196291368299 ),
 .UNSPECIFIED. ) ;
#92061 = CARTESIAN_POINT ( 'NONE',  ( -68.92287095715006728, -23.47593901973090169, -1.443836447538997536 ) ) ;
#92062 = CARTESIAN_POINT ( 'NONE',  ( -9.637476322613308000, -17.25261889746210997, -1.500000000000002220 ) ) ;
#92063 = AXIS2_PLACEMENT_3D ( 'NONE', #95556, #95054, #25035 ) ;
#92064 = CARTESIAN_POINT ( 'NONE',  ( -56.52206875506576012, -23.48783264082477018, -1.443836473390095909 ) ) ;
#92065 = CARTESIAN_POINT ( 'NONE',  ( -40.07089665442598658, -25.29116527456120522, 2.873457746617287700 ) ) ;
#92066 = CARTESIAN_POINT ( 'NONE',  ( -42.52287095715006160, -24.50216790748203977, 0.6166512839542503954 ) ) ;
#92067 = CARTESIAN_POINT ( 'NONE',  ( 14.23986175545555355, -14.96101607593195304, 11.49999999999999645 ) ) ;
#92068 = CARTESIAN_POINT ( 'NONE',  ( -39.56136241089613037, -25.31628735779903039, 5.536731292741799315 ) ) ;
#92069 = AXIS2_PLACEMENT_3D ( 'NONE', #79643, #55833, #72550 ) ;
#92070 = FACE_OUTER_BOUND ( 'NONE', #72210, .T. ) ;
#92071 = CARTESIAN_POINT ( 'NONE',  ( -13.58842472641693711, -18.21064416987719525, 11.49999999999999645 ) ) ;
#92072 = ORIENTED_EDGE ( 'NONE', *, *, #8701, .F. ) ;
#92073 = CARTESIAN_POINT ( 'NONE',  ( -67.52287095715006160, -24.64898659630528854, 1.056161002820824368 ) ) ;
#92074 = CARTESIAN_POINT ( 'NONE',  ( 29.73828978136053891, -5.356774720514425603, -4.021765098496561386 ) ) ;
#92075 = CIRCLE ( 'NONE', #82371, 2.499999999999995115 ) ;
#92076 = CARTESIAN_POINT ( 'NONE',  ( 17.97931717627152182, 9.192180251422895410, -1.500000000000002220 ) ) ;
#92077 = CARTESIAN_POINT ( 'NONE',  ( -108.6228709571500701, -23.72773821059535848, 11.05748984161097503 ) ) ;
#92078 = CARTESIAN_POINT ( 'NONE',  ( -45.58953762381672448, -23.48786465467240703, 11.44779295918255002 ) ) ;
#92079 = ORIENTED_EDGE ( 'NONE', *, *, #83449, .T. ) ;
#92080 = ORIENTED_EDGE ( 'NONE', *, *, #2367, .T. ) ;
#92081 = CARTESIAN_POINT ( 'NONE',  ( -0.001774553997815280816, -5.876774720514413630, 19.59623724171353487 ) ) ;
#92082 = CARTESIAN_POINT ( 'NONE',  ( 18.88093902437788785, 12.95799798663108682, -1.500000000000002220 ) ) ;
#92083 = CARTESIAN_POINT ( 'NONE',  ( -41.86183995336322994, -25.27646494108434183, 4.023331222604434210 ) ) ;
#92084 = CARTESIAN_POINT ( 'NONE',  ( 21.56569437331729233, -1.927008741106717604, -1.500000000000002220 ) ) ;
#92085 = AXIS2_PLACEMENT_3D ( 'NONE', #86458, #222, #40289 ) ;
#92086 = DIRECTION ( 'NONE',  ( 1.000000000000000000, 3.773278334444167608E-23, 8.201307833595939069E-29 ) ) ;
#92087 = CARTESIAN_POINT ( 'NONE',  ( -34.65813035707638079, -23.73766607897670866, -1.055555164236443133 ) ) ;
#92088 = CARTESIAN_POINT ( 'NONE',  ( -16.12721948686093754, -13.32240427740599564, 11.49999999999999645 ) ) ;
#92089 = VERTEX_POINT ( 'NONE', #29064 ) ;
#92090 = B_SPLINE_CURVE_WITH_KNOTS ( 'NONE', 3,
 ( #36788, #36294, #20546, #81962 ),
 .UNSPECIFIED., .F., .F.,
 ( 4, 4 ),
 ( 0.000000000000000000, 9.999999999998897304E-05 ),
 .UNSPECIFIED. ) ;
#92091 = CARTESIAN_POINT ( 'NONE',  ( -104.5228709571501184, -23.48783264082477373, -1.443836473390087027 ) ) ;
#92092 = CARTESIAN_POINT ( 'NONE',  ( 7.855769811932122870, -20.56199346058834720, -1.500000000000002220 ) ) ;
#92093 = EDGE_CURVE ( 'NONE', #32532, #46308, #79360, .T. ) ;
#92094 = CARTESIAN_POINT ( 'NONE',  ( -105.6261421520168540, -24.73531770709095312, 8.716586749053508498 ) ) ;
#92095 = CARTESIAN_POINT ( 'NONE',  ( -41.68940843163829868, -25.10925916055124318, 3.512445505603538187 ) ) ;
#92096 = ORIENTED_EDGE ( 'NONE', *, *, #14221, .T. ) ;
#92097 = CARTESIAN_POINT ( 'NONE',  ( 4.959895098850171102, -6.376774720514411854, 19.67755022954121813 ) ) ;
#92098 = ADVANCED_FACE ( 'NONE', ( #68635 ), #6226, .T. ) ;
#92099 = CARTESIAN_POINT ( 'NONE',  ( -90.58606251549953470, -24.73531770709095312, 8.716586749053512051 ) ) ;
#92100 = EDGE_LOOP ( 'NONE', ( #26026, #44940, #90695, #2642 ) ) ;
#92101 = FACE_OUTER_BOUND ( 'NONE', #12868, .T. ) ;
#92102 = ORIENTED_EDGE ( 'NONE', *, *, #99098, .T. ) ;
#92103 = VERTEX_POINT ( 'NONE', #99059 ) ;
#92104 = CARTESIAN_POINT ( 'NONE',  ( -71.52210967603697611, -23.48786465467241058, 11.44779295918254824 ) ) ;
#92105 = CARTESIAN_POINT ( 'NONE',  ( -101.7776484685884242, -25.27404881181734808, 3.986250615313824408 ) ) ;
#92106 = CARTESIAN_POINT ( 'NONE',  ( -100.5228709571500758, -24.51254535375843702, 9.355368624242247577 ) ) ;
#92107 = CARTESIAN_POINT ( 'NONE',  ( 20.06376955418885899, 4.186446014007643157, -1.500000000000002220 ) ) ;
#92108 = ORIENTED_EDGE ( 'NONE', *, *, #65642, .F. ) ;
#92109 = CARTESIAN_POINT ( 'NONE',  ( -3.095730855174848362, -5.876774720514412742, 20.04377961306771638 ) ) ;
#92110 = DIRECTION ( 'NONE',  ( -3.773278334453080206E-23, 0.9999999999976377785, 2.173523156925979975E-06 ) ) ;
#92111 = CARTESIAN_POINT ( 'NONE',  ( -99.58953762381672448, -23.48783264082478794, -1.443836473390061936 ) ) ;
#92112 = CARTESIAN_POINT ( 'NONE',  ( -18.06118310651259407, 13.05043149098080058, -1.500000000000002220 ) ) ;
#92113 = CARTESIAN_POINT ( 'NONE',  ( -74.62287095715005592, -29.50250243563736774, 8.947779886222143375 ) ) ;
#92114 = CARTESIAN_POINT ( 'NONE',  ( -7.426349086584751902, 10.80195425911416329, -0.9450485415980990345 ) ) ;
#92115 = ORIENTED_EDGE ( 'NONE', *, *, #79693, .T. ) ;
#92116 = LINE ( 'NONE', #12992, #71135 ) ;
#92117 = CARTESIAN_POINT ( 'NONE',  ( -29.60812400815161283, -24.63645724241111168, 6.685405290659707234 ) ) ;
#92118 = CARTESIAN_POINT ( 'NONE',  ( 16.81283763619640936, 12.23492182941471107, 11.49999999999998934 ) ) ;
#92119 = EDGE_LOOP ( 'NONE', ( #14012, #27252, #13243, #17631 ) ) ;
#92120 = EDGE_CURVE ( 'NONE', #61188, #10228, #84343, .T. ) ;
#92122 = VERTEX_POINT ( 'NONE', #14826 ) ;
#92121 = CARTESIAN_POINT ( 'NONE',  ( -54.62287095715004881, -24.50216790748096685, 0.6166512839513625943 ) ) ;
#92123 = B_SPLINE_SURFACE_WITH_KNOTS ( 'NONE', 3, 3, ( 
 ( #37565, #60916, #84732, #46689 ),
 ( #13715, #15223, #70012, #498 ),
 ( #60421, #46181, #44687, #91346 ),
 ( #21821, #91843, #77109, #22319 ),
 ( #69520, #55308, #86240, #63938 ),
 ( #54803, #16224, #40577, #10620 ),
 ( #86737, #47189, #56815, #17226 ) ),
 .UNSPECIFIED., .F., .F., .F.,
 ( 4, 3, 4 ),
 ( 4, 4 ),
 ( 0.7945040050992233649, 0.8970133687736494554, 0.9995227324480754350 ),
 ( 0.2195497878891723154, 0.2206638711953707588 ),
 .UNSPECIFIED. ) ;
#92124 = CARTESIAN_POINT ( 'NONE',  ( -98.52287095715006160, -23.48786465467241769, 11.44779295918254114 ) ) ;
#92125 = ORIENTED_EDGE ( 'NONE', *, *, #98205, .T. ) ;
#92126 = ORIENTED_EDGE ( 'NONE', *, *, #82014, .T. ) ;
#92127 = DIRECTION ( 'NONE',  ( 0.000000000000000000, 0.000000000000000000, 1.000000000000000000 ) ) ;
#92128 = CARTESIAN_POINT ( 'NONE',  ( -50.72667573002448904, -25.10935765147311471, 2.869183402993591425 ) ) ;
#92129 = CARTESIAN_POINT ( 'NONE',  ( 6.190876379491990988, -5.356774720513713284, -27.38145113946987408 ) ) ;
#92130 = CARTESIAN_POINT ( 'NONE',  ( -60.62287095715004881, -29.50250786944525672, 11.44777988621623876 ) ) ;
#92131 = CARTESIAN_POINT ( 'NONE',  ( -109.2249784094242244, -25.20198318546772498, 3.338762932793643223 ) ) ;
#92132 = CARTESIAN_POINT ( 'NONE',  ( -43.62287095715004881, -29.50250243563736774, 8.947779886222148704 ) ) ;
#92134 = ORIENTED_EDGE ( 'NONE', *, *, #28249, .F. ) ;
#92133 = CARTESIAN_POINT ( 'NONE',  ( 21.55033589006239936, 5.121329677682045833, 11.49999999999999645 ) ) ;
#92135 = CARTESIAN_POINT ( 'NONE',  ( -44.62287095715005592, -24.51387760970723662, 9.387446482453432495 ) ) ;
#92136 = CARTESIAN_POINT ( 'NONE',  ( -22.51868310087907687, -2.221351303042197411, 11.49999999999998934 ) ) ;
#92137 = VECTOR ( 'NONE', #54382, 1000.000000000000227 ) ;
#92139 = ORIENTED_EDGE ( 'NONE', *, *, #98444, .T. ) ;
#92138 = CARTESIAN_POINT ( 'NONE',  ( -28.74698468279304819, -24.98503885035050942, 7.079829357813114399 ) ) ;
#92140 = ORIENTED_EDGE ( 'NONE', *, *, #91840, .T. ) ;
#92141 = CARTESIAN_POINT ( 'NONE',  ( 5.802984775641024662, -6.376774720514402972, 18.35026041666666430 ) ) ;
#92142 = CARTESIAN_POINT ( 'NONE',  ( 10.61947033613929214, 17.11087026910869469, -1.500000000000002220 ) ) ;
#92143 = CARTESIAN_POINT ( 'NONE',  ( -71.52287095715007581, -29.50248528299804818, 1.056150453629036701 ) ) ;
#92144 = ORIENTED_EDGE ( 'NONE', *, *, #5153, .F. ) ;
#92145 = VECTOR ( 'NONE', #99311, 1000.000000000000114 ) ;
#92146 = CARTESIAN_POINT ( 'NONE',  ( -39.62287095715005592, -23.48786465467240347, 11.44779295918255180 ) ) ;
#92147 = CARTESIAN_POINT ( 'NONE',  ( -22.28969446433750434, -1.297463027894488086, -1.500000000000002220 ) ) ;
#92148 = ORIENTED_EDGE ( 'NONE', *, *, #1444, .F. ) ;
#92149 = VERTEX_POINT ( 'NONE', #45795 ) ;
#92150 = CARTESIAN_POINT ( 'NONE',  ( 2.100208336950355914, 0.000000000000000000, 0.000000000000000000 ) ) ;
#92151 = CARTESIAN_POINT ( 'NONE',  ( -34.62287095715005592, -29.50248528299804818, 1.056150453629029817 ) ) ;
#92152 = ADVANCED_FACE ( 'NONE', ( #7216 ), #30562, .T. ) ;
#92153 = FACE_OUTER_BOUND ( 'NONE', #57773, .T. ) ;
#92154 = EDGE_CURVE ( 'NONE', #76855, #44309, #92268, .T. ) ;
#92155 = LINE ( 'NONE', #84546, #65058 ) ;
#92156 = CARTESIAN_POINT ( 'NONE',  ( 17.64699390344983598, -8.409456921668478913, -1.500000000000002220 ) ) ;
#92157 = EDGE_CURVE ( 'NONE', #10237, #68291, #23643, .T. ) ;
#92158 = CARTESIAN_POINT ( 'NONE',  ( -102.5228709571501327, -23.73907113217669007, -1.053371485781297023 ) ) ;
#92159 = CARTESIAN_POINT ( 'NONE',  ( -21.25412285906045895, 3.082840150875858054, -1.500000000000002220 ) ) ;
#92160 = CARTESIAN_POINT ( 'NONE',  ( -25.53440485667337612, -24.58000155304849699, 4.657483218939315606 ) ) ;
#92161 = EDGE_CURVE ( 'NONE', #83403, #73995, #645, .T. ) ;
#92163 = DIRECTION ( 'NONE',  ( 1.000000000000000000, 0.000000000000000000, 0.000000000000000000 ) ) ;
#92162 = B_SPLINE_CURVE_WITH_KNOTS ( 'NONE', 3,
 ( #24597, #86504, #47956, #40337, #71289, #80896 ),
 .UNSPECIFIED., .F., .F.,
 ( 4, 2, 4 ),
 ( 1.570755371633777598E-05, 0.001396183895866084934, 0.002776660238015832109 ),
 .UNSPECIFIED. ) ;
#92164 = FACE_OUTER_BOUND ( 'NONE', #89092, .T. ) ;
#92165 = CARTESIAN_POINT ( 'NONE',  ( 10.78062712001149492, -20.16176685268226976, -1.500000000000002220 ) ) ;
#92166 = B_SPLINE_CURVE_WITH_KNOTS ( 'NONE', 3,
 ( #93773, #39992, #54233, #62341 ),
 .UNSPECIFIED., .F., .F.,
 ( 4, 4 ),
 ( 0.2099358345183179875, 0.2189422657904334657 ),
 .UNSPECIFIED. ) ;
#92167 = VECTOR ( 'NONE', #83051, 1000.000000000000114 ) ;
#92168 = DATE_AND_TIME ( #22640, #90969 ) ;
#92169 = DIRECTION ( 'NONE',  ( 0.000000000000000000, -0.9999999999976377785, -2.173523156925979975E-06 ) ) ;
#92170 = DIRECTION ( 'NONE',  ( 0.000000000000000000, 0.000000000000000000, 1.000000000000000000 ) ) ;
#92171 = CARTESIAN_POINT ( 'NONE',  ( -7.473237707827510512, 18.53023608995856009, 11.49999999999999645 ) ) ;
#92172 = CARTESIAN_POINT ( 'NONE',  ( -89.40841769935767047, -25.06732983082694943, 7.447789526168953955 ) ) ;
#92173 = LINE ( 'NONE', #15547, #8457 ) ;
#92174 = CARTESIAN_POINT ( 'NONE',  ( -108.6228709571500275, -23.72747288104442021, -1.053458166803660889 ) ) ;
#92175 = ORIENTED_EDGE ( 'NONE', *, *, #75366, .F. ) ;
#92176 = EDGE_CURVE ( 'NONE', #18738, #8368, #59973, .T. ) ;
#92177 = CARTESIAN_POINT ( 'NONE',  ( 2.499999999999995115, 19.99999999999999645, 0.000000000000000000 ) ) ;
#92178 = CARTESIAN_POINT ( 'NONE',  ( -114.5562042904833788, -24.64898659630529210, 1.056161002820829475 ) ) ;
#92179 = CARTESIAN_POINT ( 'NONE',  ( -12.78816955685674372, 17.57309652720472570, -1.500000000000002220 ) ) ;
#92180 = CARTESIAN_POINT ( 'NONE',  ( -108.6228709571500559, -24.64965695001468404, 8.947790433994176951 ) ) ;
#92181 = CARTESIAN_POINT ( 'NONE',  ( 16.12930680145378304, -11.13525102954884893, -1.500000000000002220 ) ) ;
#92182 = DIRECTION ( 'NONE',  ( -3.773278334453080206E-23, 0.9999999999976377785, 2.173523156925979975E-06 ) ) ;
#92183 = CARTESIAN_POINT ( 'NONE',  ( -41.43233941641154416, -25.25932830633372461, 3.941234411137095606 ) ) ;
#92184 = SECURITY_CLASSIFICATION_LEVEL ( 'unclassified' ) ;
#92185 = CARTESIAN_POINT ( 'NONE',  ( -28.98875734969026041, -0.3587747205144265483, 25.61802280011862720 ) ) ;
#92186 = CARTESIAN_POINT ( 'NONE',  ( -124.2228709571500502, -23.47596703998600631, 11.44779298504227860 ) ) ;
#92187 = CARTESIAN_POINT ( 'NONE',  ( -17.34406541665444124, 10.97931167347951842, 11.49999999999999645 ) ) ;
#92188 = CARTESIAN_POINT ( 'NONE',  ( -1.675486951385420475, 10.82748519320431591, -3.549999999999999822 ) ) ;
#92189 = DIRECTION ( 'NONE',  ( -0.000000000000000000, 0.000000000000000000, 1.000000000000000000 ) ) ;
#92190 = VERTEX_POINT ( 'NONE', #25454 ) ;
#92191 = SHAPE_REPRESENTATION_RELATIONSHIP ( 'NONE' , 'NONE' ,  #55609, #29431 ) ;
#92192 = DIRECTION ( 'NONE',  ( -3.773278334453079030E-23, 0.9999999999976377785, 2.173523156925979128E-06 ) ) ;
#92193 = CARTESIAN_POINT ( 'NONE',  ( -39.67258447180102365, -25.18430942437969122, 3.621101466496972066 ) ) ;
#92194 = VECTOR ( 'NONE', #100174, 1000.000000000000114 ) ;
#92195 = CARTESIAN_POINT ( 'NONE',  ( -125.5916857295030553, -23.48786465467241413, 11.44779295918253581 ) ) ;
#92196 = CARTESIAN_POINT ( 'NONE',  ( -85.62287095715004170, -23.48783264082478794, -1.443836473390063713 ) ) ;
#92197 = CIRCLE ( 'NONE', #59844, 24.00000000000000000 ) ;
#92198 = CARTESIAN_POINT ( 'NONE',  ( -8.160000000000000142, 0.1579206558577708475, 5.788828319098143105 ) ) ;
#92199 = CARTESIAN_POINT ( 'NONE',  ( 10.34999999999999254, 4.999999999999998224, 2.100000000000000089 ) ) ;
#92200 = B_SPLINE_CURVE_WITH_KNOTS ( 'NONE', 3,
 ( #19057, #95190, #25674, #49030, #82455, #4351 ),
 .UNSPECIFIED., .F., .F.,
 ( 4, 2, 4 ),
 ( 0.000000000000000000, 0.001380901958385387027, 0.002761803916770774053 ),
 .UNSPECIFIED. ) ;
#92201 = EDGE_CURVE ( 'NONE', #18856, #67869, #71138, .T. ) ;
#92202 = CARTESIAN_POINT ( 'NONE',  ( -22.67921066581790868, 4.291001918001082771, 11.49999999999999645 ) ) ;
#92203 = CARTESIAN_POINT ( 'NONE',  ( -15.22011711465338912, -17.00649957279452451, -1.500000000000002220 ) ) ;
#92204 = CARTESIAN_POINT ( 'NONE',  ( -74.52211797261165316, -23.48783264082477018, -1.443836473390096353 ) ) ;
#92205 = CARTESIAN_POINT ( 'NONE',  ( -5.824076695599092801, -6.376774720514411854, 19.72913074730691108 ) ) ;
#92206 = CARTESIAN_POINT ( 'NONE',  ( -60.45647493444359810, -25.28662977279051560, 6.028426056058751037 ) ) ;
#92207 = B_SPLINE_CURVE_WITH_KNOTS ( 'NONE', 3,
 ( #5556, #80687, #12666, #42150 ),
 .UNSPECIFIED., .F., .F.,
 ( 4, 4 ),
 ( 0.000000000000000000, 1.000000000000000000 ),
 .UNSPECIFIED. ) ;
#92208 = CARTESIAN_POINT ( 'NONE',  ( 6.649717926671450563, 21.43536518531312396, 11.49999999999999645 ) ) ;
#92209 = VECTOR ( 'NONE', #58762, 1000.000000000000114 ) ;
#92210 = FACE_OUTER_BOUND ( 'NONE', #82859, .T. ) ;
#92211 = CARTESIAN_POINT ( 'NONE',  ( -38.62287095715007013, -23.95044443724992078, 10.65354141964649592 ) ) ;
#92212 = CARTESIAN_POINT ( 'NONE',  ( -17.33335002049248530, 13.43749923854009509, -1.500000000000002220 ) ) ;
#92213 = ADVANCED_FACE ( 'NONE', ( #24948 ), #8735, .T. ) ;
#92214 = CARTESIAN_POINT ( 'NONE',  ( -5.799455386767018439, -6.376774720514415407, 19.66076420632890276 ) ) ;
#92215 = CARTESIAN_POINT ( 'NONE',  ( -87.62602049761908063, -24.51419770103156281, 9.386484678747175181 ) ) ;
#92216 = CARTESIAN_POINT ( 'NONE',  ( -33.52287095715006160, -23.48786465467240347, 11.44779295918255357 ) ) ;
#92217 = CARTESIAN_POINT ( 'NONE',  ( -78.49839763410953708, -24.65952944569304606, 1.056160979905704789 ) ) ;
#92218 = DIRECTION ( 'NONE',  ( 0.000000000000000000, -1.000000000000000000, 0.000000000000000000 ) ) ;
#92219 = ORIENTED_EDGE ( 'NONE', *, *, #50567, .F. ) ;
#92220 = VECTOR ( 'NONE', #44800, 1000.000000000000114 ) ;
#92221 = CARTESIAN_POINT ( 'NONE',  ( 20.41236503877875563, 1.188189311754236144, 11.49999999999998934 ) ) ;
#92222 = ORIENTED_EDGE ( 'NONE', *, *, #21906, .T. ) ;
#92223 = ORIENTED_EDGE ( 'NONE', *, *, #95878, .T. ) ;
#92224 = VERTEX_POINT ( 'NONE', #62026 ) ;
#92225 = ORIENTED_EDGE ( 'NONE', *, *, #72147, .F. ) ;
#92226 = CARTESIAN_POINT ( 'NONE',  ( -22.67921066581790868, 4.291001918001082771, 11.49999999999998934 ) ) ;
#92227 = CARTESIAN_POINT ( 'NONE',  ( -39.43812566566255384, -25.18341647909762315, 3.283321612209681994 ) ) ;
#92228 = CARTESIAN_POINT ( 'NONE',  ( -17.45352675615719917, 10.31968153043333380, -1.500000000000002220 ) ) ;
#92229 = EDGE_LOOP ( 'NONE', ( #52170, #11010, #87242, #37463 ) ) ;
#92230 = CARTESIAN_POINT ( 'NONE',  ( -122.5228709571501042, -24.33832256527049154, 0.1851278514138668951 ) ) ;
#92231 = CARTESIAN_POINT ( 'NONE',  ( -41.69070460756492480, -25.31528773746466143, 4.890768902268528784 ) ) ;
#92232 = CARTESIAN_POINT ( 'NONE',  ( -94.52287095715006160, -23.47596703998600631, 11.44779298504228393 ) ) ;
#92233 = CARTESIAN_POINT ( 'NONE',  ( -70.55922828164491989, -23.85016227208580730, -0.8807180028928335291 ) ) ;
#92235 = ORIENTED_EDGE ( 'NONE', *, *, #74955, .T. ) ;
#92234 = CARTESIAN_POINT ( 'NONE',  ( -3.867184171070207288, -21.11305558764578194, 11.49999999999999645 ) ) ;
#92236 = DIRECTION ( 'NONE',  ( -1.000000000000000000, -0.000000000000000000, -0.000000000000000000 ) ) ;
#92237 = CARTESIAN_POINT ( 'NONE',  ( 15.77421270221668692, 3.602820947333609691, -28.08718493694523133 ) ) ;
#92238 = ORIENTED_EDGE ( 'NONE', *, *, #16444, .F. ) ;
#92239 = CARTESIAN_POINT ( 'NONE',  ( 20.67342648114324533, -1.018679444107209342, -1.500000000000002220 ) ) ;
#92240 = VERTEX_POINT ( 'NONE', #2141 ) ;
#92241 = CC_DESIGN_PERSON_AND_ORGANIZATION_ASSIGNMENT ( #83434, #82443, ( #16510 ) ) ;
#92244 = ORIENTED_EDGE ( 'NONE', *, *, #97201, .T. ) ;
#92243 = VECTOR ( 'NONE', #68232, 1000.000000000000000 ) ;
#92242 = LINE ( 'NONE', #85131, #517 ) ;
#92245 = B_SPLINE_CURVE_WITH_KNOTS ( 'NONE', 3,
 ( #20752, #50727, #81672, #28373 ),
 .UNSPECIFIED., .F., .F.,
 ( 4, 4 ),
 ( 0.000000000000000000, 9.999999999998897304E-05 ),
 .UNSPECIFIED. ) ;
#92246 = CARTESIAN_POINT ( 'NONE',  ( -28.52198438452846574, -23.32368101661869275, -1.443835813551990865 ) ) ;
#92247 = ORIENTED_EDGE ( 'NONE', *, *, #88964, .F. ) ;
#92248 = ORIENTED_EDGE ( 'NONE', *, *, #8796, .F. ) ;
#92249 = CARTESIAN_POINT ( 'NONE',  ( 4.039061187531148178, -6.376774720514401196, 18.18637930035166761 ) ) ;
#92250 = CARTESIAN_POINT ( 'NONE',  ( -65.53231158233933229, -24.92564183028979130, 1.928384488918254869 ) ) ;
#92251 = CARTESIAN_POINT ( 'NONE',  ( 20.73430856240977249, 7.200853762728330665, 11.49999999999999645 ) ) ;
#92252 = CARTESIAN_POINT ( 'NONE',  ( 6.660000000000001030, -9.123836073446797812, -2.666350264951732552 ) ) ;
#92253 = CARTESIAN_POINT ( 'NONE',  ( 1.525329354412473970, -22.51392980886878448, 11.49999999999998934 ) ) ;
#92254 = ADVANCED_FACE ( 'NONE', ( #39673 ), #16334, .F. ) ;
#92255 = CARTESIAN_POINT ( 'NONE',  ( -20.02981537788295441, -6.213780249082809348, -1.500000000000002220 ) ) ;
#92256 = CARTESIAN_POINT ( 'NONE',  ( -124.6228709571500559, -29.50248528299804818, 1.056150453629045360 ) ) ;
#92257 = CARTESIAN_POINT ( 'NONE',  ( 9.940598223437577374, -5.876774720514426953, 22.08128695274315945 ) ) ;
#92258 = ORIENTED_EDGE ( 'NONE', *, *, #56853, .T. ) ;
#92259 = ORIENTED_EDGE ( 'NONE', *, *, #100027, .F. ) ;
#92260 = ORIENTED_EDGE ( 'NONE', *, *, #61005, .T. ) ;
#92261 = CARTESIAN_POINT ( 'NONE',  ( 2.499999999999994671, 18.99999999999977618, 0.000000000000000000 ) ) ;
#92262 = CARTESIAN_POINT ( 'NONE',  ( -14.35963886870962192, 16.04489112172382903, -1.500000000000002220 ) ) ;
#92263 = CARTESIAN_POINT ( 'NONE',  ( 9.019313479210172346, -0.9107773096390181511, -3.707288619710387145 ) ) ;
#92264 = ORIENTED_EDGE ( 'NONE', *, *, #88218, .T. ) ;
#92265 = CARTESIAN_POINT ( 'NONE',  ( -15.95541298346445735, 13.85296639876547076, 11.49999999999998934 ) ) ;
#92266 = CARTESIAN_POINT ( 'NONE',  ( 11.93051494998403683, 1.682774720514426114, 10.48039711075945490 ) ) ;
#92267 = CARTESIAN_POINT ( 'NONE',  ( -89.81226385320383088, -29.50249166729307149, 3.993452963156916002 ) ) ;
#92269 = CARTESIAN_POINT ( 'NONE',  ( -50.17717618564654458, -25.30219648044955250, 4.715273004579882077 ) ) ;
#92268 = CIRCLE ( 'NONE', #32377, 129.7684398600581517 ) ;
#92270 = FACE_OUTER_BOUND ( 'NONE', #9697, .T. ) ;
#92271 = CARTESIAN_POINT ( 'NONE',  ( 0.000000000000000000, -0.3850000000000046163, 1.529999999999998916 ) ) ;
#92272 = CARTESIAN_POINT ( 'NONE',  ( 20.51613352552997327, 8.347415244503286758, -1.500000000000002220 ) ) ;
#92273 = CARTESIAN_POINT ( 'NONE',  ( -112.5228709571500616, -23.48783264083431988, -1.443836473375253782 ) ) ;
#92274 = EDGE_CURVE ( 'NONE', #47959, #17515, #23946, .T. ) ;
#92275 = ORIENTED_EDGE ( 'NONE', *, *, #59167, .T. ) ;
#92276 = CARTESIAN_POINT ( 'NONE',  ( -51.66594184980125704, -25.31633186406339675, 5.409172801058263147 ) ) ;
#92277 = CARTESIAN_POINT ( 'NONE',  ( 13.12137440454564796, 3.706387542726002682, -28.15098661896695376 ) ) ;
#92278 = CARTESIAN_POINT ( 'NONE',  ( 30.53060340732035982, 5.278399900168558645, 6.051577412957072077 ) ) ;
#92279 = VECTOR ( 'NONE', #83376, 1000.000000000000000 ) ;
#92280 = CARTESIAN_POINT ( 'NONE',  ( -100.5441727580858782, -25.00158670708910691, 2.256160236439218369 ) ) ;
#92281 = AXIS2_PLACEMENT_3D ( 'NONE', #14823, #76711, #14322 ) ;
#92282 = CARTESIAN_POINT ( 'NONE',  ( 19.43689267596983683, 0.5339526363925560792, -1.500000000000002220 ) ) ;
#92283 = EDGE_CURVE ( 'NONE', #78060, #70264, #11302, .T. ) ;
#92284 = VECTOR ( 'NONE', #53290, 1000.000000000000000 ) ;
#92285 = B_SPLINE_CURVE_WITH_KNOTS ( 'NONE', 3,
 ( #93975, #23961, #64567, #630 ),
 .UNSPECIFIED., .F., .F.,
 ( 4, 4 ),
 ( 0.000000000000000000, 9.999999999998897304E-05 ),
 .UNSPECIFIED. ) ;
#92286 = CARTESIAN_POINT ( 'NONE',  ( 6.831138157384286203, 20.27010762675863731, 11.49999999999998934 ) ) ;
#92287 = CARTESIAN_POINT ( 'NONE',  ( -38.52287095715007581, -24.35013146730203815, 9.818937971375103047 ) ) ;
#92288 = LINE ( 'NONE', #45626, #28493 ) ;
#92289 = EDGE_CURVE ( 'NONE', #79731, #97458, #85856, .T. ) ;
#92290 = CARTESIAN_POINT ( 'NONE',  ( 0.000000000000000000, 2.682774720514426559, 0.000000000000000000 ) ) ;
#92291 = FACE_OUTER_BOUND ( 'NONE', #42714, .T. ) ;
#92292 = CARTESIAN_POINT ( 'NONE',  ( -19.66899025692886838, 11.29834648773183581, -1.500000000000002220 ) ) ;
#92293 = AXIS2_PLACEMENT_3D ( 'NONE', #1559, #48743, #18275 ) ;
#92294 = CARTESIAN_POINT ( 'NONE',  ( -106.6228709571500559, -23.47593901973091235, -1.443836447538999312 ) ) ;
#92295 = FACE_OUTER_BOUND ( 'NONE', #40984, .T. ) ;
#92296 = CARTESIAN_POINT ( 'NONE',  ( -11.78406182805296254, 15.88391379356440503, 11.49999999999999645 ) ) ;
#92297 = CARTESIAN_POINT ( 'NONE',  ( 15.32643653063177958, -2.682774720514426559, -27.14485409495429380 ) ) ;
#92298 = ORIENTED_EDGE ( 'NONE', *, *, #12415, .T. ) ;
#92299 = EDGE_CURVE ( 'NONE', #45608, #833, #98573, .T. ) ;
#92300 = CARTESIAN_POINT ( 'NONE',  ( -66.62287095715005592, -24.64898659630367916, 1.056161002820824368 ) ) ;
#92301 = PLANE ( 'NONE',  #1009 ) ;
#92302 = CARTESIAN_POINT ( 'NONE',  ( 16.53012286974688294, -13.99140274789385252, -1.500000000000002220 ) ) ;
#92303 = CARTESIAN_POINT ( 'NONE',  ( -29.62287095715005592, -24.42708174548585731, 9.387659993670769865 ) ) ;
#92304 = CARTESIAN_POINT ( 'NONE',  ( -17.77321681866180469, -7.816401696202086136, -1.500000000000002220 ) ) ;
#92305 = CARTESIAN_POINT ( 'NONE',  ( -82.52287095715006160, -23.48786465467241058, 11.44779295918254469 ) ) ;
#92306 = CARTESIAN_POINT ( 'NONE',  ( -35.62287095715004881, -23.48783264082477729, -1.443836473390072372 ) ) ;
#92307 = CARTESIAN_POINT ( 'NONE',  ( -4.880483578727112359, 19.22116399702514045, -1.500000000000002220 ) ) ;
#92308 = B_SPLINE_CURVE_WITH_KNOTS ( 'NONE', 3,
 ( #88170, #64355, #26764, #72948 ),
 .UNSPECIFIED., .F., .F.,
 ( 4, 4 ),
 ( 0.000000000000000000, 9.999999999999592548E-05 ),
 .UNSPECIFIED. ) ;
#92309 = ORIENTED_EDGE ( 'NONE', *, *, #22888, .T. ) ;
#92310 = CARTESIAN_POINT ( 'NONE',  ( 13.61570878652767291, 15.11107311891478666, 11.49999999999999645 ) ) ;
#92311 = CARTESIAN_POINT ( 'NONE',  ( -80.58925929066886340, -24.52300882791530157, 0.6510814631126378149 ) ) ;
#92312 = CARTESIAN_POINT ( 'NONE',  ( -123.6228709571500559, -29.50248528299804818, 1.056150453629045360 ) ) ;
#92313 = EDGE_LOOP ( 'NONE', ( #93462, #24940, #30116, #37158 ) ) ;
#92314 = B_SPLINE_SURFACE_WITH_KNOTS ( 'NONE', 3, 3, ( 
 ( #64545, #48294, #25445, #32055 ),
 ( #63028, #56421, #24439, #26459 ),
 ( #48804, #57423, #79727, #95456 ),
 ( #55410, #41181, #86349, #72138 ),
 ( #2625, #87852, #80235, #88352 ),
 ( #16831, #10729, #41693, #34071 ),
 ( #97939, #74126, #59910, #36550 ) ),
 .UNSPECIFIED., .F., .F., .F.,
 ( 4, 3, 4 ),
 ( 4, 4 ),
 ( 0.3389043340504380719, 0.5146335846998003616, 0.6903628353491626513 ),
 ( 0.2860456367239210818, 0.3169887994066197812 ),
 .UNSPECIFIED. ) ;
#92315 = CARTESIAN_POINT ( 'NONE',  ( -105.5228709571500758, -29.50248528299804818, 1.056150453629043584 ) ) ;
#92316 = CARTESIAN_POINT ( 'NONE',  ( -8.160000000000000142, 1.682056942681651179, 5.192823660268256702 ) ) ;
#92317 = CARTESIAN_POINT ( 'NONE',  ( -49.03252113942349411, -25.31601947462323920, 5.540384453209895810 ) ) ;
#92318 = CARTESIAN_POINT ( 'NONE',  ( -40.49851917831725245, -24.15602025860895097, 10.28564288303536856 ) ) ;
#92319 = CARTESIAN_POINT ( 'NONE',  ( -128.6228709571500417, -29.50250243563736774, 8.947779886222132717 ) ) ;
#92320 = CARTESIAN_POINT ( 'NONE',  ( -17.52916707085001136, 9.785066945116392745, -1.500000000000002220 ) ) ;
#92321 = DIRECTION ( 'NONE',  ( -1.000000000000000000, -0.000000000000000000, -5.238131417152343399E-15 ) ) ;
#92322 = EDGE_LOOP ( 'NONE', ( #57232, #64845, #1079, #9780 ) ) ;
#92323 = CARTESIAN_POINT ( 'NONE',  ( -91.62287095715004170, -24.66019654487199730, 8.947790411086124607 ) ) ;
#92324 = CARTESIAN_POINT ( 'NONE',  ( -19.55383134093860420, 11.88776249338449986, 11.49999999999999645 ) ) ;
#92325 = CARTESIAN_POINT ( 'NONE',  ( -17.66434017299383896, 14.31182286555179139, -1.500000000000002220 ) ) ;
#92326 = CARTESIAN_POINT ( 'NONE',  ( -50.16163650206989644, -25.26258880167387488, 4.712129156570222577 ) ) ;
#92327 = DIRECTION ( 'NONE',  ( -3.773278334453079618E-23, 0.9999999999976377785, 2.173523156925979975E-06 ) ) ;
#92328 = CARTESIAN_POINT ( 'NONE',  ( -31.24388727629347784, -24.87219037989215309, 1.747789950310770779 ) ) ;
#92329 = CARTESIAN_POINT ( 'NONE',  ( -17.97250661212648026, 5.965225279485594001, -23.43622901028613015 ) ) ;
#92330 = CIRCLE ( 'NONE', #58828, 20.00000000000000000 ) ;
#92331 = CARTESIAN_POINT ( 'NONE',  ( 33.00535138976592719, 3.570691370340881576, -12.97242311383975988 ) ) ;
#92332 = ADVANCED_FACE ( 'NONE', ( #15830 ), #70128, .T. ) ;
#92333 = CARTESIAN_POINT ( 'NONE',  ( -101.5228709571500758, -29.50250243563736774, 8.947779886222138046 ) ) ;
#92334 = ORIENTED_EDGE ( 'NONE', *, *, #32240, .F. ) ;
#92335 = AXIS2_PLACEMENT_3D ( 'NONE', #37695, #53933, #21950 ) ;
#92336 = CARTESIAN_POINT ( 'NONE',  ( 14.56535739210195857, -14.21638276092092745, -1.500000000000002220 ) ) ;
#92337 = ORIENTED_EDGE ( 'NONE', *, *, #86902, .F. ) ;
#92338 = CARTESIAN_POINT ( 'NONE',  ( -7.281717392095591102, 21.80608952751712692, -1.500000000000002220 ) ) ;
#92339 = FACE_OUTER_BOUND ( 'NONE', #51070, .T. ) ;
#92340 = ORIENTED_EDGE ( 'NONE', *, *, #90775, .T. ) ;
#92341 = AXIS2_PLACEMENT_3D ( 'NONE', #3048, #32991, #57345 ) ;
#92342 = FACE_OUTER_BOUND ( 'NONE', #12518, .T. ) ;
#92343 = DIRECTION ( 'NONE',  ( 0.000000000000000000, 1.000000000000000000, 0.000000000000000000 ) ) ;
#92344 = VECTOR ( 'NONE', #18358, 1000.000000000000114 ) ;
#92345 = CARTESIAN_POINT ( 'NONE',  ( -40.62287095715004881, -24.14321612903114556, -0.2833117244521690670 ) ) ;
#92347 = VERTEX_POINT ( 'NONE', #70629 ) ;
#92346 = CARTESIAN_POINT ( 'NONE',  ( 0.1273799443098547757, 21.28700333820561497, 11.49999999999999645 ) ) ;
#92348 = CIRCLE ( 'NONE', #19420, 1.530000000000000249 ) ;
#92349 = ORIENTED_EDGE ( 'NONE', *, *, #42932, .T. ) ;
#92350 = CARTESIAN_POINT ( 'NONE',  ( 12.10043277420606778, 18.60588626676543100, 11.49999999999998934 ) ) ;
#92351 = CARTESIAN_POINT ( 'NONE',  ( 1.647368763193059582, 20.57021071130147405, 11.49999999999998934 ) ) ;
#92352 = EDGE_CURVE ( 'NONE', #38564, #46308, #7831, .T. ) ;
#92354 = EDGE_LOOP ( 'NONE', ( #4905, #49237, #5157, #64787 ) ) ;
#92353 = CIRCLE ( 'NONE', #27549, 15.00000000000000178 ) ;
#92355 = VERTEX_POINT ( 'NONE', #1125 ) ;
#92356 = CARTESIAN_POINT ( 'NONE',  ( -109.1951039547969202, -25.31627293009379187, 4.973673916210892720 ) ) ;
#92357 = CARTESIAN_POINT ( 'NONE',  ( -56.62287095715006302, -24.51283580621364777, 0.6167428607019728171 ) ) ;
#92358 = ORIENTED_EDGE ( 'NONE', *, *, #69473, .T. ) ;
#92359 = LINE ( 'NONE', #93355, #52628 ) ;
#92360 = ADVANCED_FACE ( 'NONE', ( #16839 ), #84199, .T. ) ;
#92361 = ORIENTED_EDGE ( 'NONE', *, *, #16891, .T. ) ;
#92362 = CARTESIAN_POINT ( 'NONE',  ( -126.1692044365139225, -25.21250203164489889, 3.500954016957966264 ) ) ;
#92363 = CARTESIAN_POINT ( 'NONE',  ( -44.52287095715006160, -24.50216790748204332, 0.6166512839542455104 ) ) ;
#92364 = CARTESIAN_POINT ( 'NONE',  ( 18.03836333725549324, -10.36167025447706713, -1.500000000000002220 ) ) ;
#92365 = CARTESIAN_POINT ( 'NONE',  ( -19.96617879207914825, 8.700599545123990808, 11.49999999999999645 ) ) ;
#92366 = CARTESIAN_POINT ( 'NONE',  ( 26.51161204093744317, -5.098805221225331863, -7.190516857961198660 ) ) ;
#92367 = CARTESIAN_POINT ( 'NONE',  ( 4.621320343559255583, 11.49999999999999645, 2.100000000000000089 ) ) ;
#92368 = CARTESIAN_POINT ( 'NONE',  ( -19.72384299526936857, -10.77339039931002773, 11.49999999999998934 ) ) ;
#92369 = EDGE_CURVE ( 'NONE', #52199, #67682, #11724, .T. ) ;
#92370 = EDGE_CURVE ( 'NONE', #82958, #28190, #69484, .T. ) ;
#92371 = CARTESIAN_POINT ( 'NONE',  ( -9.543201319291914093E-14, -5.876774720514426953, 18.21871304725679508 ) ) ;
#92372 = ORIENTED_EDGE ( 'NONE', *, *, #65642, .T. ) ;
#92373 = CYLINDRICAL_SURFACE ( 'NONE', #87427, 0.3000000000000016542 ) ;
#92374 = CARTESIAN_POINT ( 'NONE',  ( 32.64853395142472436, 3.736174708400741729, -2.687157883629963884 ) ) ;
#92375 = EDGE_CURVE ( 'NONE', #34336, #15522, #52592, .T. ) ;
#92376 = ORIENTED_EDGE ( 'NONE', *, *, #75381, .F. ) ;
#92377 = VERTEX_POINT ( 'NONE', #97467 ) ;
#92378 = VERTEX_POINT ( 'NONE', #27956 ) ;
#92379 = CARTESIAN_POINT ( 'NONE',  ( 0.2649960030224881025, 21.33594185153759426, -1.500000000000002220 ) ) ;
#92380 = ORIENTED_EDGE ( 'NONE', *, *, #50241, .F. ) ;
#92381 = CARTESIAN_POINT ( 'NONE',  ( 16.43158684610488862, 13.14696595092960152, 11.49999999999998934 ) ) ;
#92382 = CARTESIAN_POINT ( 'NONE',  ( -30.57655055308772418, -25.31557562294173280, 3.857144010898052588 ) ) ;
#92383 = CARTESIAN_POINT ( 'NONE',  ( -100.0133086385735908, -25.19440624866216893, 3.361853740790277989 ) ) ;
#92384 = CARTESIAN_POINT ( 'NONE',  ( -29.49875734969025842, 5.965225279485572685, 25.61802280011862720 ) ) ;
#92385 = CARTESIAN_POINT ( 'NONE',  ( 21.30657626330824783, 5.479626006175059239, -1.500000000000002220 ) ) ;
#92386 = CARTESIAN_POINT ( 'NONE',  ( -39.52287095715004739, -23.73907113216988307, -1.053371485793256124 ) ) ;
#92387 = ORIENTED_EDGE ( 'NONE', *, *, #37526, .F. ) ;
#92388 = DIRECTION ( 'NONE',  ( 0.6599726524652352877, 0.000000000000000000, -0.7512896232465891000 ) ) ;
#92389 = EDGE_CURVE ( 'NONE', #32935, #15956, #39278, .T. ) ;
#92390 = CARTESIAN_POINT ( 'NONE',  ( -55.52287095715008292, -23.47593901973090169, -1.443836447538997092 ) ) ;
#92391 = CARTESIAN_POINT ( 'NONE',  ( -84.64007757551536315, -23.73791477778912196, 11.05961554403170588 ) ) ;
#92392 = CARTESIAN_POINT ( 'NONE',  ( -106.5228709571500758, -29.50250243563736774, 8.947779886222136270 ) ) ;
#92393 = CARTESIAN_POINT ( 'NONE',  ( -10.20960514438541011, -23.56704696218565687, 7.291654623549827186 ) ) ;
#92394 = CARTESIAN_POINT ( 'NONE',  ( 6.245503531335690361, -20.37428601906679759, -1.500000000000002220 ) ) ;
#92395 = CARTESIAN_POINT ( 'NONE',  ( -46.52287095715006160, -23.48786465467241058, 11.44779295918255002 ) ) ;
#92396 = CARTESIAN_POINT ( 'NONE',  ( -107.5162098792497858, -24.15620529776628800, 10.23563542870659759 ) ) ;
#92397 = AXIS2_PLACEMENT_3D ( 'NONE', #11251, #57946, #44207 ) ;
#92398 = EDGE_CURVE ( 'NONE', #20987, #70270, #58913, .T. ) ;
#92399 = CARTESIAN_POINT ( 'NONE',  ( -70.52287095715007581, -24.99132157543166599, 2.256160258750667502 ) ) ;
#92400 = CARTESIAN_POINT ( 'NONE',  ( 3.433349652534986696, 22.22849440524942111, -1.500000000000002220 ) ) ;
#92401 = ADVANCED_FACE ( 'NONE', ( #37063 ), #22320, .F. ) ;
#92402 = CARTESIAN_POINT ( 'NONE',  ( -111.9715540114818566, -25.25626643526282322, 3.571638612575482874 ) ) ;
#92403 = ORIENTED_EDGE ( 'NONE', *, *, #55709, .T. ) ;
#92404 = CARTESIAN_POINT ( 'NONE',  ( -119.5562042904834072, -24.65952944569305316, 1.056160979905705677 ) ) ;
#92405 = CARTESIAN_POINT ( 'NONE',  ( 19.58216393897113505, 1.562425146961006650, 11.49999999999999645 ) ) ;
#92406 = CARTESIAN_POINT ( 'NONE',  ( 9.478389368232452483, 4.132774720514426292, -23.17485683983816003 ) ) ;
#92407 = CARTESIAN_POINT ( 'NONE',  ( -100.6228709571500701, -24.62285846362215835, 9.038163152653526211 ) ) ;
#92408 = ORIENTED_EDGE ( 'NONE', *, *, #43736, .F. ) ;
#92409 = ADVANCED_FACE ( 'NONE', ( #99940 ), #99567, .T. ) ;
#92410 = CARTESIAN_POINT ( 'NONE',  ( -88.50802900976825072, -24.35071581493543746, 9.817618358456025263 ) ) ;
#92411 = CARTESIAN_POINT ( 'NONE',  ( -36.52287095715006160, -24.50321055353803601, 9.387540953477518713 ) ) ;
#92412 = CARTESIAN_POINT ( 'NONE',  ( -89.90102583468038233, -25.31476272485208057, 5.144091107239471938 ) ) ;
#92413 = EDGE_CURVE ( 'NONE', #95239, #22543, #61502, .T. ) ;
#92414 = CARTESIAN_POINT ( 'NONE',  ( -5.084378373094740944, 19.06436389234985285, -1.500000000000002220 ) ) ;
#92415 = EDGE_CURVE ( 'NONE', #88543, #28216, #53298, .T. ) ;
#92416 = AXIS2_PLACEMENT_3D ( 'NONE', #11511, #10515, #66328 ) ;
#92417 = ORIENTED_EDGE ( 'NONE', *, *, #74081, .F. ) ;
#92418 = AXIS2_PLACEMENT_3D ( 'NONE', #64934, #43073, #11113 ) ;
#92419 = CARTESIAN_POINT ( 'NONE',  ( 6.310942340984578180, 6.376774720514426953, -25.29254520177807208 ) ) ;
#92420 = PLANE ( 'NONE',  #90146 ) ;
#92421 = VECTOR ( 'NONE', #12046, 1000.000000000000114 ) ;
#92422 = B_SPLINE_CURVE_WITH_KNOTS ( 'NONE', 3,
 ( #30085, #14353, #45331, #77741 ),
 .UNSPECIFIED., .F., .F.,
 ( 4, 4 ),
 ( 0.000000000000000000, 9.999999999998897304E-05 ),
 .UNSPECIFIED. ) ;
#92423 = DATE_AND_TIME ( #93420, #45774 ) ;
#92424 = ORIENTED_EDGE ( 'NONE', *, *, #52677, .F. ) ;
#92425 = LINE ( 'NONE', #100016, #37025 ) ;
#92426 = DIRECTION ( 'NONE',  ( -0.7512896232465891000, 0.000000000000000000, -0.6599726524652351767 ) ) ;
#92427 = CARTESIAN_POINT ( 'NONE',  ( -81.61611000704998276, -25.23679622552714008, 6.293943003980941420 ) ) ;
#92428 = CARTESIAN_POINT ( 'NONE',  ( -1.044871794871790938, -6.376774720514427841, 21.75000000000000355 ) ) ;
#92429 = CARTESIAN_POINT ( 'NONE',  ( -1.390986686320385468, -5.876774720514414518, 19.62288733224860948 ) ) ;
#92430 = CARTESIAN_POINT ( 'NONE',  ( -58.92287095715003886, -23.47593901973090169, -1.443836447538997758 ) ) ;
#92431 = CARTESIAN_POINT ( 'NONE',  ( -30.64752034897746924, -23.47593901973090169, -1.443836447538997758 ) ) ;
#92432 = CARTESIAN_POINT ( 'NONE',  ( 1.534201407001029027, 19.92515851932037663, 11.49999999999998934 ) ) ;
#92433 = CARTESIAN_POINT ( 'NONE',  ( -95.52287095715010423, -25.00182538069145366, 7.747789668545101982 ) ) ;
#92434 = CARTESIAN_POINT ( 'NONE',  ( -45.57564872872666939, -24.92592662359561118, 8.075495903018000021 ) ) ;
#92435 = VERTEX_POINT ( 'NONE', #45189 ) ;
#92436 = CARTESIAN_POINT ( 'NONE',  ( -8.160000000000000142, -5.907068460905240411E-16, 5.788828319098143105 ) ) ;
#92437 = CARTESIAN_POINT ( 'NONE',  ( -109.7896840091628832, -25.29012758118892634, 3.444317882821586796 ) ) ;
#92438 = DIRECTION ( 'NONE',  ( 0.000000000000000000, -0.9999999999976377785, -2.173523156925979128E-06 ) ) ;
#92439 = CARTESIAN_POINT ( 'NONE',  ( -101.6814946224345704, -25.25287247409163527, 6.236250661346386615 ) ) ;
#92440 = LINE ( 'NONE', #61520, #83679 ) ;
#92441 = B_SPLINE_CURVE_WITH_KNOTS ( 'NONE', 3,
 ( #18373, #48838, #88896, #56954, #80272, #95998 ),
 .UNSPECIFIED., .F., .F.,
 ( 4, 2, 4 ),
 ( 1.570755371633915156E-05, 0.001396183895866088620, 0.002776660238015838181 ),
 .UNSPECIFIED. ) ;
#92442 = LINE ( 'NONE', #24936, #35637 ) ;
#92443 = DIRECTION ( 'NONE',  ( -1.000000000000000000, 0.000000000000000000, 0.000000000000000000 ) ) ;
#92444 = CARTESIAN_POINT ( 'NONE',  ( -40.52287095715006870, -23.47596703998600631, 11.44779298504229281 ) ) ;
#92445 = VERTEX_POINT ( 'NONE', #76113 ) ;
#92446 = CARTESIAN_POINT ( 'NONE',  ( 3.949161919925879172, -19.86910077469890723, 11.49999999999998934 ) ) ;
#92447 = CARTESIAN_POINT ( 'NONE',  ( -90.55620429048337883, -23.48783264082478084, -1.443836473390064157 ) ) ;
#92448 = LINE ( 'NONE', #15322, #93880 ) ;
#92449 = CARTESIAN_POINT ( 'NONE',  ( 282.9764569301858046, 5.965225279485572685, 20.79159422840526616 ) ) ;
#92450 = VERTEX_POINT ( 'NONE', #5115 ) ;
#92451 = CARTESIAN_POINT ( 'NONE',  ( -105.6228709571500559, -29.50250243563736774, 8.947779886222136270 ) ) ;
#92452 = CARTESIAN_POINT ( 'NONE',  ( 19.08902475966321788, 6.433202353099247262, -1.500000000000002220 ) ) ;
#92453 = CARTESIAN_POINT ( 'NONE',  ( -21.07084664159375009, 0.3847054351051909515, 11.49999999999999645 ) ) ;
#92454 = CARTESIAN_POINT ( 'NONE',  ( 6.499999999999992895, 2.239999999999996660, 2.100000000000000977 ) ) ;
#92455 = CARTESIAN_POINT ( 'NONE',  ( 21.87352179494074633, -3.179377960941109915, 11.49999999999998934 ) ) ;
#92456 = AXIS2_PLACEMENT_3D ( 'NONE', #58693, #97747, #98741 ) ;
#92457 = CARTESIAN_POINT ( 'NONE',  ( 19.76637988705548210, 5.604140092158477415, -1.500000000000002220 ) ) ;
#92458 = LINE ( 'NONE', #30569, #51167 ) ;
#92459 = EDGE_CURVE ( 'NONE', #76499, #45115, #57464, .T. ) ;
#92460 = CARTESIAN_POINT ( 'NONE',  ( -53.62287095715003460, -23.73907113216990084, -1.053371485793234807 ) ) ;
#92461 = ORIENTED_EDGE ( 'NONE', *, *, #41569, .F. ) ;
#92462 = DIRECTION ( 'NONE',  ( -0.4771587602595987465, -0.8788171126619706008, 0.000000000000000000 ) ) ;
#92463 = ORIENTED_EDGE ( 'NONE', *, *, #12338, .T. ) ;
#92464 = CARTESIAN_POINT ( 'NONE',  ( -126.6228709571500275, -23.48783264082479505, -1.443836473390057051 ) ) ;
#92465 = CARTESIAN_POINT ( 'NONE',  ( -130.2562042904833959, -23.47596703998600631, 11.44779298504227860 ) ) ;
#92466 = ORIENTED_EDGE ( 'NONE', *, *, #42264, .F. ) ;
#92467 = VERTEX_POINT ( 'NONE', #22817 ) ;
#92468 = ORIENTED_EDGE ( 'NONE', *, *, #70456, .F. ) ;
#92469 = PLANE ( 'NONE',  #92335 ) ;
#92470 = CARTESIAN_POINT ( 'NONE',  ( -5.366453405989236813, 2.247226876435393361E-15, -18.35000000000000142 ) ) ;
#92471 = CARTESIAN_POINT ( 'NONE',  ( -68.50595449436075057, -24.15620529776627734, 10.23563542870660825 ) ) ;
#92472 = CARTESIAN_POINT ( 'NONE',  ( 20.50092990308456464, -2.467789585553555654, -1.500000000000002220 ) ) ;
#92473 = CARTESIAN_POINT ( 'NONE',  ( 21.32721141102669193, -3.434809268862642817, 11.49999999999999645 ) ) ;
#92474 = ORIENTED_EDGE ( 'NONE', *, *, #21348, .F. ) ;
#92475 = EDGE_CURVE ( 'NONE', #922, #76871, #64660, .T. ) ;
#92476 = DIRECTION ( 'NONE',  ( 1.000000000000000000, 1.232047923278981953E-16, 0.000000000000000000 ) ) ;
#92477 = CARTESIAN_POINT ( 'NONE',  ( 3.475076759263674209, -5.876774720514402084, 18.20843037655054530 ) ) ;
#92478 = CARTESIAN_POINT ( 'NONE',  ( -11.14805103425725719, -19.39388463112642214, -1.500000000000002220 ) ) ;
#92479 = EDGE_CURVE ( 'NONE', #88312, #80762, #21129, .T. ) ;
#92480 = EDGE_CURVE ( 'NONE', #66723, #3925, #93737, .T. ) ;
#92481 = CARTESIAN_POINT ( 'NONE',  ( -80.48900664166535535, -25.12205811808326672, 7.101635561061091728 ) ) ;
#92482 = CARTESIAN_POINT ( 'NONE',  ( -75.52287095715007581, -23.47596703998600631, 11.44779298504228571 ) ) ;
#92483 = ORIENTED_EDGE ( 'NONE', *, *, #40878, .T. ) ;
#92484 = B_SPLINE_CURVE_WITH_KNOTS ( 'NONE', 3,
 ( #77033, #79039, #17145, #92263, #9534, #71449 ),
 .UNSPECIFIED., .F., .F.,
 ( 4, 2, 4 ),
 ( 0.000000000000000000, 0.5000000000000000000, 1.000000000000000000 ),
 .UNSPECIFIED. ) ;
#92485 = CARTESIAN_POINT ( 'NONE',  ( -116.4728709571500360, -25.40558663563427189, 5.000950442582703381 ) ) ;
#92486 = VECTOR ( 'NONE', #43383, 1000.000000000000000 ) ;
#92487 = CARTESIAN_POINT ( 'NONE',  ( -49.50709656002590719, -23.96169478059712432, 10.65365249895718414 ) ) ;
#92489 = ADVANCED_FACE ( 'NONE', ( #69522 ), #2395, .T. ) ;
#92488 = VECTOR ( 'NONE', #31470, 1000.000000000000000 ) ;
#92490 = DIRECTION ( 'NONE',  ( 1.000000000000000000, 0.000000000000000000, 0.000000000000000000 ) ) ;
#92491 = CARTESIAN_POINT ( 'NONE',  ( -16.13976855045889636, 13.32451261336467496, -1.500000000000002220 ) ) ;
#92492 = ORIENTED_EDGE ( 'NONE', *, *, #59899, .T. ) ;
#92493 = CARTESIAN_POINT ( 'NONE',  ( -86.50736880509799676, -24.34968618360934300, 0.1864209137778916336 ) ) ;
#92494 = ORIENTED_EDGE ( 'NONE', *, *, #24007, .T. ) ;
#92495 = CARTESIAN_POINT ( 'NONE',  ( -128.6228709571499849, -24.50321055353805733, 9.387540953477527594 ) ) ;
#92496 = CARTESIAN_POINT ( 'NONE',  ( 20.46717832272283033, -5.532298862796615424, -1.500000000000002220 ) ) ;
#92497 = VERTEX_POINT ( 'NONE', #30949 ) ;
#92498 = CARTESIAN_POINT ( 'NONE',  ( -60.55620429048339304, -24.99156044556202261, 7.747789690856174083 ) ) ;
#92499 = CARTESIAN_POINT ( 'NONE',  ( -35.55620429048339304, -25.00182538069145011, 7.747789668545097541 ) ) ;
#92500 = CARTESIAN_POINT ( 'NONE',  ( -8.334044162642690878, 20.12857247364870616, 11.49999999999998934 ) ) ;
#92501 = CARTESIAN_POINT ( 'NONE',  ( 9.299999999999993605, 12.00000000000002309, 0.000000000000000000 ) ) ;
#92502 = CARTESIAN_POINT ( 'NONE',  ( 0.000000000000000000, -4.132774720514426292, 0.000000000000000000 ) ) ;
#92503 = CARTESIAN_POINT ( 'NONE',  ( 7.480769230769231726, -5.876774720514419847, 20.77403846153845635 ) ) ;
#92504 = CARTESIAN_POINT ( 'NONE',  ( -15.20188179817220231, 15.67080601223297442, -1.500000000000002220 ) ) ;
#92505 = CARTESIAN_POINT ( 'NONE',  ( -71.20541289166536103, -25.24674059646277868, 4.885890097747910943 ) ) ;
#92506 = ORIENTED_EDGE ( 'NONE', *, *, #47264, .F. ) ;
#92507 = CARTESIAN_POINT ( 'NONE',  ( 25.50613189835290484, 5.179663042751369240, -8.021752483163538727 ) ) ;
#92508 = CARTESIAN_POINT ( 'NONE',  ( -123.5895376238167245, -24.65952944569305316, 1.056160979905711894 ) ) ;
#92509 = EDGE_CURVE ( 'NONE', #99597, #14044, #40950, .T. ) ;
#92510 = CARTESIAN_POINT ( 'NONE',  ( 30.93860345374796594, 6.475225279485573360, 20.86760796525322093 ) ) ;
#92511 = ORIENTED_EDGE ( 'NONE', *, *, #39104, .F. ) ;
#92512 = EDGE_LOOP ( 'NONE', ( #65354, #88883, #82659, #60878 ) ) ;
#92513 = EDGE_CURVE ( 'NONE', #46085, #1891, #56662, .T. ) ;
#92514 = ORIENTED_EDGE ( 'NONE', *, *, #62332, .F. ) ;
#92515 = CARTESIAN_POINT ( 'NONE',  ( -44.62287095715004881, -23.94994826722565762, -0.6494450866342738049 ) ) ;
#92516 = CARTESIAN_POINT ( 'NONE',  ( -16.84575021678815432, -12.90291372800108505, 11.49999999999998934 ) ) ;
#92517 = CARTESIAN_POINT ( 'NONE',  ( -94.63995231824821985, -23.48783264082477373, -1.443836473390087249 ) ) ;
#92518 = CARTESIAN_POINT ( 'NONE',  ( -80.29067095681661215, -25.27791970390547860, 7.551389258223609069 ) ) ;
#92519 = EDGE_CURVE ( 'NONE', #5151, #38725, #77611, .T. ) ;
#92520 = CARTESIAN_POINT ( 'NONE',  ( -80.62287095715004170, -25.00182538069145721, 7.747789668545097541 ) ) ;
#92521 = CARTESIAN_POINT ( 'NONE',  ( 10.34999999999999254, 4.999999999999998224, 2.100000000000000089 ) ) ;
#92522 = CARTESIAN_POINT ( 'NONE',  ( -19.24332624019526961, -2.196797614219411443, 11.49999999999998934 ) ) ;
#92523 = CARTESIAN_POINT ( 'NONE',  ( -51.59514189427220288, -25.31187621157931034, 5.320822997074797556 ) ) ;
#92524 = ORIENTED_EDGE ( 'NONE', *, *, #98007, .T. ) ;
#92525 = CARTESIAN_POINT ( 'NONE',  ( -19.30698013599780083, -2.078282243779251637, 11.49999999999999645 ) ) ;
#92526 = CARTESIAN_POINT ( 'NONE',  ( -88.52287095715006160, -24.65952944569304606, 1.056160979905700570 ) ) ;
#92527 = B_SPLINE_CURVE_WITH_KNOTS ( 'NONE', 3,
 ( #85434, #38760, #46889, #69729 ),
 .UNSPECIFIED., .F., .F.,
 ( 4, 4 ),
 ( 1.328512187993866617E-05, 0.002239812633505373039 ),
 .UNSPECIFIED. ) ;
#92528 = CARTESIAN_POINT ( 'NONE',  ( -24.55517127435777169, 5.965225279485592225, -15.44180958690142802 ) ) ;
#92529 = EDGE_LOOP ( 'NONE', ( #45321, #93072, #87408, #53971 ) ) ;
#92530 = DIRECTION ( 'NONE',  ( -0.000000000000000000, -0.000000000000000000, -1.000000000000000000 ) ) ;
#92531 = CARTESIAN_POINT ( 'NONE',  ( -59.52287095715005449, -24.35013146730204525, 9.818937971375108376 ) ) ;
#92533 = EDGE_CURVE ( 'NONE', #80847, #35458, #59786, .T. ) ;
#92532 = CARTESIAN_POINT ( 'NONE',  ( 10.34999999999998010, 22.00000000000000000, 2.100000000000000089 ) ) ;
#92534 = DIRECTION ( 'NONE',  ( 0.000000000000000000, -0.000000000000000000, -1.000000000000000000 ) ) ;
#92535 = CARTESIAN_POINT ( 'NONE',  ( -8.122062702759739850, 17.86989387945112995, 11.49999999999998934 ) ) ;
#92536 = CARTESIAN_POINT ( 'NONE',  ( -41.29362909362059497, -25.27806053428773581, 4.684754197744505078 ) ) ;
#92537 = ORIENTED_EDGE ( 'NONE', *, *, #858, .F. ) ;
#92538 = CARTESIAN_POINT ( 'NONE',  ( 15.64208908530913256, 14.88810259432246852, -1.500000000000002220 ) ) ;
#92539 = DIRECTION ( 'NONE',  ( -0.000000000000000000, -1.000000000000000000, -0.000000000000000000 ) ) ;
#92540 = CARTESIAN_POINT ( 'NONE',  ( -40.62957245546282792, -24.83618233451450052, 1.606449574219539267 ) ) ;
#92542 = ADVANCED_FACE ( 'NONE', ( #62417 ), #93339, .F. ) ;
#92541 = VECTOR ( 'NONE', #37634, 1000.000000000000000 ) ;
#92543 = CARTESIAN_POINT ( 'NONE',  ( 2.230654205607476293, 0.1647943925233646134, -7.514475724998474108E-17 ) ) ;
#92544 = CARTESIAN_POINT ( 'NONE',  ( -11.96207688724106610, 19.68918167733909641, -1.500000000000002220 ) ) ;
#92545 = B_SPLINE_CURVE_WITH_KNOTS ( 'NONE', 3,
 ( #22087, #84000, #14483, #90619 ),
 .UNSPECIFIED., .F., .F.,
 ( 4, 4 ),
 ( 0.000000000000000000, 0.0001000000000000028644 ),
 .UNSPECIFIED. ) ;
#92546 = PERSON_AND_ORGANIZATION ( #70597, #27821 ) ;
#92547 = CARTESIAN_POINT ( 'NONE',  ( -55.62287095715004170, -23.47596703998600631, 11.44779298504227505 ) ) ;
#92548 = CARTESIAN_POINT ( 'NONE',  ( 4.329581153495547063, -6.376774720514422512, 21.24220543808225869 ) ) ;
#92549 = CARTESIAN_POINT ( 'NONE',  ( -121.5901295846091585, -24.15620529776628445, 10.23563542870660115 ) ) ;
#92550 = CARTESIAN_POINT ( 'NONE',  ( -29.49975734969026320, 6.475225279485571583, 13.17908622612278435 ) ) ;
#92551 = CARTESIAN_POINT ( 'NONE',  ( -111.4457194297752807, -25.10921488884410735, 3.361189062929010429 ) ) ;
#92552 = CARTESIAN_POINT ( 'NONE',  ( 32.88562546571908740, -6.376774720514426953, -5.083907541707153754 ) ) ;
#92553 = FACE_OUTER_BOUND ( 'NONE', #92529, .T. ) ;
#92554 = CARTESIAN_POINT ( 'NONE',  ( 8.615496892348360802, 17.92367856960711947, 11.49999999999998934 ) ) ;
#92555 = CARTESIAN_POINT ( 'NONE',  ( -101.3738023147422780, -25.27307239909452008, 3.986250617436227550 ) ) ;
#92556 = CARTESIAN_POINT ( 'NONE',  ( 12.93213199337649044, -14.99640713134888692, -1.500000000000002220 ) ) ;
#92557 = CARTESIAN_POINT ( 'NONE',  ( -56.57855137815445090, -24.65952944569304250, 1.056160979905696795 ) ) ;
#92558 = VECTOR ( 'NONE', #17294, 1000.000000000000000 ) ;
#92559 = CARTESIAN_POINT ( 'NONE',  ( -108.6228709571500559, -24.64898659630368627, 1.056161002820831474 ) ) ;
#92560 = PLANE ( 'NONE',  #36194 ) ;
#92561 = CARTESIAN_POINT ( 'NONE',  ( -1.268444833121266546, 20.69640364028325052, 11.49999999999999645 ) ) ;
#92562 = LINE ( 'NONE', #47906, #79126 ) ;
#92563 = FACE_OUTER_BOUND ( 'NONE', #96727, .T. ) ;
#92564 = CARTESIAN_POINT ( 'NONE',  ( -2.780358639097238349, 22.57001311929844434, 11.49999999999999645 ) ) ;
#92565 = ORIENTED_EDGE ( 'NONE', *, *, #56467, .F. ) ;
#92566 = CARTESIAN_POINT ( 'NONE',  ( -60.62287095715004170, -24.92579138211020862, 1.929029949965662238 ) ) ;
#92567 = CARTESIAN_POINT ( 'NONE',  ( -52.55620429048338593, -23.47596703998600276, 11.44779298504227505 ) ) ;
#92568 = CARTESIAN_POINT ( 'NONE',  ( 20.19498477198788322, 0.2509159868347127231, -1.500000000000002220 ) ) ;
#92569 = DIRECTION ( 'NONE',  ( 0.000000000000000000, 2.173523156925980399E-06, -0.9999999999976378895 ) ) ;
#92570 = CARTESIAN_POINT ( 'NONE',  ( -45.55620429048339304, -23.48786465467240347, 11.44779295918255002 ) ) ;
#92571 = ORIENTED_EDGE ( 'NONE', *, *, #92652, .T. ) ;
#92572 = B_SPLINE_CURVE_WITH_KNOTS ( 'NONE', 3,
 ( #93593, #15970, #46435, #76369, #22082, #45949, #38315, #61679 ),
 .UNSPECIFIED., .F., .F.,
 ( 4, 2, 2, 4 ),
 ( -0.001224554619866348015, -0.0002241820295893690029, 0.0007761905606876100087, 0.002776935741241576706 ),
 .UNSPECIFIED. ) ;
#92573 = ORIENTED_EDGE ( 'NONE', *, *, #25317, .T. ) ;
#92574 = CARTESIAN_POINT ( 'NONE',  ( 0.09189959430841809773, -6.376774720514410077, 19.67013632031035542 ) ) ;
#92575 = CARTESIAN_POINT ( 'NONE',  ( 2.875404258304424143, 22.71175023210845012, 11.49999999999998934 ) ) ;
#92576 = CARTESIAN_POINT ( 'NONE',  ( -50.58832339509404363, -25.18439652211503699, 3.304980435165238983 ) ) ;
#92577 = CARTESIAN_POINT ( 'NONE',  ( -19.98381242416700587, 8.274006965216138099, -1.500000000000002220 ) ) ;
#92578 = CARTESIAN_POINT ( 'NONE',  ( -123.6243262789347739, -24.34968618360933945, 0.1864209137778903291 ) ) ;
#92579 = CARTESIAN_POINT ( 'NONE',  ( -34.55279844800535471, -23.96119346886880663, -0.6495511937831991434 ) ) ;
#92580 = CARTESIAN_POINT ( 'NONE',  ( -20.36979505965413395, -4.774807507659313721, 11.49999999999999645 ) ) ;
#92581 = ORIENTED_EDGE ( 'NONE', *, *, #98144, .T. ) ;
#92582 = CARTESIAN_POINT ( 'NONE',  ( -124.6251027437798484, -23.96119346886880308, -0.6495511937832024740 ) ) ;
#92583 = CARTESIAN_POINT ( 'NONE',  ( -20.57682416348112397, 7.868404785394932155, -1.500000000000002220 ) ) ;
#92584 = CARTESIAN_POINT ( 'NONE',  ( -33.52287095715006160, -29.50248528299804818, 1.056150453629029817 ) ) ;
#92585 = DIRECTION ( 'NONE',  ( -3.773278334453079030E-23, 0.9999999999976377785, 2.173523156925979128E-06 ) ) ;
#92586 = ORIENTED_EDGE ( 'NONE', *, *, #81428, .T. ) ;
#92587 = DIRECTION ( 'NONE',  ( -1.334402673828313093E-16, 0.000000000000000000, -1.000000000000000000 ) ) ;
#92588 = CARTESIAN_POINT ( 'NONE',  ( -122.6228709571500417, -23.72773821059536559, 11.05748984161097326 ) ) ;
#92589 = ORIENTED_EDGE ( 'NONE', *, *, #34939, .F. ) ;
#92590 = DIRECTION ( 'NONE',  ( 0.000000000000000000, 0.000000000000000000, -1.000000000000000000 ) ) ;
#92591 = EDGE_CURVE ( 'NONE', #71172, #24828, #61033, .T. ) ;
#92592 = ORIENTED_EDGE ( 'NONE', *, *, #53326, .F. ) ;
#92593 = EDGE_CURVE ( 'NONE', #41731, #43974, #29564, .T. ) ;
#92594 = ORIENTED_EDGE ( 'NONE', *, *, #27030, .F. ) ;
#92595 = CARTESIAN_POINT ( 'NONE',  ( -71.59683312727963767, -23.96169478059713498, 10.65365249895718058 ) ) ;
#92596 = CARTESIAN_POINT ( 'NONE',  ( -83.52287095715006160, -24.64965694238407323, 8.947790433994198267 ) ) ;
#92597 = CARTESIAN_POINT ( 'NONE',  ( -36.62906116432126424, -24.51314013834316086, 0.6176544820404111791 ) ) ;
#92598 = CARTESIAN_POINT ( 'NONE',  ( -19.64171699416042571, -5.764624264842452384, -1.500000000000002220 ) ) ;
#92599 = EDGE_CURVE ( 'NONE', #8718, #33210, #13746, .T. ) ;
#92600 = ORIENTED_EDGE ( 'NONE', *, *, #73662, .F. ) ;
#92601 = CARTESIAN_POINT ( 'NONE',  ( -99.90834851333848121, -25.30148146617204219, 5.319218632498879273 ) ) ;
#92602 = DIRECTION ( 'NONE',  ( 0.000000000000000000, 0.000000000000000000, -1.000000000000000000 ) ) ;
#92603 = CARTESIAN_POINT ( 'NONE',  ( 5.271800844963591359, 3.316774720514426456, -28.56638892015329745 ) ) ;
#92604 = CARTESIAN_POINT ( 'NONE',  ( -21.97457344801873447, 3.670769625195870134, 11.49999999999998934 ) ) ;
#92605 = EDGE_CURVE ( 'NONE', #53799, #74504, #85828, .T. ) ;
#92606 = CARTESIAN_POINT ( 'NONE',  ( -79.11611000704996854, -25.20074463982482982, 3.409327697717700278 ) ) ;
#92607 = CARTESIAN_POINT ( 'NONE',  ( -8.134552738279960948, 10.05242149336743296, -0.8794729216540254635 ) ) ;
#92608 = ORIENTED_EDGE ( 'NONE', *, *, #20555, .F. ) ;
#92609 = LINE ( 'NONE', #16988, #48487 ) ;
#92610 = CARTESIAN_POINT ( 'NONE',  ( -29.60812400815161283, -25.26247736358755702, 6.685403929990477501 ) ) ;
#92611 = CARTESIAN_POINT ( 'NONE',  ( -20.74012505511919713, -1.853331690952414013, -1.500000000000002220 ) ) ;
#92612 = AXIS2_PLACEMENT_3D ( 'NONE', #68352, #22647, #54138 ) ;
#92613 = ORIENTED_EDGE ( 'NONE', *, *, #43739, .T. ) ;
#92615 = ORIENTED_EDGE ( 'NONE', *, *, #26163, .T. ) ;
#92614 = CARTESIAN_POINT ( 'NONE',  ( 4.593956459244529889, -6.376774720514410077, 19.29001220640957115 ) ) ;
#92617 = EDGE_CURVE ( 'NONE', #58438, #67443, #35343, .T. ) ;
#92616 = CARTESIAN_POINT ( 'NONE',  ( -50.71600500446225368, -25.12217856757505530, 7.074609049370240044 ) ) ;
#92618 = ORIENTED_EDGE ( 'NONE', *, *, #66394, .F. ) ;
#92619 = ORIENTED_EDGE ( 'NONE', *, *, #2081, .F. ) ;
#92620 = CARTESIAN_POINT ( 'NONE',  ( 1.600000000000000755, 0.000000000000000000, 0.000000000000000000 ) ) ;
#92621 = CARTESIAN_POINT ( 'NONE',  ( 3.797776442307698286, -6.376774720514427841, 21.83974358974358410 ) ) ;
#92622 = B_SPLINE_CURVE_WITH_KNOTS ( 'NONE', 3,
 ( #14527, #61231, #84541, #85539 ),
 .UNSPECIFIED., .F., .F.,
 ( 4, 4 ),
 ( 0.03981435493391547592, 0.04882078620603082231 ),
 .UNSPECIFIED. ) ;
#92623 = APPLICATION_CONTEXT ( 'configuration controlled 3d designs of mechanical parts and assemblies' ) ;
#92624 =( BOUNDED_SURFACE ( )  B_SPLINE_SURFACE ( 3, 1, ( 
 ( #72602, #47762 ),
 ( #10192, #56888 ),
 ( #87819, #79696 ),
 ( #72106, #26420 ) ),
 .UNSPECIFIED., .F., .F., .T. ) 
 B_SPLINE_SURFACE_WITH_KNOTS ( ( 4, 4 ),
 ( 2, 2 ),
 ( 0.000000000000000000, 1.000000000000000000 ),
 ( 0.000000000000000000, 1.000000000000000000 ),
 .UNSPECIFIED. ) 
 GEOMETRIC_REPRESENTATION_ITEM ( )  RATIONAL_B_SPLINE_SURFACE ( (
 ( 1.000000000000000000, 1.000000000000000000),
 ( 0.3333333333333333703, 0.3333333333333333703),
 ( 0.3333333333333333703, 0.3333333333333333703),
 ( 1.000000000000000000, 1.000000000000000000) ) ) 
 REPRESENTATION_ITEM ( '' )  SURFACE ( )  );
#92625 = CARTESIAN_POINT ( 'NONE',  ( 30.00738719773716667, 1.477225279485574028, -9.049252915307089751 ) ) ;
#92626 = DIRECTION ( 'NONE',  ( 0.000000000000000000, -0.7071067811865525687, 0.7071067811865425767 ) ) ;
#92627 = CARTESIAN_POINT ( 'NONE',  ( -92.59761174911608350, -23.73791477778911840, 11.05961554403170588 ) ) ;
#92628 = CARTESIAN_POINT ( 'NONE',  ( -53.58953762381672448, -23.48783264082478084, -1.443836473390070596 ) ) ;
#92630 = VERTEX_POINT ( 'NONE', #59176 ) ;
#92629 = CARTESIAN_POINT ( 'NONE',  ( 18.11909884760711975, -12.84011383348296853, 11.49999999999999645 ) ) ;
#92631 = CARTESIAN_POINT ( 'NONE',  ( -89.49044893904931541, -25.11033443465437287, 2.832404802291436319 ) ) ;
#92632 = ORIENTED_EDGE ( 'NONE', *, *, #34119, .T. ) ;
#92633 = CARTESIAN_POINT ( 'NONE',  ( -6.441999407266626676, 21.70310835763521595, 11.49999999999998934 ) ) ;
#92635 = ORIENTED_EDGE ( 'NONE', *, *, #44571, .T. ) ;
#92634 = CARTESIAN_POINT ( 'NONE',  ( -115.5589197295127946, -23.48786465467241769, 11.44779295918253581 ) ) ;
#92636 = VECTOR ( 'NONE', #12296, 1000.000000000000000 ) ;
#92637 = ORIENTED_EDGE ( 'NONE', *, *, #92864, .F. ) ;
#92638 = APPROVAL_PERSON_ORGANIZATION ( #25033, #7222, #71225 ) ;
#92639 = CARTESIAN_POINT ( 'NONE',  ( -7.662324775236974972, 31.59999999999999787, 2.100000000000000089 ) ) ;
#92640 = CARTESIAN_POINT ( 'NONE',  ( -15.22981678846565856, -13.14137338692033907, -1.500000000000002220 ) ) ;
#92641 = PLANE ( 'NONE',  #26263 ) ;
#92642 = VERTEX_POINT ( 'NONE', #36836 ) ;
#92643 = CARTESIAN_POINT ( 'NONE',  ( -92.52287095715006160, -23.48786465467241769, 11.44779295918254292 ) ) ;
#92644 = CARTESIAN_POINT ( 'NONE',  ( 20.23429811176546167, 9.490607074118958764, -1.500000000000002220 ) ) ;
#92645 = ORIENTED_EDGE ( 'NONE', *, *, #83658, .T. ) ;
#92646 = ORIENTED_EDGE ( 'NONE', *, *, #4902, .T. ) ;
#92647 = PLANE ( 'NONE',  #98429 ) ;
#92648 = CARTESIAN_POINT ( 'NONE',  ( -119.6228709571500559, -24.64965695001469115, 8.947790433994175174 ) ) ;
#92649 = CARTESIAN_POINT ( 'NONE',  ( -4.209565145052936330, 8.865772972990910716, -1.700000000000008837 ) ) ;
#92650 = PLANE ( 'NONE',  #88734 ) ;
#92652 = EDGE_CURVE ( 'NONE', #14697, #45943, #66306, .T. ) ;
#92651 = DIRECTION ( 'NONE',  ( 0.000000000000000000, 0.000000000000000000, -1.000000000000000000 ) ) ;
#92653 = CARTESIAN_POINT ( 'NONE',  ( 10.86043079284791091, -16.25897383129715834, -1.500000000000002220 ) ) ;
#92654 = FACE_OUTER_BOUND ( 'NONE', #98016, .T. ) ;
#92655 = CARTESIAN_POINT ( 'NONE',  ( 19.19993882694861753, 9.668096177433461946, -1.500000000000002220 ) ) ;
#92656 = CARTESIAN_POINT ( 'NONE',  ( -2.732037236150805626, -5.876774720514410077, 19.78976258633487717 ) ) ;
#92657 = CARTESIAN_POINT ( 'NONE',  ( 7.662324775236977636, 31.59999999999999787, 2.100000000000000089 ) ) ;
#92658 = CARTESIAN_POINT ( 'NONE',  ( -129.5228709571500474, -24.66019654487199730, 8.947790411086115725 ) ) ;
#92659 = ADVANCED_FACE ( 'NONE', ( #67799 ), #11491, .F. ) ;
#92660 = FACE_OUTER_BOUND ( 'NONE', #56980, .T. ) ;
#92661 = CARTESIAN_POINT ( 'NONE',  ( 18.88093902437788785, 12.95799798663108682, -1.500000000000002220 ) ) ;
#92662 = VECTOR ( 'NONE', #87537, 1000.000000000000114 ) ;
#92663 = APPROVAL_STATUS ( 'not_yet_approved' ) ;
#92664 = CARTESIAN_POINT ( 'NONE',  ( 0.000000000000000000, -0.3849999999999936806, -1.530000000000001359 ) ) ;
#92665 = CARTESIAN_POINT ( 'NONE',  ( -29.52287095715006160, -24.56560739788454129, 1.056161319240904728 ) ) ;
#92666 = CARTESIAN_POINT ( 'NONE',  ( 3.179702300980958185, 19.78100630842630281, 11.49999999999999645 ) ) ;
#92667 = CARTESIAN_POINT ( 'NONE',  ( -79.09669456484505190, -25.26612537777918632, 5.260500027664780198 ) ) ;
#92668 = CARTESIAN_POINT ( 'NONE',  ( -33.62287095715005592, -23.47596703998600276, 11.44779298504227505 ) ) ;
#92669 = PLANE ( 'NONE',  #24667 ) ;
#92670 = FACE_BOUND ( 'NONE', #67043, .T. ) ;
#92671 = EDGE_LOOP ( 'NONE', ( #34467, #57272, #28743, #94854 ) ) ;
#92672 = PLANE ( 'NONE',  #73666 ) ;
#92673 = CYLINDRICAL_SURFACE ( 'NONE', #28035, 19.30000000000000071 ) ;
#92674 = CARTESIAN_POINT ( 'NONE',  ( -19.25911440464646063, 10.06369110047026538, 11.49999999999998934 ) ) ;
#92675 = DIRECTION ( 'NONE',  ( -0.000000000000000000, -0.000000000000000000, -1.000000000000000000 ) ) ;
#92676 = CARTESIAN_POINT ( 'NONE',  ( -18.23851433863309879, 7.102826447048048664, -1.500000000000002220 ) ) ;
#92677 = PLANE ( 'NONE',  #50794 ) ;
#92678 = DIRECTION ( 'NONE',  ( -0.000000000000000000, -0.000000000000000000, -1.000000000000000000 ) ) ;
#92679 = APPROVAL_ROLE ( '' ) ;
#92680 = CARTESIAN_POINT ( 'NONE',  ( -91.51200254185937411, -24.15620529776628445, 10.23563542870660292 ) ) ;
#92681 = DIRECTION ( 'NONE',  ( 4.218136541796977197E-15, -1.000000000000000000, 1.324960360541890271E-16 ) ) ;
#92682 = CARTESIAN_POINT ( 'NONE',  ( 19.76637988705548210, 5.604140092158477415, 11.49999999999999645 ) ) ;
#92683 = CARTESIAN_POINT ( 'NONE',  ( 30.60443771307607008, 4.296120514312956828, 26.89827953497908908 ) ) ;
#92684 = VECTOR ( 'NONE', #56518, 1000.000000000000000 ) ;
#92685 = CARTESIAN_POINT ( 'NONE',  ( -120.6267774785480356, -24.15503026093913874, -0.2815557561904504791 ) ) ;
#92686 = ORIENTED_EDGE ( 'NONE', *, *, #37414, .T. ) ;
#92687 = CARTESIAN_POINT ( 'NONE',  ( -99.55666892486131303, -25.31296331729878446, 4.188639739155572528 ) ) ;
#92688 = DIRECTION ( 'NONE',  ( -3.773278334444167608E-23, 1.000000000000000000, 0.000000000000000000 ) ) ;
#92689 = CARTESIAN_POINT ( 'NONE',  ( -125.5549464543417884, -24.52399227489127043, 9.353111116836528183 ) ) ;
#92690 = DIRECTION ( 'NONE',  ( 0.000000000000000000, -0.000000000000000000, -1.000000000000000000 ) ) ;
#92691 = CARTESIAN_POINT ( 'NONE',  ( -25.74405688418818272, -24.61459765063332483, 6.647229985634355742 ) ) ;
#92692 = CARTESIAN_POINT ( 'NONE',  ( 31.81388842165050335, 4.825737335974109143, -4.598239840489335428 ) ) ;
#92693 = AXIS2_PLACEMENT_3D ( 'NONE', #77662, #39111, #70065 ) ;
#92694 = CARTESIAN_POINT ( 'NONE',  ( -17.14199295335891904, -15.44578658782692671, 11.49999999999999645 ) ) ;
#92695 = CARTESIAN_POINT ( 'NONE',  ( -0.9063223138645676302, -22.79912562917415997, -1.500000000000002220 ) ) ;
#92696 = CARTESIAN_POINT ( 'NONE',  ( -74.59647204067105974, -23.96119346886880308, -0.6495511937832119109 ) ) ;
#92697 = CARTESIAN_POINT ( 'NONE',  ( -78.62287095715005592, -29.50250243563736774, 8.947779886222141599 ) ) ;
#92698 = CARTESIAN_POINT ( 'NONE',  ( -86.52287095715000476, -23.95044443724992789, 10.65354141964649237 ) ) ;
#92699 = CC_DESIGN_APPROVAL ( #14687, ( #29472 ) ) ;
#92700 = CARTESIAN_POINT ( 'NONE',  ( 18.65981798208652265, 12.38953945867474360, 11.49999999999999645 ) ) ;
#92701 = ORIENTED_EDGE ( 'NONE', *, *, #348, .F. ) ;
#92702 = CARTESIAN_POINT ( 'NONE',  ( -59.56094173781918499, -29.50249039766296022, 3.409318347773680369 ) ) ;
#92703 = CARTESIAN_POINT ( 'NONE',  ( -43.56067006883019843, -23.73766607897671221, -1.055555164236442689 ) ) ;
#92704 = CARTESIAN_POINT ( 'NONE',  ( 17.58553779993395594, 13.13030503331179411, 11.49999999999998934 ) ) ;
#92705 = CARTESIAN_POINT ( 'NONE',  ( -113.5228709571500616, -24.34917612406836795, 0.1852690917426624284 ) ) ;
#92706 = FACE_OUTER_BOUND ( 'NONE', #94987, .T. ) ;
#92707 = CARTESIAN_POINT ( 'NONE',  ( -33.52287095715004739, -23.73934037231756022, 11.05740245334329686 ) ) ;
#92708 = CARTESIAN_POINT ( 'NONE',  ( -69.52287095715006160, -24.64898659630367916, 1.056161002820824368 ) ) ;
#92709 = CARTESIAN_POINT ( 'NONE',  ( -96.92287095715008149, -23.47593901973090169, -1.443836447538996870 ) ) ;
#92710 = ORIENTED_EDGE ( 'NONE', *, *, #71105, .F. ) ;
#92711 = EDGE_CURVE ( 'NONE', #83737, #80766, #60184, .T. ) ;
#92712 = CARTESIAN_POINT ( 'NONE',  ( -4.979992623568794130, 19.86841884474198494, -1.500000000000002220 ) ) ;
#92713 = ORIENTED_EDGE ( 'NONE', *, *, #37752, .F. ) ;
#92714 = ORIENTED_EDGE ( 'NONE', *, *, #11334, .T. ) ;
#92715 = ORIENTED_EDGE ( 'NONE', *, *, #100143, .T. ) ;
#92716 = ORIENTED_EDGE ( 'NONE', *, *, #10623, .F. ) ;
#92717 = CARTESIAN_POINT ( 'NONE',  ( -18.41700849636773540, 13.91914711744011157, 11.49999999999998934 ) ) ;
#92718 = CARTESIAN_POINT ( 'NONE',  ( -40.11481023079474539, -25.30977039686255026, 4.487062071701387822 ) ) ;
#92719 = CARTESIAN_POINT ( 'NONE',  ( -20.02346298389695534, -3.155783441878276196, -1.500000000000002220 ) ) ;
#92720 = EDGE_CURVE ( 'NONE', #34175, #22695, #96078, .T. ) ;
#92721 = ORIENTED_EDGE ( 'NONE', *, *, #34992, .F. ) ;
#92722 = CARTESIAN_POINT ( 'NONE',  ( -26.07767875451820316, -24.95303847834740907, 4.027978703335532096 ) ) ;
#92723 = CARTESIAN_POINT ( 'NONE',  ( -92.58614606148624659, -24.51314013834316796, 0.6176544820404266112 ) ) ;
#92724 = EDGE_CURVE ( 'NONE', #41093, #68328, #73896, .T. ) ;
#92725 = LINE ( 'NONE', #75501, #10789 ) ;
#92726 = CARTESIAN_POINT ( 'NONE',  ( -70.49292501847948245, -24.73486907724917572, 1.287355809206963908 ) ) ;
#92728 = EDGE_LOOP ( 'NONE', ( #44558, #38174, #21607, #77898 ) ) ;
#92727 = CARTESIAN_POINT ( 'NONE',  ( 16.48747857468482891, 13.79107804547330929, 11.49999999999999645 ) ) ;
#92729 = CYLINDRICAL_SURFACE ( 'NONE', #28974, 1.306876713926001798 ) ;
#92730 = CARTESIAN_POINT ( 'NONE',  ( -34.62287095715007723, -23.94994826722565762, -0.6494450866342736939 ) ) ;
#92731 = EDGE_CURVE ( 'NONE', #45676, #99683, #3901, .T. ) ;
#92732 = ORIENTED_EDGE ( 'NONE', *, *, #24145, .F. ) ;
#92733 = EDGE_CURVE ( 'NONE', #54952, #58907, #89095, .T. ) ;
#92734 = CARTESIAN_POINT ( 'NONE',  ( 20.29938135082171158, -4.300543036493735372, -1.500000000000002220 ) ) ;
#92735 = ORIENTED_EDGE ( 'NONE', *, *, #12541, .T. ) ;
#92737 = EDGE_LOOP ( 'NONE', ( #58214, #22902, #35436, #98250 ) ) ;
#92736 = PLANE ( 'NONE',  #36163 ) ;
#92738 = VECTOR ( 'NONE', #6298, 1000.000000000000000 ) ;
#92739 = B_SPLINE_SURFACE_WITH_KNOTS ( 'NONE', 3, 3, ( 
 ( #90453, #20932, #82340, #51905 ),
 ( #37168, #43790, #36666, #67631 ),
 ( #36176, #83334, #98552, #45287 ),
 ( #98052, #29048, #44789, #60523 ),
 ( #60023, #76213, #52397, #61014 ),
 ( #91438, #99046, #21921, #14811 ),
 ( #59517, #52900, #6708, #37663 ) ),
 .UNSPECIFIED., .F., .F., .F.,
 ( 4, 3, 4 ),
 ( 4, 4 ),
 ( 0.0004766839783814116297, 0.1029713700210891786, 0.2054660560637969480 ),
 ( 0.9097254158518339739, 0.9111578860431817084 ),
 .UNSPECIFIED. ) ;
#92740 = CARTESIAN_POINT ( 'NONE',  ( 10.57556460110582286, 0.7139560615726621151, 8.999999999999984013 ) ) ;
#92741 = ORIENTED_EDGE ( 'NONE', *, *, #27731, .F. ) ;
#92742 = VERTEX_POINT ( 'NONE', #27229 ) ;
#92743 = CARTESIAN_POINT ( 'NONE',  ( -55.52287095715006870, -23.47596703998600631, 11.44779298504228926 ) ) ;
#92744 = CARTESIAN_POINT ( 'NONE',  ( -117.2228709571500644, -23.47596703998600631, 11.44779298504227860 ) ) ;
#92745 = EDGE_CURVE ( 'NONE', #44101, #55067, #74459, .T. ) ;
#92746 = CARTESIAN_POINT ( 'NONE',  ( -102.5228709571500474, -24.50321055353806088, 9.387540953477520489 ) ) ;
#92747 = CARTESIAN_POINT ( 'NONE',  ( -4.809782828112996178, 21.40371668077904488, 11.49999999999999645 ) ) ;
#92748 = CARTESIAN_POINT ( 'NONE',  ( 20.50669422456317292, -9.396423750077818937, -1.500000000000002220 ) ) ;
#92749 = CARTESIAN_POINT ( 'NONE',  ( -12.59924929152775874, 16.77720732749412846, 11.49999999999998934 ) ) ;
#92750 = FACE_OUTER_BOUND ( 'NONE', #62394, .T. ) ;
#92751 = FACE_OUTER_BOUND ( 'NONE', #13220, .T. ) ;
#92752 = VERTEX_POINT ( 'NONE', #4395 ) ;
#92753 = AXIS2_PLACEMENT_3D ( 'NONE', #34294, #33787, #26171 ) ;
#92754 = ORIENTED_EDGE ( 'NONE', *, *, #8212, .T. ) ;
#92755 = ORIENTED_EDGE ( 'NONE', *, *, #81277, .T. ) ;
#92756 = B_SPLINE_CURVE_WITH_KNOTS ( 'NONE', 3,
 ( #16091, #7982, #8982, #48057, #16585, #78986 ),
 .UNSPECIFIED., .F., .F.,
 ( 4, 2, 4 ),
 ( 0.000000000000000000, 0.001380901958385389412, 0.002761803916770778824 ),
 .UNSPECIFIED. ) ;
#92757 = CARTESIAN_POINT ( 'NONE',  ( -36.62287095715005592, -24.34917612406837861, 0.1852690917426571271 ) ) ;
#92758 = CARTESIAN_POINT ( 'NONE',  ( -10.19830463584622571, -18.94658877215714909, -1.500000000000002220 ) ) ;
#92759 = CARTESIAN_POINT ( 'NONE',  ( -85.52287095715004739, -29.50249982740957577, 7.747779886224967605 ) ) ;
#92760 = ORIENTED_EDGE ( 'NONE', *, *, #13019, .F. ) ;
#92761 = CARTESIAN_POINT ( 'NONE',  ( 6.572693220633653688, -20.11273663914708365, 11.49999999999998934 ) ) ;
#92762 = CARTESIAN_POINT ( 'NONE',  ( -96.62287095715005592, -29.50248528299804818, 1.056150453629042030 ) ) ;
#92763 = CARTESIAN_POINT ( 'NONE',  ( -50.46940435010577630, -25.26041116785443563, 7.561691964516831455 ) ) ;
#92764 = CARTESIAN_POINT ( 'NONE',  ( -121.5222464850925661, -23.48783264082477373, -1.443836473390087916 ) ) ;
#92765 = DIRECTION ( 'NONE',  ( -1.000000000000000000, -3.773278334444167608E-23, -8.201307833595939069E-29 ) ) ;
#92766 = CARTESIAN_POINT ( 'NONE',  ( -101.5228709571500758, -24.51283580621364777, 0.6167428607019801445 ) ) ;
#92767 = CARTESIAN_POINT ( 'NONE',  ( 5.777647480883832287, 21.37485705712154171, -1.500000000000002220 ) ) ;
#92768 = CARTESIAN_POINT ( 'NONE',  ( -81.52213703500444808, -23.48786465467241058, 11.44779295918254824 ) ) ;
#92769 = EDGE_CURVE ( 'NONE', #24715, #11225, #27067, .T. ) ;
#92770 = B_SPLINE_CURVE_WITH_KNOTS ( 'NONE', 3,
 ( #63418, #14822, #61529, #69117, #71017, #30048 ),
 .UNSPECIFIED., .F., .F.,
 ( 4, 2, 4 ),
 ( 1.570887131794638196E-05, 0.001396322306279762591, 0.002776935741241578874 ),
 .UNSPECIFIED. ) ;
#92771 = ORIENTED_EDGE ( 'NONE', *, *, #73374, .F. ) ;
#92772 = CARTESIAN_POINT ( 'NONE',  ( -82.55620429048336462, -23.47596703998600276, 11.44779298504227683 ) ) ;
#92773 = CARTESIAN_POINT ( 'NONE',  ( -110.6228709571500559, -29.50250786944525672, 11.44777988621622988 ) ) ;
#92774 = CARTESIAN_POINT ( 'NONE',  ( -2.960655606634402748, -19.13016773636607581, 11.49999999999999645 ) ) ;
#92775 = EDGE_CURVE ( 'NONE', #70435, #69536, #6578, .T. ) ;
#92776 = CARTESIAN_POINT ( 'NONE',  ( -100.5053578517286326, -24.92564183028979130, 1.928384488918251760 ) ) ;
#92777 = VECTOR ( 'NONE', #15285, 1000.000000000000000 ) ;
#92778 = CARTESIAN_POINT ( 'NONE',  ( 19.33761327413411024, 2.027444641817329973, -1.500000000000002220 ) ) ;
#92779 = SECURITY_CLASSIFICATION ( '', '', #13295 ) ;
#92780 = CARTESIAN_POINT ( 'NONE',  ( -11.99125074976391048, 17.70416384622758343, 11.49999999999998934 ) ) ;
#92781 = LINE ( 'NONE', #38506, #43430 ) ;
#92782 = LINE ( 'NONE', #46128, #44887 ) ;
#92783 = DIRECTION ( 'NONE',  ( 0.000000000000000000, 0.000000000000000000, 1.000000000000000000 ) ) ;
#92784 = CARTESIAN_POINT ( 'NONE',  ( -107.6228709571500701, -23.47593901973091235, -1.443836447538999312 ) ) ;
#92785 = CARTESIAN_POINT ( 'NONE',  ( -7.973561950239375307, 21.24132968703115765, -1.500000000000002220 ) ) ;
#92786 = AXIS2_PLACEMENT_3D ( 'NONE', #47653, #87200, #16183 ) ;
#92787 = ADVANCED_FACE ( 'NONE', ( #59682 ), #90614, .F. ) ;
#92788 = DIRECTION ( 'NONE',  ( -0.7689940216596069522, 5.365801633547210331E-16, 0.6392559695863496705 ) ) ;
#92789 = CARTESIAN_POINT ( 'NONE',  ( -122.5562042904833646, -23.48783264082479505, -1.443836473390057717 ) ) ;
#92790 = CARTESIAN_POINT ( 'NONE',  ( -18.24115112668064853, 7.888873183027880209, 11.49999999999999645 ) ) ;
#92791 = AXIS2_PLACEMENT_3D ( 'NONE', #33361, #26758, #48106 ) ;
#92792 = DIRECTION ( 'NONE',  ( -0.9994733861282923959, -0.000000000000000000, -0.03244919754393515293 ) ) ;
#92793 = ORIENTED_EDGE ( 'NONE', *, *, #29868, .F. ) ;
#92794 = CARTESIAN_POINT ( 'NONE',  ( 10.57556460110582996, 0.7139560615726621151, -8.999999999999994671 ) ) ;
#92795 = EDGE_CURVE ( 'NONE', #69074, #57808, #38813, .T. ) ;
#92796 = CARTESIAN_POINT ( 'NONE',  ( 8.160000000000000142, 0.1579206558577707364, 6.788828319098143105 ) ) ;
#92797 = DIRECTION ( 'NONE',  ( -1.000000000000000000, 0.000000000000000000, 0.000000000000000000 ) ) ;
#92798 = CARTESIAN_POINT ( 'NONE',  ( 1.064956243273112557, 21.61254047163424019, -1.500000000000002220 ) ) ;
#92799 = CARTESIAN_POINT ( 'NONE',  ( 6.044871794871792048, -5.876774720514402084, 18.16025641025640880 ) ) ;
#92800 = CARTESIAN_POINT ( 'NONE',  ( -13.55963120218723361, -13.89248740512243430, -1.500000000000002220 ) ) ;
#92801 = LINE ( 'NONE', #53763, #41608 ) ;
#92802 = CARTESIAN_POINT ( 'NONE',  ( -55.62594644532315868, -24.92592662359560762, 8.075495903017996469 ) ) ;
#92803 = CARTESIAN_POINT ( 'NONE',  ( 18.55763160240848109, 7.024834138330111166, -1.500000000000002220 ) ) ;
#92804 = ORIENTED_EDGE ( 'NONE', *, *, #99188, .T. ) ;
#92805 = CARTESIAN_POINT ( 'NONE',  ( 5.487062353440709472, 19.58251264919930534, 11.49999999999999645 ) ) ;
#92806 = CARTESIAN_POINT ( 'NONE',  ( -80.58144820728932700, -24.92564183028979130, 1.928384488918253536 ) ) ;
#92807 = APPROVAL ( #98530, 'UNSPECIFIED' ) ;
#92808 = CARTESIAN_POINT ( 'NONE',  ( -26.91814428177455909, -6.376774720514426953, 29.98490496616818746 ) ) ;
#92809 = B_SPLINE_CURVE_WITH_KNOTS ( 'NONE', 3,
 ( #48510, #54124, #78431, #87055 ),
 .UNSPECIFIED., .F., .F.,
 ( 4, 4 ),
 ( 0.000000000000000000, 1.000000000000000000 ),
 .UNSPECIFIED. ) ;
#92810 = ORIENTED_EDGE ( 'NONE', *, *, #16198, .T. ) ;
#92811 = CARTESIAN_POINT ( 'NONE',  ( -102.5870824237361489, -24.51419770103155926, 9.386484678747178734 ) ) ;
#92812 = DIRECTION ( 'NONE',  ( -1.000000000000000000, -0.000000000000000000, 0.000000000000000000 ) ) ;
#92813 = CARTESIAN_POINT ( 'NONE',  ( -48.87629837916329478, -25.25214667544315716, 6.044965762095690032 ) ) ;
#92814 = CARTESIAN_POINT ( 'NONE',  ( -40.54153813899623060, -24.40133493613049609, 9.663955038902802386 ) ) ;
#92815 = B_SPLINE_CURVE_WITH_KNOTS ( 'NONE', 3,
 ( #27518, #80615, #57308, #24823, #87736, #80115, #18221, #49191 ),
 .UNSPECIFIED., .F., .F.,
 ( 4, 2, 2, 4 ),
 ( -0.001224873891641418272, -0.0002244903592271035083, 0.0007758931731872112554, 0.002776660238015837313 ),
 .UNSPECIFIED. ) ;
#92816 = CARTESIAN_POINT ( 'NONE',  ( -81.92287095715008149, -23.47596703998600631, 11.44779298504227860 ) ) ;
#92817 = CARTESIAN_POINT ( 'NONE',  ( 20.09017895974002599, 0.4902201509063087159, -1.500000000000002220 ) ) ;
#92818 = CARTESIAN_POINT ( 'NONE',  ( 3.138110291115776995, 11.54688212118755075, 3.549999999999999822 ) ) ;
#92819 = AXIS2_PLACEMENT_3D ( 'NONE', #19611, #34851, #89139 ) ;
#92820 = EDGE_LOOP ( 'NONE', ( #2280, #83312, #18576, #17600, #88901 ) ) ;
#92821 = CARTESIAN_POINT ( 'NONE',  ( -30.64427850938831099, -23.56000036390796382, 11.50200000000000067 ) ) ;
#92822 = CARTESIAN_POINT ( 'NONE',  ( 11.15996004898972771, 19.99216496293481882, 11.49999999999999645 ) ) ;
#92823 = CARTESIAN_POINT ( 'NONE',  ( 17.68435195917723490, -14.24712819257710095, 11.49999999999998934 ) ) ;
#92824 = ORIENTED_EDGE ( 'NONE', *, *, #45043, .F. ) ;
#92825 = CARTESIAN_POINT ( 'NONE',  ( -45.52287095715006160, -23.85196035786899316, -0.8779234886475214550 ) ) ;
#92826 = AXIS2_PLACEMENT_3D ( 'NONE', #70601, #69091, #38641 ) ;
#92827 = CARTESIAN_POINT ( 'NONE',  ( 11.23292546672365155, 2.682774720514426559, -27.03842650381641377 ) ) ;
#92828 = CARTESIAN_POINT ( 'NONE',  ( -38.50503708857883822, -23.96169478059712432, 10.65365249895718591 ) ) ;
#92829 = CARTESIAN_POINT ( 'NONE',  ( -30.57287095715006586, -25.23631683304001072, 3.591709287666025485 ) ) ;
#92830 = LINE ( 'NONE', #22807, #70507 ) ;
#92831 = PLANE ( 'NONE',  #51740 ) ;
#92832 = ORIENTED_EDGE ( 'NONE', *, *, #98096, .T. ) ;
#92833 = CARTESIAN_POINT ( 'NONE',  ( 20.35419724272142616, 1.316291261081859787, 11.49999999999998934 ) ) ;
#92834 = ORIENTED_EDGE ( 'NONE', *, *, #6973, .F. ) ;
#92835 = EDGE_CURVE ( 'NONE', #82610, #27537, #84033, .T. ) ;
#92836 = CARTESIAN_POINT ( 'NONE',  ( 20.04565040668967413, 11.27863464804978477, -1.500000000000002220 ) ) ;
#92837 = CARTESIAN_POINT ( 'NONE',  ( -88.52287095715006160, -23.47593901973090524, -1.443836447538996426 ) ) ;
#92838 = ORIENTED_EDGE ( 'NONE', *, *, #28946, .T. ) ;
#92839 = CARTESIAN_POINT ( 'NONE',  ( -101.6228709571501270, -24.33927499327855060, 9.819080762295810061 ) ) ;
#92840 = CARTESIAN_POINT ( 'NONE',  ( -81.30502697372733678, -25.19369771803663127, 6.720958911583400308 ) ) ;
#92841 = VECTOR ( 'NONE', #14299, 1000.000000000000000 ) ;
#92842 = B_SPLINE_CURVE_WITH_KNOTS ( 'NONE', 3,
 ( #22547, #92077, #69750, #232, #31174, #65662 ),
 .UNSPECIFIED., .F., .F.,
 ( 4, 2, 4 ),
 ( 0.000000000000000000, 0.001380901958385388545, 0.002761803916770777089 ),
 .UNSPECIFIED. ) ;
#92843 = CARTESIAN_POINT ( 'NONE',  ( -51.52205495810211033, -23.48786465467241058, 11.44779295918254824 ) ) ;
#92845 = EDGE_LOOP ( 'NONE', ( #88520, #4369, #30602, #43167 ) ) ;
#92844 = CARTESIAN_POINT ( 'NONE',  ( 13.48273455363431772, -16.43370779934446801, 11.49999999999999645 ) ) ;
#92846 = VERTEX_POINT ( 'NONE', #94367 ) ;
#92847 = EDGE_CURVE ( 'NONE', #83417, #53379, #42896, .T. ) ;
#92848 = ORIENTED_EDGE ( 'NONE', *, *, #40427, .F. ) ;
#92849 = CARTESIAN_POINT ( 'NONE',  ( 0.7529269182969693386, -22.20201975079678647, 11.49999999999998934 ) ) ;
#92850 = ADVANCED_FACE ( 'NONE', ( #22081 ), #38033, .T. ) ;
#92851 = CARTESIAN_POINT ( 'NONE',  ( -11.86786554430972096, -16.85652113839894639, 11.49999999999998934 ) ) ;
#92852 = ORIENTED_EDGE ( 'NONE', *, *, #62995, .T. ) ;
#92854 = ORIENTED_EDGE ( 'NONE', *, *, #26653, .F. ) ;
#92853 = AXIS2_PLACEMENT_3D ( 'NONE', #34764, #35273, #88058 ) ;
#92855 = CARTESIAN_POINT ( 'NONE',  ( -5.023036858974361252, -6.376774720514410077, 19.14743589743590846 ) ) ;
#92856 = CARTESIAN_POINT ( 'NONE',  ( -95.50253988115005654, -24.92592662359561473, 8.075495903017998245 ) ) ;
#92857 = VERTEX_POINT ( 'NONE', #85486 ) ;
#92858 = CARTESIAN_POINT ( 'NONE',  ( -91.54409941458948197, -24.65952944569304606, 1.056160979905703234 ) ) ;
#92859 = ORIENTED_EDGE ( 'NONE', *, *, #794, .F. ) ;
#92860 = CONICAL_SURFACE ( 'NONE', #49153, 1.249999999999996003, 0.7853981633974514986 ) ;
#92861 = CARTESIAN_POINT ( 'NONE',  ( -6.499999999999992895, -1.267509437117509414E-15, 0.000000000000000000 ) ) ;
#92862 = CARTESIAN_POINT ( 'NONE',  ( -96.52287095715006160, -29.50248528299804818, 1.056150453629042030 ) ) ;
#92863 = CARTESIAN_POINT ( 'NONE',  ( -20.61801493038525379, 2.926015819835423581, -1.500000000000002220 ) ) ;
#92864 = EDGE_CURVE ( 'NONE', #32116, #28525, #79176, .T. ) ;
#92865 = CARTESIAN_POINT ( 'NONE',  ( 6.392671032147439369, 20.83241601264130693, 11.49999999999999645 ) ) ;
#92866 = CARTESIAN_POINT ( 'NONE',  ( 26.29690453849245912, -5.126799159439001663, -7.299189467990571778 ) ) ;
#92867 = FACE_OUTER_BOUND ( 'NONE', #2786, .T. ) ;
#92868 = CARTESIAN_POINT ( 'NONE',  ( -22.46026885398333661, -0.8929446408661095846, 11.49999999999998934 ) ) ;
#92869 = FACE_OUTER_BOUND ( 'NONE', #31851, .T. ) ;
#92870 = ORIENTED_EDGE ( 'NONE', *, *, #91676, .T. ) ;
#92871 = FACE_OUTER_BOUND ( 'NONE', #23226, .T. ) ;
#92872 = DIRECTION ( 'NONE',  ( -0.6599726524652352877, 0.000000000000000000, 0.7512896232465891000 ) ) ;
#92873 = B_SPLINE_SURFACE_WITH_KNOTS ( 'NONE', 3, 1, ( 
 ( #19933, #39410 ),
 ( #27567, #24177 ),
 ( #86080, #97065 ),
 ( #78958, #17066 ),
 ( #33290, #50902 ),
 ( #58519, #47533 ),
 ( #2868, #78455 ),
 ( #64277, #89456 ),
 ( #33800, #87591 ),
 ( #18071, #48543 ),
 ( #49041, #81842 ),
 ( #32296, #8958 ),
 ( #70871, #63267 ),
 ( #40416, #55652 ),
 ( #71372, #32796 ),
 ( #17571, #79469 ),
 ( #5214, #98547 ),
 ( #43294, #82336 ),
 ( #21416, #29043 ),
 ( #44783, #67136 ),
 ( #51900, #35674 ),
 ( #91433, #28542 ),
 ( #52393, #59511 ) ),
 .UNSPECIFIED., .F., .F., .F.,
 ( 4, 1, 1, 1, 1, 1, 1, 1, 1, 1, 1, 1, 1, 1, 1, 1, 1, 1, 1, 1, 4 ),
 ( 2, 2 ),
 ( 0.000000000000000000, 0.06003444026901250119, 0.1202779235945630187, 0.1823475613976146548, 0.2479191353524036190, 0.2816410472276386079, 0.3157005399103620658, 0.3503217567352117090, 0.3857031347924850806, 0.4218194746720334010, 0.4591956847073521697, 0.4978664178964332665, 0.5383012713842354469, 0.5812102302905466367, 0.6281834969011891312, 0.6794027672860705191, 0.7346986428153930992, 0.7940735398291317582, 0.8584163058134541835, 0.9270489341241319181, 1.000000000000000000 ),
 ( 0.000000000000000000, 1.000000000000000000 ),
 .UNSPECIFIED. ) ;
#92874 = VERTEX_POINT ( 'NONE', #83491 ) ;
#92875 = ORIENTED_EDGE ( 'NONE', *, *, #16821, .F. ) ;
#92876 = ORIENTED_EDGE ( 'NONE', *, *, #19334, .F. ) ;
#92877 = CARTESIAN_POINT ( 'NONE',  ( 16.11712757473013014, 13.99349609535929773, -1.500000000000002220 ) ) ;
#92878 = ORIENTED_EDGE ( 'NONE', *, *, #72802, .F. ) ;
#92879 = CARTESIAN_POINT ( 'NONE',  ( 16.43158684610488862, 13.14696595092960152, -1.500000000000002220 ) ) ;
#92880 = CARTESIAN_POINT ( 'NONE',  ( -30.56647679783655036, -24.05295578312052385, -0.4713115009884515927 ) ) ;
#92881 = CARTESIAN_POINT ( 'NONE',  ( -114.5228709571500616, -29.50248528299804818, 1.056150453629043584 ) ) ;
#92882 = CARTESIAN_POINT ( 'NONE',  ( 2.905029696106983916, -5.876774720514415407, 20.12486936895525957 ) ) ;
#92883 = CARTESIAN_POINT ( 'NONE',  ( -18.27885182143903720, 12.20952002138517045, -1.500000000000002220 ) ) ;
#92884 = CARTESIAN_POINT ( 'NONE',  ( -76.62287095715007013, -24.65952944569304606, 1.056160979905700126 ) ) ;
#92885 = EDGE_LOOP ( 'NONE', ( #29621, #68888, #93940, #25969 ) ) ;
#92886 = DIRECTION ( 'NONE',  ( -3.773278334453080206E-23, 0.9999999999976377785, 2.173523156925979975E-06 ) ) ;
#92887 = AXIS2_PLACEMENT_3D ( 'NONE', #63085, #94011, #18395 ) ;
#92888 = CARTESIAN_POINT ( 'NONE',  ( -125.6228709571500559, -29.50248789122583659, 2.256150453626215580 ) ) ;
#92889 = CARTESIAN_POINT ( 'NONE',  ( -20.74012505511919713, -1.853331690952414013, 11.49999999999999645 ) ) ;
#92890 = ADVANCED_FACE ( 'NONE', ( #30708 ), #61678, .F. ) ;
#92891 = DIRECTION ( 'NONE',  ( 0.000000000000000000, 0.000000000000000000, -1.000000000000000000 ) ) ;
#92892 = AXIS2_PLACEMENT_3D ( 'NONE', #82949, #46397, #22536 ) ;
#92893 = CARTESIAN_POINT ( 'NONE',  ( -6.499999999999992895, 0.9999999999999997780, 1.084202172485504187E-16 ) ) ;
#92894 = CARTESIAN_POINT ( 'NONE',  ( -10.26553491520735406, -22.69622746286980330, 9.960784317162939772 ) ) ;
#92895 = CARTESIAN_POINT ( 'NONE',  ( -9.338289970059909351, 19.12570833482435617, 11.49999999999998934 ) ) ;
#92896 = CARTESIAN_POINT ( 'NONE',  ( -98.59358047865015351, -23.96169478059713853, 10.65365249895717881 ) ) ;
#92897 = FACE_OUTER_BOUND ( 'NONE', #18242, .T. ) ;
#92898 = CARTESIAN_POINT ( 'NONE',  ( -90.62287095715002749, -23.84047902841601640, -0.8780736468305799791 ) ) ;
#92899 = CARTESIAN_POINT ( 'NONE',  ( -69.99198265981809186, -25.28687673834294003, 5.910757521653128066 ) ) ;
#92900 = CARTESIAN_POINT ( 'NONE',  ( -14.39138815452349718, -17.32352244779961481, -1.500000000000002220 ) ) ;
#92901 = EDGE_CURVE ( 'NONE', #7329, #11431, #28318, .T. ) ;
#92902 = CARTESIAN_POINT ( 'NONE',  ( -110.9414999475800272, -25.06174035403189038, 7.474877196992074424 ) ) ;
#92903 = ORIENTED_EDGE ( 'NONE', *, *, #85452, .T. ) ;
#92904 = FACE_OUTER_BOUND ( 'NONE', #47068, .T. ) ;
#92905 = CARTESIAN_POINT ( 'NONE',  ( 9.507684299284662188, -17.14340340408069707, 11.49999999999999645 ) ) ;
#92906 = CARTESIAN_POINT ( 'NONE',  ( -125.6228709571500559, -24.52232992886361274, 0.6492154411906163602 ) ) ;
#92907 = CARTESIAN_POINT ( 'NONE',  ( -32.52287095715006160, -24.51387760970726504, 9.387446482453436047 ) ) ;
#92908 = ORIENTED_EDGE ( 'NONE', *, *, #38443, .T. ) ;
#92909 = FACE_OUTER_BOUND ( 'NONE', #37732, .T. ) ;
#92910 = DIRECTION ( 'NONE',  ( -3.773278334453079618E-23, 0.9999999999976377785, 2.173523156925979975E-06 ) ) ;
#92911 = CARTESIAN_POINT ( 'NONE',  ( -88.86953192292943982, -25.31476272485208057, 5.144091107239471938 ) ) ;
#92912 = VECTOR ( 'NONE', #55473, 1000.000000000000114 ) ;
#92913 = CARTESIAN_POINT ( 'NONE',  ( 15.11087362536062173, -12.71848776332401521, -1.500000000000002220 ) ) ;
#92914 = VERTEX_POINT ( 'NONE', #60681 ) ;
#92915 = CARTESIAN_POINT ( 'NONE',  ( 5.548031177074126852, 6.376774720514426953, -25.42222224686167920 ) ) ;
#92916 = EDGE_CURVE ( 'NONE', #23124, #59212, #1730, .T. ) ;
#92917 = EDGE_CURVE ( 'NONE', #37981, #57842, #68282, .T. ) ;
#92918 = AXIS2_PLACEMENT_3D ( 'NONE', #27657, #50998, #2827 ) ;
#92919 = COORDINATED_UNIVERSAL_TIME_OFFSET ( 0, 0, .AHEAD. ) ;
#92920 = ORIENTED_EDGE ( 'NONE', *, *, #22365, .T. ) ;
#92921 = CARTESIAN_POINT ( 'NONE',  ( -29.49875734969025842, -5.965225279485572685, 17.86602280011862476 ) ) ;
#92922 = FACE_OUTER_BOUND ( 'NONE', #96617, .T. ) ;
#92923 = CARTESIAN_POINT ( 'NONE',  ( -81.75072539166535535, -25.23679622552714363, 6.293943003980942308 ) ) ;
#92924 = CARTESIAN_POINT ( 'NONE',  ( 1.255616527394258553, 17.95615290467683778, -9.000000000000000000 ) ) ;
#92925 = CARTESIAN_POINT ( 'NONE',  ( 6.274899854645557440, -6.376774720514429617, 21.83451738260096775 ) ) ;
#92926 = DIRECTION ( 'NONE',  ( 0.000000000000000000, 0.000000000000000000, 1.000000000000000000 ) ) ;
#92927 = CIRCLE ( 'NONE', #49219, 2.249999999999998668 ) ;
#92928 = CARTESIAN_POINT ( 'NONE',  ( -29.62287095715004881, -23.39678932012542845, -1.443836140311830940 ) ) ;
#92929 = CARTESIAN_POINT ( 'NONE',  ( 18.25133680241413359, 8.160682379734268466, 11.49999999999998934 ) ) ;
#92930 = DIRECTION ( 'NONE',  ( -0.000000000000000000, 2.173523156925979552E-06, -0.9999999999976378895 ) ) ;
#92931 = CARTESIAN_POINT ( 'NONE',  ( -51.66817263684756512, -25.29162628464893103, 4.237763228474503485 ) ) ;
#92932 = ORIENTED_EDGE ( 'NONE', *, *, #80981, .F. ) ;
#92933 = EDGE_CURVE ( 'NONE', #21, #46348, #51331, .T. ) ;
#92934 = EDGE_CURVE ( 'NONE', #78991, #23706, #80384, .T. ) ;
#92935 = CARTESIAN_POINT ( 'NONE',  ( -79.50173439926879837, -24.51419770103157347, 9.386484678747176957 ) ) ;
#92936 = CARTESIAN_POINT ( 'NONE',  ( -109.6228709571500559, -29.50250786944525672, 11.44777988621622988 ) ) ;
#92937 = CARTESIAN_POINT ( 'NONE',  ( -35.61370564495084778, -23.85016227208580730, -0.8807180028928173199 ) ) ;
#92938 = CARTESIAN_POINT ( 'NONE',  ( -101.9507253916653440, -25.25287247409162816, 6.236250661346385726 ) ) ;
#92939 = CARTESIAN_POINT ( 'NONE',  ( -7.160000000000000142, 1.682056942681651401, 5.192823660268256702 ) ) ;
#92940 = CARTESIAN_POINT ( 'NONE',  ( -19.69812919673063689, -0.3587747205143964613, -22.00173861453436430 ) ) ;
#92941 = B_SPLINE_SURFACE_WITH_KNOTS ( 'NONE', 3, 1, ( 
 ( #67726, #5804 ),
 ( #29139, #36761 ),
 ( #39123, #74324 ),
 ( #76299, #12910 ),
 ( #60114, #83418 ),
 ( #13905, #93403 ),
 ( #98140, #43876 ),
 ( #28154, #52993 ),
 ( #51490, #44381 ),
 ( #74809, #4815 ),
 ( #35769, #14405 ),
 ( #82426, #31513 ),
 ( #5305, #44884 ),
 ( #90049, #75804 ),
 ( #62476, #54867 ),
 ( #59607, #43386 ),
 ( #29640, #13408 ),
 ( #36264, #66738 ),
 ( #6306, #37262 ),
 ( #91535, #49270 ),
 ( #86304, #47250 ),
 ( #9684, #80197 ),
 ( #25908, #93911 ) ),
 .UNSPECIFIED., .F., .F., .F.,
 ( 4, 1, 1, 1, 1, 1, 1, 1, 1, 1, 1, 1, 1, 1, 1, 1, 1, 1, 1, 1, 4 ),
 ( 2, 2 ),
 ( 0.000000000000000000, 0.05968866615394263775, 0.1195065383498360445, 0.1810745839532865720, 0.2461623370263499311, 0.2798942139317999178, 0.3144679584461503863, 0.3504028635546707626, 0.3874736882805470684, 0.4261472450317768113, 0.4666236557295641019, 0.5087454666265019965, 0.5533282563676282795, 0.6000583194662235664, 0.6491770639906175866, 0.7005515754705256004, 0.7548938693300147884, 0.8118248696719926327, 0.8715135358259358256, 0.9343188020093610158, 1.000000000000000000 ),
 ( 0.000000000000000000, 1.000000000000000000 ),
 .UNSPECIFIED. ) ;
#92942 = LINE ( 'NONE', #23418, #944 ) ;
#92943 = DIRECTION ( 'NONE',  ( 0.000000000000000000, 2.173523156925980399E-06, -0.9999999999976378895 ) ) ;
#92944 = ORIENTED_EDGE ( 'NONE', *, *, #45900, .T. ) ;
#92945 = CARTESIAN_POINT ( 'NONE',  ( 20.23811035156253979, -1.552196809741442696, 11.49999999999998934 ) ) ;
#92946 = EDGE_CURVE ( 'NONE', #50658, #84887, #51140, .T. ) ;
#92947 = CARTESIAN_POINT ( 'NONE',  ( 29.58897068672300179, 4.307329379639823763, 29.06043472499518643 ) ) ;
#92948 = VECTOR ( 'NONE', #32111, 1000.000000000000114 ) ;
#92949 = CARTESIAN_POINT ( 'NONE',  ( -7.749999999999996447, 23.99999999999999289, 2.100000000000000089 ) ) ;
#92950 = ORIENTED_EDGE ( 'NONE', *, *, #94861, .F. ) ;
#92951 = CARTESIAN_POINT ( 'NONE',  ( -86.52287095715009002, -24.35013146730204170, 9.818937971375103047 ) ) ;
#92952 = CARTESIAN_POINT ( 'NONE',  ( -19.48533387766964964, -5.011242947278518045, -1.500000000000002220 ) ) ;
#92953 = VECTOR ( 'NONE', #77977, 1000.000000000000114 ) ;
#92954 = CARTESIAN_POINT ( 'NONE',  ( -14.90395405082875335, 14.90835605916499418, 11.49999999999999645 ) ) ;
#92955 = CARTESIAN_POINT ( 'NONE',  ( 2.710298230372018669, -21.94706154713207980, -1.500000000000002220 ) ) ;
#92956 = EDGE_CURVE ( 'NONE', #41964, #26321, #48551, .T. ) ;
#92957 = CARTESIAN_POINT ( 'NONE',  ( -20.41219973434085944, 2.133827299322149429, 11.49999999999998934 ) ) ;
#92958 = CARTESIAN_POINT ( 'NONE',  ( -59.66800995418955722, -25.32911129577617970, 4.489957709566354538 ) ) ;
#92959 = CARTESIAN_POINT ( 'NONE',  ( -60.56964333814166679, -23.48783264082477018, -1.443836473390097908 ) ) ;
#92960 = VERTEX_POINT ( 'NONE', #2774 ) ;
#92961 = CARTESIAN_POINT ( 'NONE',  ( 26.73860345374794534, 1.682774720514426114, 3.440769881205035638E-15 ) ) ;
#92962 = ORIENTED_EDGE ( 'NONE', *, *, #52422, .T. ) ;
#92963 = ADVANCED_FACE ( 'NONE', ( #55056 ), #41325, .T. ) ;
#92964 = DIRECTION ( 'NONE',  ( -0.8788171126619707119, 0.4771587602595986910, -0.000000000000000000 ) ) ;
#92965 = CARTESIAN_POINT ( 'NONE',  ( -85.62287095715002749, -24.52323809116983000, 9.355190652339416602 ) ) ;
#92966 = ORIENTED_EDGE ( 'NONE', *, *, #80816, .T. ) ;
#92967 = EDGE_LOOP ( 'NONE', ( #73151, #32282, #10205, #46980, #31950, #57862, #97369, #36352 ) ) ;
#92968 = ORIENTED_EDGE ( 'NONE', *, *, #2020, .F. ) ;
#92969 = CARTESIAN_POINT ( 'NONE',  ( -116.6228709571500559, -23.47593901973091235, -1.443836447538997536 ) ) ;
#92970 = PLANE ( 'NONE',  #11362 ) ;
#92971 = CARTESIAN_POINT ( 'NONE',  ( -68.58386858832108146, -24.51419770103157347, 9.386484678747180510 ) ) ;
#92972 = CARTESIAN_POINT ( 'NONE',  ( 20.28538307770854487, 3.844468116359331944, -1.500000000000002220 ) ) ;
#92973 = EDGE_CURVE ( 'NONE', #1282, #47230, #78862, .T. ) ;
#92974 = CARTESIAN_POINT ( 'NONE',  ( 17.58597629297885589, -12.55149374826878272, 11.49999999999999645 ) ) ;
#92975 = ORIENTED_EDGE ( 'NONE', *, *, #25845, .F. ) ;
#92976 = CARTESIAN_POINT ( 'NONE',  ( -11.64875734969026233, 0.3587747205144265483, 31.02402280011862246 ) ) ;
#92977 = CARTESIAN_POINT ( 'NONE',  ( -60.62287095715006302, -24.91544648472620693, 1.928969306349228363 ) ) ;
#92978 = CARTESIAN_POINT ( 'NONE',  ( -15.72835732567950195, 15.92727474065614501, -1.500000000000002220 ) ) ;
#92979 = EDGE_CURVE ( 'NONE', #52696, #24841, #78366, .T. ) ;
#92980 = CARTESIAN_POINT ( 'NONE',  ( -47.64622550042292204, -23.96169478059712432, 10.65365249895718591 ) ) ;
#92981 = LINE ( 'NONE', #8260, #12487 ) ;
#92982 = ORIENTED_EDGE ( 'NONE', *, *, #62794, .F. ) ;
#92983 = CARTESIAN_POINT ( 'NONE',  ( -58.55620429048338593, -24.65952944569304250, 1.056160979905696129 ) ) ;
#92984 = CARTESIAN_POINT ( 'NONE',  ( 6.365284455128204399, -5.876774720514413630, 19.73076923076922640 ) ) ;
#92985 = PLANE ( 'NONE',  #84302 ) ;
#92986 = CARTESIAN_POINT ( 'NONE',  ( -16.12721948686093754, -13.32240427740599564, 11.49999999999998934 ) ) ;
#92987 = VERTEX_POINT ( 'NONE', #25595 ) ;
#92988 = DIRECTION ( 'NONE',  ( 0.000000000000000000, -1.000000000000000000, 0.000000000000000000 ) ) ;
#92989 = ORIENTED_EDGE ( 'NONE', *, *, #99782, .F. ) ;
#92990 = CARTESIAN_POINT ( 'NONE',  ( -128.6228709571500701, -23.95044443724992433, 10.65354141964650481 ) ) ;
#92991 = CARTESIAN_POINT ( 'NONE',  ( 19.97935793590388442, -6.945280299276400449, -1.500000000000002220 ) ) ;
#92992 = B_SPLINE_CURVE_WITH_KNOTS ( 'NONE', 3,
 ( #59768, #52641, #36414, #67377 ),
 .UNSPECIFIED., .F., .F.,
 ( 4, 4 ),
 ( 0.000000000000000000, 9.999999999998206125E-05 ),
 .UNSPECIFIED. ) ;
#92993 = ORIENTED_EDGE ( 'NONE', *, *, #92480, .F. ) ;
#92994 = CARTESIAN_POINT ( 'NONE',  ( -50.67080217151737287, -23.48783264082476308, -1.443836473390096797 ) ) ;
#92995 = CARTESIAN_POINT ( 'NONE',  ( 17.22188757068894915, 13.35947340969901198, -1.500000000000002220 ) ) ;
#92996 = PLANE ( 'NONE',  #99957 ) ;
#92997 = B_SPLINE_CURVE_WITH_KNOTS ( 'NONE', 3,
 ( #100054, #67659, #51927, #6731 ),
 .UNSPECIFIED., .F., .F.,
 ( 4, 4 ),
 ( 0.6292232213963703247, 0.6302239684371359063 ),
 .UNSPECIFIED. ) ;
#92998 = CARTESIAN_POINT ( 'NONE',  ( -41.52287095715006870, -24.64898659630528144, 1.056161002820819261 ) ) ;
#92999 = CARTESIAN_POINT ( 'NONE',  ( 7.370931459274800090, -6.376774720514417183, 20.26286690110499578 ) ) ;
#93000 = CARTESIAN_POINT ( 'NONE',  ( 17.22188757068894915, 13.35947340969901198, -1.500000000000002220 ) ) ;
#93001 = CARTESIAN_POINT ( 'NONE',  ( -95.52287095715011844, -24.52232992886363760, 0.6492154411906031486 ) ) ;
#93002 = ORIENTED_EDGE ( 'NONE', *, *, #27568, .F. ) ;
#93003 = CARTESIAN_POINT ( 'NONE',  ( -30.54625915432725591, -23.48007831457673689, 11.44779284091286087 ) ) ;
#93004 = CARTESIAN_POINT ( 'NONE',  ( 14.76093561896379214, 3.316774720514426456, -26.55548769130089681 ) ) ;
#93005 = ORIENTED_EDGE ( 'NONE', *, *, #50792, .F. ) ;
#93006 = ORIENTED_EDGE ( 'NONE', *, *, #5024, .T. ) ;
#93007 = EDGE_CURVE ( 'NONE', #90387, #44200, #64186, .T. ) ;
#93008 = VERTEX_POINT ( 'NONE', #32198 ) ;
#93009 = CARTESIAN_POINT ( 'NONE',  ( -29.24566889703875106, -25.20109657442075601, 4.649030501266317117 ) ) ;
#93010 = CARTESIAN_POINT ( 'NONE',  ( 282.9764569301858046, 2.682774720514426559, 20.79159422840526616 ) ) ;
#93011 = CARTESIAN_POINT ( 'NONE',  ( -4.771770383141621608, -20.67029057396967318, -1.500000000000002220 ) ) ;
#93012 = CARTESIAN_POINT ( 'NONE',  ( -121.6228709571500417, -23.47593901973091235, -1.443836447538997536 ) ) ;
#93013 = CARTESIAN_POINT ( 'NONE',  ( -79.98156793206884174, -25.27791956405971163, 7.487048666137972042 ) ) ;
#93014 = VECTOR ( 'NONE', #18811, 1000.000000000000000 ) ;
#93015 = FACE_OUTER_BOUND ( 'NONE', #86153, .T. ) ;
#93016 = CARTESIAN_POINT ( 'NONE',  ( -99.52287095715003318, -23.72747288104470087, -1.053458166803225682 ) ) ;
#93017 = CARTESIAN_POINT ( 'NONE',  ( 18.67713048845720181, -5.233370074711279685, 11.49999999999998934 ) ) ;
#93018 = EDGE_CURVE ( 'NONE', #404, #81766, #14548, .T. ) ;
#93019 = CARTESIAN_POINT ( 'NONE',  ( -40.93246554024547379, -25.31392318313163514, 5.203682277190879724 ) ) ;
#93020 = VERTEX_POINT ( 'NONE', #40324 ) ;
#93021 = CARTESIAN_POINT ( 'NONE',  ( 3.148799746435844593, 19.17640706095922098, 11.49999999999999645 ) ) ;
#93022 = DIRECTION ( 'NONE',  ( -0.9888510809027408754, -5.365801633547210331E-16, -0.1489078231574191558 ) ) ;
#93023 = DIRECTION ( 'NONE',  ( -0.000000000000000000, 1.000000000000000000, -0.000000000000000000 ) ) ;
#93024 = VERTEX_POINT ( 'NONE', #93592 ) ;
#93025 = VECTOR ( 'NONE', #4990, 1000.000000000000114 ) ;
#93026 = CARTESIAN_POINT ( 'NONE',  ( 3.714584954927674154, -5.876774720514403860, 18.16171433633635246 ) ) ;
#93027 = LINE ( 'NONE', #16915, #20473 ) ;
#93028 = CARTESIAN_POINT ( 'NONE',  ( -0.4909855769230799249, -6.376774720514410077, 19.14743589743590491 ) ) ;
#93029 = DIRECTION ( 'NONE',  ( -1.000000000000000000, -0.000000000000000000, 0.000000000000000000 ) ) ;
#93030 = CARTESIAN_POINT ( 'NONE',  ( 0.7808950796103379943, -19.64173473864696717, 11.49999999999998934 ) ) ;
#93031 = CIRCLE ( 'NONE', #91375, 6.119803529381341534 ) ;
#93032 = CARTESIAN_POINT ( 'NONE',  ( -41.46379453422112249, -25.31583596542261816, 4.278542312007326487 ) ) ;
#93033 = VERTEX_POINT ( 'NONE', #24584 ) ;
#93034 = CARTESIAN_POINT ( 'NONE',  ( 5.819084965910729323, 20.79142713412266730, 11.49999999999998934 ) ) ;
#93035 = CARTESIAN_POINT ( 'NONE',  ( 22.02124265030973760, 3.456774720514426136, 17.35402280011862786 ) ) ;
#93036 = CARTESIAN_POINT ( 'NONE',  ( -40.58888693302551331, -24.52300882791530157, 0.6510814631126359275 ) ) ;
#93037 = CARTESIAN_POINT ( 'NONE',  ( -90.52287095715000476, -24.52323809116983355, 9.355190652339423707 ) ) ;
#93038 = CARTESIAN_POINT ( 'NONE',  ( -16.13607370526515794, 16.44073208242836159, -1.500000000000002220 ) ) ;
#93039 = EDGE_CURVE ( 'NONE', #78762, #4757, #27534, .T. ) ;
#93040 = APPLICATION_PROTOCOL_DEFINITION ( 'international standard', 'config_control_design', 1994, #42716 ) ;
#93041 = CARTESIAN_POINT ( 'NONE',  ( -93.62566969909174475, -24.51314013834316086, 0.6176544820404149538 ) ) ;
#93042 = CARTESIAN_POINT ( 'NONE',  ( -115.5562042904833788, -23.47593901973091235, -1.443836447538997536 ) ) ;
#93043 = CARTESIAN_POINT ( 'NONE',  ( -121.5564787414976990, -23.73791477778912551, 11.05961554403170055 ) ) ;
#93044 = DIRECTION ( 'NONE',  ( 0.000000000000000000, 0.9999999999976377785, 2.173523156925979128E-06 ) ) ;
#93045 = CARTESIAN_POINT ( 'NONE',  ( -109.5647320221236356, -25.22850916238827068, 3.633130482123976712 ) ) ;
#93046 = CARTESIAN_POINT ( 'NONE',  ( -121.6228709571500417, -23.48786465467241769, 11.44779295918253759 ) ) ;
#93047 = CARTESIAN_POINT ( 'NONE',  ( -99.64934318012689118, -25.31566098596702119, 4.927356294101793210 ) ) ;
#93048 = CARTESIAN_POINT ( 'NONE',  ( 14.69432462292611952, 13.40460087117274490, 11.49999999999998934 ) ) ;
#93050 = EDGE_CURVE ( 'NONE', #63968, #42129, #47556, .T. ) ;
#93049 = CARTESIAN_POINT ( 'NONE',  ( -79.11611000704996854, -25.21083105912962097, 3.409327675794633361 ) ) ;
#93051 = CARTESIAN_POINT ( 'NONE',  ( -5.703961651189128901, -19.02375728206049743, -1.500000000000002220 ) ) ;
#93052 = EDGE_CURVE ( 'NONE', #36444, #97749, #9363, .T. ) ;
#93053 = CARTESIAN_POINT ( 'NONE',  ( 0.3545156366401029935, -5.876774720514414518, 20.17598923696321478 ) ) ;
#93054 = ADVANCED_FACE ( 'NONE', ( #94604 ), #49451, .F. ) ;
#93055 = EDGE_CURVE ( 'NONE', #65803, #27638, #2275, .T. ) ;
#93056 = CARTESIAN_POINT ( 'NONE',  ( -39.04979701406145409, -25.29116779651338831, 4.033763859792823148 ) ) ;
#93057 = CARTESIAN_POINT ( 'NONE',  ( 5.802984775641024662, -5.876774720514403860, 18.35026041666666430 ) ) ;
#93058 = CARTESIAN_POINT ( 'NONE',  ( 5.906898857431191807, -19.90033995357616092, 11.49999999999999645 ) ) ;
#93059 = CARTESIAN_POINT ( 'NONE',  ( 10.24059822343752479, -5.876774720514426953, -2.394817856121274864E-14 ) ) ;
#93060 = CARTESIAN_POINT ( 'NONE',  ( -126.5562042904833930, -24.64898659630529565, 1.056161002820832806 ) ) ;
#93061 = CARTESIAN_POINT ( 'NONE',  ( -16.34568771794417685, -15.85656593008108750, 11.49999999999999645 ) ) ;
#93062 = ORIENTED_EDGE ( 'NONE', *, *, #62334, .F. ) ;
#93063 = CARTESIAN_POINT ( 'NONE',  ( -69.56520740950848847, -23.48783264082476308, -1.443836473390097908 ) ) ;
#93064 = CARTESIAN_POINT ( 'NONE',  ( -16.22218391600152643, 6.475225279485573360, -54.85883559227303863 ) ) ;
#93065 = ORIENTED_EDGE ( 'NONE', *, *, #4850, .F. ) ;
#93066 = CARTESIAN_POINT ( 'NONE',  ( -19.98115086844608612, 2.773124471107000666, -1.500000000000002220 ) ) ;
#93067 = EDGE_CURVE ( 'NONE', #52082, #85110, #48815, .T. ) ;
#93068 = ADVANCED_FACE ( 'NONE', ( #32702 ), #95107, .T. ) ;
#93069 = CARTESIAN_POINT ( 'NONE',  ( 30.43908124610613086, 2.682774720514426559, -13.86910542224436682 ) ) ;
#93070 = CARTESIAN_POINT ( 'NONE',  ( -95.62287095715005592, -24.99132157543084531, 2.256160258750667502 ) ) ;
#93071 = B_SPLINE_CURVE_WITH_KNOTS ( 'NONE', 3,
 ( #35451, #11105, #96344, #66420 ),
 .UNSPECIFIED., .F., .F.,
 ( 4, 4 ),
 ( 0.1699072510866937724, 0.1789136823588095560 ),
 .UNSPECIFIED. ) ;
#93072 = ORIENTED_EDGE ( 'NONE', *, *, #24145, .T. ) ;
#93073 = ORIENTED_EDGE ( 'NONE', *, *, #19135, .F. ) ;
#93074 = ADVANCED_FACE ( 'NONE', ( #35213 ), #13350, .T. ) ;
#93075 = LINE ( 'NONE', #30179, #9633 ) ;
#93076 = CARTESIAN_POINT ( 'NONE',  ( -13.69284064830502423, 18.33895024417757469, 11.49999999999998934 ) ) ;
#93077 = CARTESIAN_POINT ( 'NONE',  ( -41.51659605236564232, -25.19377129250086611, 3.283922396756908668 ) ) ;
#93078 = CARTESIAN_POINT ( 'NONE',  ( 20.17453868081960167, 7.849935799312063089, -1.500000000000002220 ) ) ;
#93079 = CARTESIAN_POINT ( 'NONE',  ( -123.5194377984048941, -24.51314013834318217, 0.6176544820404261671 ) ) ;
#93080 = CARTESIAN_POINT ( 'NONE',  ( -15.12424899162716230, 14.39509690008720177, 11.49999999999999645 ) ) ;
#93081 = ORIENTED_EDGE ( 'NONE', *, *, #20547, .T. ) ;
#93082 = CARTESIAN_POINT ( 'NONE',  ( -69.03429854110324015, -25.31612597287615785, 5.665244572013464541 ) ) ;
#93083 = CARTESIAN_POINT ( 'NONE',  ( -21.82725030464235516, 2.967780500094957308, -1.500000000000002220 ) ) ;
#93084 = AXIS2_PLACEMENT_3D ( 'NONE', #67125, #82326, #66635 ) ;
#93085 = EDGE_CURVE ( 'NONE', #23597, #57023, #45421, .T. ) ;
#93086 = DIRECTION ( 'NONE',  ( 0.000000000000000000, 0.000000000000000000, 1.000000000000000000 ) ) ;
#93087 = LINE ( 'NONE', #747, #26969 ) ;
#93088 = ORIENTED_EDGE ( 'NONE', *, *, #45668, .F. ) ;
#93089 = CARTESIAN_POINT ( 'NONE',  ( 3.797776442307698286, -6.376774720514401196, 18.16025641025640525 ) ) ;
#93090 = FACE_OUTER_BOUND ( 'NONE', #75895, .T. ) ;
#93091 = VERTEX_POINT ( 'NONE', #34710 ) ;
#93092 = CARTESIAN_POINT ( 'NONE',  ( -72.65005370508750104, -23.48786465467241058, 11.44779295918254824 ) ) ;
#93093 = VERTEX_POINT ( 'NONE', #28587 ) ;
#93094 = ORIENTED_EDGE ( 'NONE', *, *, #84953, .F. ) ;
#93095 = CARTESIAN_POINT ( 'NONE',  ( -71.65051242377489871, -23.48786465467241058, 11.44779295918254824 ) ) ;
#93096 = CARTESIAN_POINT ( 'NONE',  ( -101.4571681947234083, -25.27404731337933441, 3.296845483386515063 ) ) ;
#93097 = CARTESIAN_POINT ( 'NONE',  ( -36.64213287987285383, -24.15543982623907127, -0.2315651400026672579 ) ) ;
#93098 = CARTESIAN_POINT ( 'NONE',  ( 19.09590870110849181, 7.302211495713927469, -1.500000000000002220 ) ) ;
#93099 = EDGE_CURVE ( 'NONE', #35481, #58114, #73277, .T. ) ;
#93100 = AXIS2_PLACEMENT_3D ( 'NONE', #32337, #77990, #385 ) ;
#93101 = EDGE_LOOP ( 'NONE', ( #12991, #57478, #53837, #8295 ) ) ;
#93102 = LINE ( 'NONE', #85491, #55904 ) ;
#93103 = CARTESIAN_POINT ( 'NONE',  ( -44.50617629668793995, -23.96119346886879953, -0.6495511937832129101 ) ) ;
#93104 = CARTESIAN_POINT ( 'NONE',  ( -99.55620429048337883, -23.48783264082477729, -1.443836473390061492 ) ) ;
#93105 = CARTESIAN_POINT ( 'NONE',  ( 4.546662993595487201, 21.82331882591909178, -1.500000000000002220 ) ) ;
#93106 = ADVANCED_FACE ( 'NONE', ( #82373 ), #75256, .T. ) ;
#93107 = CARTESIAN_POINT ( 'NONE',  ( 14.43441819135929727, -5.965225279485572685, -28.36222020317710246 ) ) ;
#93108 = CARTESIAN_POINT ( 'NONE',  ( -31.52287095715006160, -24.66019654487198665, 8.947790411086131712 ) ) ;
#93109 = ORIENTED_EDGE ( 'NONE', *, *, #12078, .T. ) ;
#93110 = EDGE_CURVE ( 'NONE', #46485, #85772, #4264, .T. ) ;
#93111 = DIRECTION ( 'NONE',  ( 1.000000000000000000, -0.000000000000000000, 1.286817348990133655E-16 ) ) ;
#93112 = CARTESIAN_POINT ( 'NONE',  ( -29.81116385467300489, -25.26247379366626333, 5.042945557627021458 ) ) ;
#93113 = CARTESIAN_POINT ( 'NONE',  ( 9.770152518076534065, 18.40777400073588410, 11.49999999999998934 ) ) ;
#93114 = EDGE_LOOP ( 'NONE', ( #53975, #64405, #41420, #8598 ) ) ;
#93116 = ORIENTED_EDGE ( 'NONE', *, *, #85849, .F. ) ;
#93115 = CARTESIAN_POINT ( 'NONE',  ( 3.903461913076534451, -6.376774720514404748, 18.52532880998198905 ) ) ;
#93117 = DIRECTION ( 'NONE',  ( 4.218136541796977197E-15, -1.000000000000000000, 1.324960360541890271E-16 ) ) ;
#93118 = CARTESIAN_POINT ( 'NONE',  ( -17.04133944854041616, 12.32129857345222845, -1.500000000000002220 ) ) ;
#93119 = ORIENTED_EDGE ( 'NONE', *, *, #89994, .T. ) ;
#93120 = CARTESIAN_POINT ( 'NONE',  ( -69.52287095715009002, -24.51387760970724727, 9.387446482453405849 ) ) ;
#93121 = CARTESIAN_POINT ( 'NONE',  ( -51.29687923781917647, -25.26364009307625125, 3.993462176398971497 ) ) ;
#93122 = FACE_OUTER_BOUND ( 'NONE', #68059, .T. ) ;
#93123 = CARTESIAN_POINT ( 'NONE',  ( -123.6228709571500559, -23.48783264082478794, -1.443836473390058606 ) ) ;
#93124 = CARTESIAN_POINT ( 'NONE',  ( -92.55184653144422668, -24.15620529776627734, 10.23563542870659937 ) ) ;
#93125 = LINE ( 'NONE', #1298, #65973 ) ;
#93127 = EDGE_LOOP ( 'NONE', ( #79916, #4879, #91130, #82378 ) ) ;
#93126 = CARTESIAN_POINT ( 'NONE',  ( -0.9571703918902072505, -22.19477237104690914, 11.49999999999999645 ) ) ;
#93128 = DIRECTION ( 'NONE',  ( 0.000000000000000000, -0.9999999999976377785, -2.173523156925979128E-06 ) ) ;
#93129 = CARTESIAN_POINT ( 'NONE',  ( -44.62287095715004881, -23.48786465467240347, 11.44779295918255180 ) ) ;
#93130 = ORIENTED_EDGE ( 'NONE', *, *, #18217, .F. ) ;
#93131 = CARTESIAN_POINT ( 'NONE',  ( -21.16596634977960179, 8.012090315382277339, -1.500000000000002220 ) ) ;
#93133 = EDGE_LOOP ( 'NONE', ( #14604, #20486, #2996, #97118 ) ) ;
#93132 = CARTESIAN_POINT ( 'NONE',  ( 32.98733314340959311, -5.965225279485572685, 2.074222136288530027 ) ) ;
#93134 = ORIENTED_EDGE ( 'NONE', *, *, #2880, .F. ) ;
#93135 = AXIS2_PLACEMENT_3D ( 'NONE', #4469, #42538, #28286 ) ;
#93136 = CARTESIAN_POINT ( 'NONE',  ( -8.499999999999987566, 18.74999999999999645, 0.000000000000000000 ) ) ;
#93137 = CARTESIAN_POINT ( 'NONE',  ( 14.24339680280927567, 14.23919408161895284, 11.49999999999998934 ) ) ;
#93138 = CARTESIAN_POINT ( 'NONE',  ( -81.62287095715002749, -23.73934037231756378, 11.05740245334329153 ) ) ;
#93139 = ORIENTED_EDGE ( 'NONE', *, *, #45420, .F. ) ;
#93140 = FACE_OUTER_BOUND ( 'NONE', #42853, .T. ) ;
#93141 = CARTESIAN_POINT ( 'NONE',  ( -1.374798071107336206, -22.32369649477951512, -1.500000000000002220 ) ) ;
#93142 = ORIENTED_EDGE ( 'NONE', *, *, #32601, .T. ) ;
#93143 = VERTEX_POINT ( 'NONE', #51436 ) ;
#93144 = DIRECTION ( 'NONE',  ( 1.000000000000000000, 0.000000000000000000, 1.286817348990133408E-16 ) ) ;
#93145 = LINE ( 'NONE', #71334, #3794 ) ;
#93146 = DIRECTION ( 'NONE',  ( 0.000000000000000000, 1.000000000000000000, 4.688851412615178005E-17 ) ) ;
#93147 = CARTESIAN_POINT ( 'NONE',  ( -100.5228709571500616, -25.00182538069145366, 7.747789668545101982 ) ) ;
#93148 = FACE_BOUND ( 'NONE', #37013, .T. ) ;
#93149 = B_SPLINE_CURVE_WITH_KNOTS ( 'NONE', 3,
 ( #22776, #21780, #84190, #36522, #83695, #67489, #28915, #92306 ),
 .UNSPECIFIED., .F., .F.,
 ( 4, 2, 2, 4 ),
 ( -0.001224873891641431716, -0.0002244903592271139166, 0.0007758931731872038828, 0.002776660238015839482 ),
 .UNSPECIFIED. ) ;
#93150 = CARTESIAN_POINT ( 'NONE',  ( 14.87128047407919951, 12.67365258641725312, -1.500000000000002220 ) ) ;
#93151 = CARTESIAN_POINT ( 'NONE',  ( -33.58953762381673869, -24.64898659630367206, 1.056161002820377393 ) ) ;
#93152 = CARTESIAN_POINT ( 'NONE',  ( 19.88731969966643476, 8.162773808193900749, 11.49999999999998934 ) ) ;
#93153 = CARTESIAN_POINT ( 'NONE',  ( -102.5895376238167245, -23.48786465467241769, 11.44779295918253936 ) ) ;
#93154 = DIRECTION ( 'NONE',  ( 0.000000000000000000, 0.000000000000000000, -1.000000000000000000 ) ) ;
#93155 = PLANE ( 'NONE',  #24700 ) ;
#93156 = CARTESIAN_POINT ( 'NONE',  ( -111.6228709571500559, -24.51283580621365132, 0.6167428607019819209 ) ) ;
#93158 = AXIS2_PLACEMENT_3D ( 'NONE', #19936, #6209, #28065 ) ;
#93157 = CARTESIAN_POINT ( 'NONE',  ( -4.526818761702180893, -22.41603498850323817, -1.500000000000002220 ) ) ;
#93159 = COORDINATED_UNIVERSAL_TIME_OFFSET ( 0, 0, .AHEAD. ) ;
#93160 = CARTESIAN_POINT ( 'NONE',  ( -96.52217807345559208, -23.48786465467241413, 11.44779295918254469 ) ) ;
#93161 = CARTESIAN_POINT ( 'NONE',  ( -71.18709340149318621, -25.29354215769174985, 5.743106921551899724 ) ) ;
#93162 = CARTESIAN_POINT ( 'NONE',  ( -7.547287378330592489, -18.53391252851691462, 11.49999999999999645 ) ) ;
#93163 = CARTESIAN_POINT ( 'NONE',  ( -79.55620429048339304, -23.48783264082478794, -1.443836473390066821 ) ) ;
#93164 = LINE ( 'NONE', #69849, #24156 ) ;
#93165 = EDGE_CURVE ( 'NONE', #30912, #47809, #87434, .T. ) ;
#93166 = ADVANCED_FACE ( 'NONE', ( #66185 ), #5250, .F. ) ;
#93167 = FACE_OUTER_BOUND ( 'NONE', #44822, .T. ) ;
#93168 = CARTESIAN_POINT ( 'NONE',  ( 6.660000000000001030, -9.074990544709798712, -0.7360493640965781736 ) ) ;
#93169 = ORIENTED_EDGE ( 'NONE', *, *, #1321, .F. ) ;
#93170 = DIRECTION ( 'NONE',  ( 0.000000000000000000, -0.9999999999976377785, -2.173523156925979975E-06 ) ) ;
#93171 = LINE ( 'NONE', #84566, #97702 ) ;
#93172 = VECTOR ( 'NONE', #31205, 1000.000000000000000 ) ;
#93173 = EDGE_CURVE ( 'NONE', #60837, #9193, #85098, .T. ) ;
#93174 = CARTESIAN_POINT ( 'NONE',  ( -12.31242093702619123, -17.95196869449987531, 11.49999999999998934 ) ) ;
#93175 = CARTESIAN_POINT ( 'NONE',  ( -45.52287095715006870, -24.92604778743017491, 8.074972756849357225 ) ) ;
#93176 = CARTESIAN_POINT ( 'NONE',  ( 6.681059570357060551, -18.48443787736713873, -1.500000000000002220 ) ) ;
#93177 = EDGE_CURVE ( 'NONE', #36980, #36016, #74138, .T. ) ;
#93178 = VECTOR ( 'NONE', #57061, 1000.000000000000000 ) ;
#93179 = DIRECTION ( 'NONE',  ( -1.000000000000000000, -3.773278334444166432E-23, -8.201307841325785021E-29 ) ) ;
#93180 = EDGE_CURVE ( 'NONE', #83886, #93325, #65684, .T. ) ;
#93181 = FACE_OUTER_BOUND ( 'NONE', #7612, .T. ) ;
#93182 = APPROVAL_STATUS ( 'not_yet_approved' ) ;
#93183 = CARTESIAN_POINT ( 'NONE',  ( -91.51836248188099887, -23.73791477778912196, 11.05961554403170410 ) ) ;
#93184 = LINE ( 'NONE', #85575, #75082 ) ;
#93185 = CARTESIAN_POINT ( 'NONE',  ( 6.154377932377651739, 19.64630176443789367, 11.49999999999999645 ) ) ;
#93186 = CARTESIAN_POINT ( 'NONE',  ( -29.49875734969025842, -5.965225279485572685, 17.86602280011862476 ) ) ;
#93187 = CARTESIAN_POINT ( 'NONE',  ( -4.621320343559624177, 12.75000000000004974, 2.100000000000000089 ) ) ;
#93188 = ORIENTED_EDGE ( 'NONE', *, *, #60694, .F. ) ;
#93189 = CARTESIAN_POINT ( 'NONE',  ( -80.72727483400176141, -25.26273766163786405, 3.802328419063494280 ) ) ;
#93190 = CARTESIAN_POINT ( 'NONE',  ( -26.49029821382958616, -24.85479087585913049, 6.874653004683789703 ) ) ;
#93191 = B_SPLINE_CURVE_WITH_KNOTS ( 'NONE', 3,
 ( #61867, #23274, #70471, #8572, #85186, #25286 ),
 .UNSPECIFIED., .F., .F.,
 ( 4, 2, 4 ),
 ( 0.000000000000000000, 0.001380764517853249034, 0.002761529035706498068 ),
 .UNSPECIFIED. ) ;
#93192 = CARTESIAN_POINT ( 'NONE',  ( -125.5198022206274686, -24.73531770709095312, 8.716586749053508498 ) ) ;
#93193 = DIRECTION ( 'NONE',  ( -3.773278334453079030E-23, 0.9999999999976377785, 2.173523156925979128E-06 ) ) ;
#93194 = B_SPLINE_CURVE_WITH_KNOTS ( 'NONE', 3,
 ( #73319, #3814, #81919, #65725 ),
 .UNSPECIFIED., .F., .F.,
 ( 4, 4 ),
 ( 0.2506790037405462468, 0.2596854350126617805 ),
 .UNSPECIFIED. ) ;
#93195 = ADVANCED_FACE ( 'NONE', ( #58552 ), #26601, .T. ) ;
#93196 = FACE_OUTER_BOUND ( 'NONE', #2669, .T. ) ;
#93197 = VERTEX_POINT ( 'NONE', #3771 ) ;
#93198 = EDGE_CURVE ( 'NONE', #57335, #42504, #34260, .T. ) ;
#93199 = CARTESIAN_POINT ( 'NONE',  ( 8.428894486204411507, 21.44871590506140890, 11.49999999999999645 ) ) ;
#93200 = CARTESIAN_POINT ( 'NONE',  ( 19.59772090806136902, -11.66877021596143926, -1.500000000000002220 ) ) ;
#93201 = CARTESIAN_POINT ( 'NONE',  ( 4.572862496014544753, -5.876774720514408301, 19.20224321281611068 ) ) ;
#93202 = CARTESIAN_POINT ( 'NONE',  ( -67.52287095715011844, -23.96127896941631974, -0.6493128931038022467 ) ) ;
#93203 = CARTESIAN_POINT ( 'NONE',  ( -85.55620429048336462, -24.99156044556201905, 7.747789690856173195 ) ) ;
#93204 = AXIS2_PLACEMENT_3D ( 'NONE', #94944, #96946, #50282 ) ;
#93205 = CARTESIAN_POINT ( 'NONE',  ( 15.48037617655995923, 16.25473645317415361, 11.49999999999999645 ) ) ;
#93206 = EDGE_LOOP ( 'NONE', ( #55052, #57800 ) ) ;
#93207 = LINE ( 'NONE', #31313, #81681 ) ;
#93208 = LINE ( 'NONE', #39930, #54646 ) ;
#93209 = CARTESIAN_POINT ( 'NONE',  ( -19.17877449816284496, 10.63638241594707345, 11.49999999999998934 ) ) ;
#93210 = CARTESIAN_POINT ( 'NONE',  ( -113.5228709571500474, -23.73907113216990084, -1.053371485793245466 ) ) ;
#93211 = CARTESIAN_POINT ( 'NONE',  ( -34.48973961494164087, -24.35071581493542681, 9.817618358456032368 ) ) ;
#93212 = CARTESIAN_POINT ( 'NONE',  ( -74.52287095715007581, -23.48786465467241058, 11.44779295918254647 ) ) ;
#93213 = VERTEX_POINT ( 'NONE', #19972 ) ;
#93214 = CARTESIAN_POINT ( 'NONE',  ( -78.58187477321953907, -24.65952944569304606, 1.056160979905704789 ) ) ;
#93215 = CARTESIAN_POINT ( 'NONE',  ( 14.76093561896379214, 5.965225279485572685, -26.55548769130089681 ) ) ;
#93216 = ORIENTED_EDGE ( 'NONE', *, *, #75071, .T. ) ;
#93217 = CARTESIAN_POINT ( 'NONE',  ( 10.21088607376515789, 17.76353854702842483, 11.49999999999998934 ) ) ;
#93218 = ORIENTED_EDGE ( 'NONE', *, *, #97578, .F. ) ;
#93219 = ORIENTED_EDGE ( 'NONE', *, *, #95764, .F. ) ;
#93220 = ORIENTED_EDGE ( 'NONE', *, *, #44517, .F. ) ;
#93221 = ORIENTED_EDGE ( 'NONE', *, *, #5033, .T. ) ;
#93222 = CARTESIAN_POINT ( 'NONE',  ( -10.32085834726444595, 20.65377284989807194, -1.500000000000002220 ) ) ;
#93223 = CARTESIAN_POINT ( 'NONE',  ( -29.24636659180999843, -25.20264517434234364, 4.940287045316306802 ) ) ;
#93224 = CARTESIAN_POINT ( 'NONE',  ( -8.335131950130996614, 18.48905954037022781, -1.500000000000002220 ) ) ;
#93225 = ORIENTED_EDGE ( 'NONE', *, *, #93099, .T. ) ;
#93226 = LINE ( 'NONE', #23716, #26641 ) ;
#93227 = CARTESIAN_POINT ( 'NONE',  ( -41.86995616089614458, -25.28979658489737048, 4.210709715701590028 ) ) ;
#93228 = EDGE_CURVE ( 'NONE', #43106, #4626, #42345, .T. ) ;
#93229 = CARTESIAN_POINT ( 'NONE',  ( -93.92287095715006728, -23.47596703998600631, 11.44779298504227860 ) ) ;
#93230 = CARTESIAN_POINT ( 'NONE',  ( 4.486687842132109694, -5.876774720514410966, 18.98221446873611029 ) ) ;
#93232 = VERTEX_POINT ( 'NONE', #12356 ) ;
#93231 = CARTESIAN_POINT ( 'NONE',  ( 17.49997855696484095, 12.48231381050728928, 11.49999999999999645 ) ) ;
#93233 = CARTESIAN_POINT ( 'NONE',  ( -75.53595366234340247, -24.92564183028979130, 1.928384488918256645 ) ) ;
#93234 = CARTESIAN_POINT ( 'NONE',  ( -61.54323830618671565, -24.35071581493542681, 9.817618358456030592 ) ) ;
#93235 = ORIENTED_EDGE ( 'NONE', *, *, #98789, .F. ) ;
#93236 = B_SPLINE_CURVE_WITH_KNOTS ( 'NONE', 3,
 ( #92485, #23458, #7247, #22956, #47330, #54441, #78253, #70160, #643, #32091, #8766, #55446, #39702, #37707, #70664, #31592, #1155, #86386 ),
 .UNSPECIFIED., .F., .F.,
 ( 4, 2, 2, 2, 2, 2, 2, 2, 4 ),
 ( 0.004711262329854501267, 0.005300117079684243601, 0.005888971829513986803, 0.006477826579343729137, 0.007066681329173471471, 0.007655536079003214672, 0.008244390828832957874, 0.008833245578662701075, 0.009422100328492442542 ),
 .UNSPECIFIED. ) ;
#93237 = CARTESIAN_POINT ( 'NONE',  ( 12.91705851660734972, -16.24616318834520001, -1.500000000000002220 ) ) ;
#93238 = EDGE_CURVE ( 'NONE', #74917, #93802, #43957, .T. ) ;
#93239 = VECTOR ( 'NONE', #25201, 1000.000000000000114 ) ;
#93240 = VERTEX_POINT ( 'NONE', #66686 ) ;
#93242 = ORIENTED_EDGE ( 'NONE', *, *, #16638, .T. ) ;
#93241 = DIRECTION ( 'NONE',  ( 0.000000000000000000, 0.000000000000000000, -1.000000000000000000 ) ) ;
#93243 = CIRCLE ( 'NONE', #47909, 0.3000000000000016542 ) ;
#93244 = CARTESIAN_POINT ( 'NONE',  ( -75.62287095715004170, -24.62285846362214770, 9.038163152653526211 ) ) ;
#93245 = DIRECTION ( 'NONE',  ( 7.726610339123061470E-14, 0.000000000000000000, -1.000000000000000000 ) ) ;
#93246 = EDGE_LOOP ( 'NONE', ( #57057, #40052, #38892, #74544 ) ) ;
#93247 = ORIENTED_EDGE ( 'NONE', *, *, #99352, .T. ) ;
#93248 = CARTESIAN_POINT ( 'NONE',  ( 4.782775879418006859, -6.376774720514406525, 18.83817099474236656 ) ) ;
#93249 = DIRECTION ( 'NONE',  ( 0.000000000000000000, -0.9999999999976377785, -2.173523156925979128E-06 ) ) ;
#93250 = VECTOR ( 'NONE', #34018, 1000.000000000000000 ) ;
#93251 = CARTESIAN_POINT ( 'NONE',  ( -76.52287095715006160, -24.35013146730202749, 9.818937971375101270 ) ) ;
#93252 = CARTESIAN_POINT ( 'NONE',  ( -14.94409825380703616, 16.19114737329946507, 11.49999999999999645 ) ) ;
#93253 = VECTOR ( 'NONE', #57223, 1000.000000000000000 ) ;
#93254 = DIRECTION ( 'NONE',  ( -3.773278334453080206E-23, 0.9999999999976377785, 2.173523156925979975E-06 ) ) ;
#93255 = CARTESIAN_POINT ( 'NONE',  ( 11.64696156460271581, 19.30390316350253244, 11.49999999999998934 ) ) ;
#93256 = CARTESIAN_POINT ( 'NONE',  ( 20.78037738254806399, 3.014218216234254566, -1.500000000000002220 ) ) ;
#93257 = CARTESIAN_POINT ( 'NONE',  ( -105.5562042904834072, -23.47593901973091235, -1.443836447538999312 ) ) ;
#93258 = EDGE_LOOP ( 'NONE', ( #98119, #98481, #97962, #26489 ) ) ;
#93259 = VERTEX_POINT ( 'NONE', #22942 ) ;
#93260 = DIRECTION ( 'NONE',  ( -0.5473052603529005022, 0.000000000000000000, 0.8369330630283666750 ) ) ;
#93261 = DIRECTION ( 'NONE',  ( 0.000000000000000000, 1.000000000000000000, -0.000000000000000000 ) ) ;
#93262 = ORIENTED_EDGE ( 'NONE', *, *, #92369, .T. ) ;
#93263 = CARTESIAN_POINT ( 'NONE',  ( 19.97935793590388442, -6.945280299276400449, -1.500000000000002220 ) ) ;
#93264 = DIRECTION ( 'NONE',  ( -1.000000000000000000, -3.773278334444167608E-23, -8.201307833595939069E-29 ) ) ;
#93265 = CARTESIAN_POINT ( 'NONE',  ( -51.63614490863932360, -25.26040999518159680, 7.022165695762002890 ) ) ;
#93266 = CARTESIAN_POINT ( 'NONE',  ( -121.5532452859548584, -24.65952944569305316, 1.056160979905709008 ) ) ;
#93267 = LINE ( 'NONE', #54732, #8713 ) ;
#93268 = DIRECTION ( 'NONE',  ( -0.000000000000000000, -1.000000000000000000, -0.000000000000000000 ) ) ;
#93269 = CARTESIAN_POINT ( 'NONE',  ( -20.56242917251232782, -8.299981740788712870, -1.500000000000002220 ) ) ;
#93270 = CARTESIAN_POINT ( 'NONE',  ( -71.50676032721460729, -24.15543982623907127, -0.2315651400026636497 ) ) ;
#93271 = ORIENTED_EDGE ( 'NONE', *, *, #51731, .F. ) ;
#93272 = CARTESIAN_POINT ( 'NONE',  ( -51.04357394935764347, -25.31633084621363494, 4.940877927261252189 ) ) ;
#93273 = CARTESIAN_POINT ( 'NONE',  ( -64.62287095715004170, -23.72773821059535848, 11.05748984161097503 ) ) ;
#93274 = CARTESIAN_POINT ( 'NONE',  ( -126.6252818438354240, -23.48783264082477018, -1.443836473390087027 ) ) ;
#93275 = CARTESIAN_POINT ( 'NONE',  ( -76.22287095715006444, -23.47593901973090169, -1.443836447538997536 ) ) ;
#93276 = CARTESIAN_POINT ( 'NONE',  ( 10.46399479596396453, -2.682774720514426559, -27.03001098546561920 ) ) ;
#93277 = CARTESIAN_POINT ( 'NONE',  ( 16.42231304340664266, 10.40281881132301045, 11.49999999999998934 ) ) ;
#93278 = AXIS2_PLACEMENT_3D ( 'NONE', #90956, #83839, #36671 ) ;
#93279 = CARTESIAN_POINT ( 'NONE',  ( -16.30254408640404051, -13.89340296626662230, 11.49999999999998934 ) ) ;
#93280 = DIRECTION ( 'NONE',  ( -0.000000000000000000, -0.000000000000000000, -1.000000000000000000 ) ) ;
#93281 = CARTESIAN_POINT ( 'NONE',  ( -60.53841807966112043, -24.63419186845290199, 9.035850630957110496 ) ) ;
#93282 = CARTESIAN_POINT ( 'NONE',  ( -30.64427850938832165, -23.47593901973090524, -1.443836447538998424 ) ) ;
#93283 = CARTESIAN_POINT ( 'NONE',  ( -100.9649361822203133, -25.18440042256897726, 3.436944287541245480 ) ) ;
#93284 = CARTESIAN_POINT ( 'NONE',  ( -13.58842472641693711, -18.21064416987719525, -1.500000000000002220 ) ) ;
#93285 = CARTESIAN_POINT ( 'NONE',  ( -103.6228709571500985, -23.73907113216991860, -1.053371485793222817 ) ) ;
#93286 = PLANE ( 'NONE',  #8704 ) ;
#93287 = CARTESIAN_POINT ( 'NONE',  ( -3.387584560642538101, 19.54024307811383210, 11.49999999999999645 ) ) ;
#93288 = CARTESIAN_POINT ( 'NONE',  ( -123.6248514950247852, -24.15620529776629866, 10.23563542870659582 ) ) ;
#93289 = EDGE_CURVE ( 'NONE', #72299, #71152, #6395, .T. ) ;
#93290 = PLANE ( 'NONE',  #50617 ) ;
#93291 = VERTEX_POINT ( 'NONE', #7742 ) ;
#93292 = PLANE ( 'NONE',  #38027 ) ;
#93293 = DIRECTION ( 'NONE',  ( -3.773278334453079030E-23, 0.9999999999976377785, 2.173523156925979128E-06 ) ) ;
#93294 = ADVANCED_FACE ( 'NONE', ( #38184 ), #61047, .F. ) ;
#93295 = DIRECTION ( 'NONE',  ( -3.773278334444167608E-23, 1.000000000000000000, 0.000000000000000000 ) ) ;
#93296 = CARTESIAN_POINT ( 'NONE',  ( -3.891998276399621481, 21.28400606017829233, 11.49999999999998934 ) ) ;
#93297 = CARTESIAN_POINT ( 'NONE',  ( -56.62786050513864211, -24.51419770103157347, 9.386484678747180510 ) ) ;
#93298 = CARTESIAN_POINT ( 'NONE',  ( 10.09180897563621926, 16.61094848277074476, -1.500000000000002220 ) ) ;
#93299 = ADVANCED_FACE ( 'NONE', ( #84864 ), #69142, .T. ) ;
#93300 = CARTESIAN_POINT ( 'NONE',  ( -55.54394653881162469, -24.40133493613049964, 9.663955038902800609 ) ) ;
#93301 = ORIENTED_EDGE ( 'NONE', *, *, #32926, .F. ) ;
#93302 = EDGE_CURVE ( 'NONE', #99675, #75250, #21454, .T. ) ;
#93303 = CARTESIAN_POINT ( 'NONE',  ( 15.88337727998148985, 12.78846505907953279, 11.49999999999999645 ) ) ;
#93304 = CARTESIAN_POINT ( 'NONE',  ( -80.59640896514189023, -24.15503026093913164, -0.2815557561904567518 ) ) ;
#93305 = EDGE_CURVE ( 'NONE', #54440, #42578, #75744, .T. ) ;
#93306 = VECTOR ( 'NONE', #91829, 1000.000000000000000 ) ;
#93307 = LINE ( 'NONE', #31421, #90214 ) ;
#93308 = ORIENTED_EDGE ( 'NONE', *, *, #31345, .F. ) ;
#93309 = CARTESIAN_POINT ( 'NONE',  ( -15.87499999999997868, 0.000000000000000000, 0.000000000000000000 ) ) ;
#93310 = CARTESIAN_POINT ( 'NONE',  ( -62.52287095715006160, -24.64898659630367561, 1.056161002820822592 ) ) ;
#93311 = CARTESIAN_POINT ( 'NONE',  ( -48.92504535501358021, -25.31601999834449401, 5.781339443314535309 ) ) ;
#93312 = VECTOR ( 'NONE', #35625, 1000.000000000000000 ) ;
#93313 = CARTESIAN_POINT ( 'NONE',  ( -34.62287095715005592, -24.66019654487199020, 8.947790411086137041 ) ) ;
#93314 = AXIS2_PLACEMENT_3D ( 'NONE', #25780, #63873, #71972 ) ;
#93315 = CARTESIAN_POINT ( 'NONE',  ( -0.8502773128684013582, -6.376774720514413630, 19.61227901093089798 ) ) ;
#93316 = CARTESIAN_POINT ( 'NONE',  ( 8.649182803842551337, -18.14983140373652404, 11.49999999999998934 ) ) ;
#93317 = VECTOR ( 'NONE', #18215, 1000.000000000000000 ) ;
#93318 = DIRECTION ( 'NONE',  ( 0.000000000000000000, -1.000000000000000000, -6.307606751056558338E-17 ) ) ;
#93319 = ORIENTED_EDGE ( 'NONE', *, *, #49906, .T. ) ;
#93320 = CARTESIAN_POINT ( 'NONE',  ( -81.92287095715006728, -23.47593901973090169, -1.443836447538997092 ) ) ;
#93322 = ADVANCED_FACE ( 'NONE', ( #67667 ), #92469, .T. ) ;
#93321 = AXIS2_PLACEMENT_3D ( 'NONE', #55666, #9469, #48554 ) ;
#93323 = CARTESIAN_POINT ( 'NONE',  ( -11.09240565882118368, -20.00103931635436538, 11.49999999999999645 ) ) ;
#93324 = CARTESIAN_POINT ( 'NONE',  ( 17.68435195917723490, -14.24712819257710095, -1.500000000000002220 ) ) ;
#93325 = VERTEX_POINT ( 'NONE', #6244 ) ;
#93326 = CARTESIAN_POINT ( 'NONE',  ( -80.96226385320385077, -25.14083923594767001, 2.947789366383926968 ) ) ;
#93327 = CARTESIAN_POINT ( 'NONE',  ( 9.940598223437573822, -6.376774720514426953, 18.21871304725684837 ) ) ;
#93328 = CARTESIAN_POINT ( 'NONE',  ( -38.62372291133213054, -24.66019654487198665, 8.947790411086121054 ) ) ;
#93329 = CARTESIAN_POINT ( 'NONE',  ( -30.57287095715006231, -24.76779993212570474, 1.387997001552113696 ) ) ;
#93330 = CARTESIAN_POINT ( 'NONE',  ( -84.58953762381673869, -23.48786465467241769, 11.44779295918254469 ) ) ;
#93331 = DIRECTION ( 'NONE',  ( 0.000000000000000000, 0.000000000000000000, 1.000000000000000000 ) ) ;
#93332 = ORIENTED_EDGE ( 'NONE', *, *, #19602, .T. ) ;
#93333 = CARTESIAN_POINT ( 'NONE',  ( 8.549789220347504326, 18.50885834720105905, 11.49999999999998934 ) ) ;
#93334 = ORIENTED_EDGE ( 'NONE', *, *, #48197, .F. ) ;
#93335 = CARTESIAN_POINT ( 'NONE',  ( -21.48638390452810043, -8.140844714011898020, 11.49999999999998934 ) ) ;
#93336 = CARTESIAN_POINT ( 'NONE',  ( -54.58737563073252375, -24.35071581493543391, 9.817618358456034144 ) ) ;
#93337 = EDGE_LOOP ( 'NONE', ( #4663, #42360, #58298, #51043 ) ) ;
#93338 = FACE_OUTER_BOUND ( 'NONE', #48706, .T. ) ;
#93339 = CYLINDRICAL_SURFACE ( 'NONE', #90681, 1.500000000000000666 ) ;
#93340 = B_SPLINE_CURVE_WITH_KNOTS ( 'NONE', 3,
 ( #40249, #71200, #8291, #56494, #93016, #23492 ),
 .UNSPECIFIED., .F., .F.,
 ( 4, 2, 4 ),
 ( 0.000000000000000000, 0.001380764517854765616, 0.002761529035709531232 ),
 .UNSPECIFIED. ) ;
#93341 = DIRECTION ( 'NONE',  ( -0.000000000000000000, 1.000000000000000000, -0.000000000000000000 ) ) ;
#93343 = ORIENTED_EDGE ( 'NONE', *, *, #7420, .F. ) ;
#93342 = CARTESIAN_POINT ( 'NONE',  ( 6.245503531335690361, -20.37428601906679759, 11.49999999999999645 ) ) ;
#93344 = B_SPLINE_CURVE_WITH_KNOTS ( 'NONE', 3,
 ( #59250, #45031, #29788, #58747 ),
 .UNSPECIFIED., .F., .F.,
 ( 4, 4 ),
 ( 0.000000000000000000, 9.999999999998897304E-05 ),
 .UNSPECIFIED. ) ;
#93345 = ORIENTED_EDGE ( 'NONE', *, *, #27260, .F. ) ;
#93346 = CARTESIAN_POINT ( 'NONE',  ( 19.10802705166043580, 11.29804532628753044, -1.500000000000002220 ) ) ;
#93347 = CARTESIAN_POINT ( 'NONE',  ( 20.28538307770854487, 3.844468116359331944, -1.500000000000002220 ) ) ;
#93348 = EDGE_CURVE ( 'NONE', #89111, #95482, #60056, .T. ) ;
#93349 = ORIENTED_EDGE ( 'NONE', *, *, #32391, .F. ) ;
#93350 = ORIENTED_EDGE ( 'NONE', *, *, #70611, .F. ) ;
#93351 = CARTESIAN_POINT ( 'NONE',  ( -108.9567485977555634, -25.27682589219649145, 4.232820627358080401 ) ) ;
#93352 = ADVANCED_FACE ( 'NONE', ( #98588 ), #68655, .T. ) ;
#93353 = CARTESIAN_POINT ( 'NONE',  ( -95.55787687970359912, -23.85049219812686161, 10.88485053497527133 ) ) ;
#93354 = ORIENTED_EDGE ( 'NONE', *, *, #38030, .F. ) ;
#93355 = CARTESIAN_POINT ( 'NONE',  ( -3.106028565906091998, -6.376774720514426953, 3.106028565906120864 ) ) ;
#93356 = ORIENTED_EDGE ( 'NONE', *, *, #33461, .T. ) ;
#93357 = CARTESIAN_POINT ( 'NONE',  ( -58.60466919147697240, -23.73791477778911840, 11.05961554403170766 ) ) ;
#93358 = CARTESIAN_POINT ( 'NONE',  ( 21.97688922017995239, 1.682774720514426114, -18.55878510778117985 ) ) ;
#93359 = CARTESIAN_POINT ( 'NONE',  ( -19.40898059523135544, 7.551958013340856368, -1.500000000000002220 ) ) ;
#93361 = EDGE_CURVE ( 'NONE', #17858, #77501, #52432, .T. ) ;
#93360 = CARTESIAN_POINT ( 'NONE',  ( -1.743439162979827595, 21.76861016152796324, 11.49999999999999645 ) ) ;
#93362 = CARTESIAN_POINT ( 'NONE',  ( -27.68651082257923335, -24.89280003935763474, 7.605672334162794535 ) ) ;
#93363 = CARTESIAN_POINT ( 'NONE',  ( -78.62985670288350093, -24.35071581493543391, 9.817618358456027039 ) ) ;
#93364 = CARTESIAN_POINT ( 'NONE',  ( 16.82713599508461400, -14.87465808564757808, -1.500000000000002220 ) ) ;
#93365 = CIRCLE ( 'NONE', #52893, 28.96799999999999642 ) ;
#93366 = DIRECTION ( 'NONE',  ( -5.238131417152343399E-15, 0.000000000000000000, 1.000000000000000000 ) ) ;
#93367 = LINE ( 'NONE', #86764, #97144 ) ;
#93368 = DIRECTION ( 'NONE',  ( 0.000000000000000000, 0.000000000000000000, -1.000000000000000000 ) ) ;
#93369 = VERTEX_POINT ( 'NONE', #76733 ) ;
#93370 = EDGE_LOOP ( 'NONE', ( #82412, #87368, #36969, #41694, #54758, #14942, #77682, #17988, #52427, #10017 ) ) ;
#93371 = APPROVAL ( #68599, 'UNSPECIFIED' ) ;
#93372 = ORIENTED_EDGE ( 'NONE', *, *, #79217, .T. ) ;
#93373 = VECTOR ( 'NONE', #46251, 1000.000000000000227 ) ;
#93374 = CARTESIAN_POINT ( 'NONE',  ( 3.515848477382193416, 21.04717058667041130, -1.500000000000002220 ) ) ;
#93375 = ORIENTED_EDGE ( 'NONE', *, *, #33658, .F. ) ;
#93376 = VECTOR ( 'NONE', #27733, 1000.000000000000000 ) ;
#93377 = CARTESIAN_POINT ( 'NONE',  ( -19.68365937621761219, -7.520201837432793468, -1.500000000000002220 ) ) ;
#93378 = CARTESIAN_POINT ( 'NONE',  ( -30.58829557286704315, -23.48329323021739512, -1.443836490256471983 ) ) ;
#93379 = CARTESIAN_POINT ( 'NONE',  ( -4.495603250223349612, -19.44740727768710187, -1.500000000000002220 ) ) ;
#93380 = CARTESIAN_POINT ( 'NONE',  ( -50.57926052499865222, -24.83644354573578283, 8.397322867130100121 ) ) ;
#93381 = AXIS2_PLACEMENT_3D ( 'NONE', #19481, #50444, #81391 ) ;
#93382 = CARTESIAN_POINT ( 'NONE',  ( 9.278253834636473130, -5.876774720514426953, 21.78128695274316229 ) ) ;
#93383 = CARTESIAN_POINT ( 'NONE',  ( -0.4018715335629812202, -22.01094342083549193, -1.500000000000002220 ) ) ;
#93384 = DIRECTION ( 'NONE',  ( -1.000000000000000000, 0.000000000000000000, 0.000000000000000000 ) ) ;
#93385 = ORIENTED_EDGE ( 'NONE', *, *, #98271, .F. ) ;
#93386 = B_SPLINE_CURVE_WITH_KNOTS ( 'NONE', 3,
 ( #73398, #19091, #3893, #42953, #34832, #73889 ),
 .UNSPECIFIED., .F., .F.,
 ( 4, 2, 4 ),
 ( 0.000000000000000000, 0.001380901958385385075, 0.002761803916770770150 ),
 .UNSPECIFIED. ) ;
#93387 = CARTESIAN_POINT ( 'NONE',  ( -90.62287095715004170, -25.00158670708908915, 2.256160236439166411 ) ) ;
#93388 = CARTESIAN_POINT ( 'NONE',  ( 2.499999999999993783, 4.999999999999997335, 0.000000000000000000 ) ) ;
#93389 = CARTESIAN_POINT ( 'NONE',  ( 16.93201058511109380, 12.15574511561022852, 11.49999999999999645 ) ) ;
#93390 = VECTOR ( 'NONE', #11954, 1000.000000000000000 ) ;
#93391 = CARTESIAN_POINT ( 'NONE',  ( 29.74624769612771402, -6.376774720514427841, 26.55905195464798396 ) ) ;
#93392 = CARTESIAN_POINT ( 'NONE',  ( -39.62287095715005592, -29.50250243563736774, 8.947779886222148704 ) ) ;
#93393 = CARTESIAN_POINT ( 'NONE',  ( -48.62287095715004881, -23.47593901973091235, -1.443836447539009749 ) ) ;
#93394 = CARTESIAN_POINT ( 'NONE',  ( -19.99249555334884221, 7.427959064407942513, -1.500000000000002220 ) ) ;
#93395 = CARTESIAN_POINT ( 'NONE',  ( -31.24388727629348494, -24.86441894802673147, 8.247789967202360017 ) ) ;
#93396 = CARTESIAN_POINT ( 'NONE',  ( -124.5228709571500616, -24.50216790748203977, 0.6166512839542644953 ) ) ;
#93397 = CARTESIAN_POINT ( 'NONE',  ( -90.62287095715001328, -24.14321612903114556, -0.2833117244521682343 ) ) ;
#93398 = CARTESIAN_POINT ( 'NONE',  ( -5.063563723219555612, -5.876774720514409189, 19.46509473978807847 ) ) ;
#93399 = CARTESIAN_POINT ( 'NONE',  ( 22.09666729679958053, 4.251135690456572469, -1.500000000000002220 ) ) ;
#93400 = CARTESIAN_POINT ( 'NONE',  ( -108.8763703466142800, -25.32390614315827193, 4.358500768180118889 ) ) ;
#93401 = VERTEX_POINT ( 'NONE', #37202 ) ;
#93402 = DIRECTION ( 'NONE',  ( -3.773278334453079030E-23, 0.9999999999976377785, 2.173523156925979128E-06 ) ) ;
#93403 = CARTESIAN_POINT ( 'NONE',  ( 3.362850247043494001, -5.876774720514404748, 18.65880685207958223 ) ) ;
#93404 = CARTESIAN_POINT ( 'NONE',  ( -6.756748142665309764, -18.51622224137248907, 11.49999999999999645 ) ) ;
#93405 = CARTESIAN_POINT ( 'NONE',  ( -0.02075734969026423599, -5.965225279485572685, -0.08597719988137648983 ) ) ;
#93406 = B_SPLINE_CURVE_WITH_KNOTS ( 'NONE', 3,
 ( #80108, #48175, #1998, #87220, #40055, #9601 ),
 .UNSPECIFIED., .F., .F.,
 ( 4, 2, 4 ),
 ( 6.384118678613675148E-06, 0.001386860460828376936, 0.002767336802978140158 ),
 .UNSPECIFIED. ) ;
#93407 = CARTESIAN_POINT ( 'NONE',  ( -23.31187512739357359, -5.965225279485572685, -17.31005501743528185 ) ) ;
#93408 = EDGE_LOOP ( 'NONE', ( #37359, #54963, #41317, #45155 ) ) ;
#93409 = CARTESIAN_POINT ( 'NONE',  ( -29.49875734969026198, 0.3587747205144265483, 2.362022800118626531 ) ) ;
#93410 = CARTESIAN_POINT ( 'NONE',  ( -108.5562042904833930, -24.66019654487199730, 8.947790411086121054 ) ) ;
#93411 = CARTESIAN_POINT ( 'NONE',  ( -88.87354082327544802, -25.06732983082694588, 7.447789526168958396 ) ) ;
#93412 = VECTOR ( 'NONE', #95118, 1000.000000000000114 ) ;
#93413 = LINE ( 'NONE', #572, #23766 ) ;
#93414 = CARTESIAN_POINT ( 'NONE',  ( 17.05426814964238957, 9.943002105365778220, 11.49999999999998934 ) ) ;
#93415 = ORIENTED_EDGE ( 'NONE', *, *, #52435, .T. ) ;
#93416 = EDGE_CURVE ( 'NONE', #9293, #75450, #74529, .T. ) ;
#93417 = CARTESIAN_POINT ( 'NONE',  ( 5.271800844967073907, 3.316774720514426456, -28.56638892015272191 ) ) ;
#93418 = EDGE_CURVE ( 'NONE', #27652, #5624, #99081, .T. ) ;
#93419 = B_SPLINE_CURVE_WITH_KNOTS ( 'NONE', 3,
 ( #16147, #86164, #1441, #46617 ),
 .UNSPECIFIED., .F., .F.,
 ( 4, 4 ),
 ( 0.000000000000000000, 0.0001000000000000028644 ),
 .UNSPECIFIED. ) ;
#93420 = CALENDAR_DATE ( 2026, 9, 10 ) ;
#93421 = VERTEX_POINT ( 'NONE', #45322 ) ;
#93422 = CARTESIAN_POINT ( 'NONE',  ( 30.93860345374796594, 5.965225279485572685, 28.07639619989136293 ) ) ;
#93423 = DIRECTION ( 'NONE',  ( -3.773278334453079030E-23, 0.9999999999976377785, 2.173523156925979128E-06 ) ) ;
#93424 = LINE ( 'NONE', #94432, #71789 ) ;
#93425 = CARTESIAN_POINT ( 'NONE',  ( -99.83839741074528717, -25.26638519438374075, 7.461409190821002291 ) ) ;
#93426 = PLANE ( 'NONE',  #35549 ) ;
#93427 = DIRECTION ( 'NONE',  ( 0.1489078231574183508, -6.454799914155188842E-16, -0.9888510809027409865 ) ) ;
#93428 = CARTESIAN_POINT ( 'NONE',  ( -53.52287095715006870, -24.65952944569304606, 1.056160979905693686 ) ) ;
#93429 = CARTESIAN_POINT ( 'NONE',  ( -13.93161493328335432, -14.37010051631055418, -1.500000000000002220 ) ) ;
#93430 = EDGE_CURVE ( 'NONE', #31349, #78091, #24527, .T. ) ;
#93431 = CARTESIAN_POINT ( 'NONE',  ( -99.12380231474227799, -25.10935291788973345, 4.001575492514970911 ) ) ;
#93432 = CARTESIAN_POINT ( 'NONE',  ( 31.52563388547018874, -4.132774720514424516, -1.605328387144967728 ) ) ;
#93433 = EDGE_LOOP ( 'NONE', ( #74309, #44139, #20126, #72177 ) ) ;
#93434 = VECTOR ( 'NONE', #77923, 1000.000000000000114 ) ;
#93435 = CARTESIAN_POINT ( 'NONE',  ( 8.090164212199763227, -5.215366374113139081, -25.84881406240220869 ) ) ;
#93436 = CARTESIAN_POINT ( 'NONE',  ( -109.7896840091628832, -25.18430186498734358, 3.444318112836231904 ) ) ;
#93437 = CARTESIAN_POINT ( 'NONE',  ( -58.52287095715004739, -23.73934037231756022, 11.05740245334328797 ) ) ;
#93438 = CARTESIAN_POINT ( 'NONE',  ( -100.6228709571500559, -23.48786465467241769, 11.44779295918254114 ) ) ;
#93439 = LINE ( 'NONE', #39161, #46455 ) ;
#93440 = CARTESIAN_POINT ( 'NONE',  ( -51.70072539166533687, -25.31574255575237231, 3.987151966999201491 ) ) ;
#93441 = VECTOR ( 'NONE', #73389, 1000.000000000000114 ) ;
#93442 = FACE_OUTER_BOUND ( 'NONE', #5152, .T. ) ;
#93444 = VECTOR ( 'NONE', #37214, 1000.000000000000000 ) ;
#93443 = DIRECTION ( 'NONE',  ( 0.000000000000000000, 0.9999999999976377785, 2.173523156925979975E-06 ) ) ;
#93445 = ORIENTED_EDGE ( 'NONE', *, *, #67709, .T. ) ;
#93446 = AXIS2_PLACEMENT_3D ( 'NONE', #65218, #65711, #50463 ) ;
#93447 = CARTESIAN_POINT ( 'NONE',  ( 19.35245777310151993, -6.127589836641541332, -1.500000000000002220 ) ) ;
#93448 = DIRECTION ( 'NONE',  ( -0.5644074343637431879, 0.000000000000000000, 0.8254963646406547895 ) ) ;
#93449 = VECTOR ( 'NONE', #44249, 1000.000000000000114 ) ;
#93450 = DIRECTION ( 'NONE',  ( -3.773278334453079618E-23, 0.9999999999976377785, 2.173523156925979975E-06 ) ) ;
#93451 = ORIENTED_EDGE ( 'NONE', *, *, #6344, .F. ) ;
#93453 = EDGE_CURVE ( 'NONE', #98127, #20122, #131, .T. ) ;
#93452 = CARTESIAN_POINT ( 'NONE',  ( -113.5228709571500616, -29.50250243563736774, 8.947779886222136270 ) ) ;
#93454 = CARTESIAN_POINT ( 'NONE',  ( -19.30929855918770954, 5.666966705251045511, -1.500000000000002220 ) ) ;
#93455 = CARTESIAN_POINT ( 'NONE',  ( -15.55823947972799282, -14.28038451723262270, 11.49999999999999645 ) ) ;
#93456 = CARTESIAN_POINT ( 'NONE',  ( -16.97254739485517661, -14.18817111035334655, -1.500000000000002220 ) ) ;
#93457 = EDGE_CURVE ( 'NONE', #81901, #46658, #99638, .T. ) ;
#93458 = CARTESIAN_POINT ( 'NONE',  ( -18.11865614447288664, 9.752654332028551920, -1.500000000000002220 ) ) ;
#93459 = CARTESIAN_POINT ( 'NONE',  ( -60.63096549711488592, -24.73486907724917572, 1.287355809206962798 ) ) ;
#93460 = ORIENTED_EDGE ( 'NONE', *, *, #31358, .F. ) ;
#93461 = CARTESIAN_POINT ( 'NONE',  ( -27.86046284349297864, 6.376774720514426953, -8.091963836038765123 ) ) ;
#93462 = ORIENTED_EDGE ( 'NONE', *, *, #87942, .F. ) ;
#93463 = CARTESIAN_POINT ( 'NONE',  ( -6.775140224358976226, -6.376774720514408301, 19.14743589743590846 ) ) ;
#93464 = DIRECTION ( 'NONE',  ( -0.8264557562326033668, 6.845827386180409975E-16, -0.5630016722799281448 ) ) ;
#93465 = ORIENTED_EDGE ( 'NONE', *, *, #12771, .T. ) ;
#93466 = ORIENTED_EDGE ( 'NONE', *, *, #73670, .T. ) ;
#93467 = ORIENTED_EDGE ( 'NONE', *, *, #21128, .T. ) ;
#93468 = CARTESIAN_POINT ( 'NONE',  ( -53.62287095715005592, -29.50248528299804818, 1.056150453629033370 ) ) ;
#93469 = CARTESIAN_POINT ( 'NONE',  ( -63.62287095715004881, -24.51283580621364067, 0.6167428607019798115 ) ) ;
#93470 = CARTESIAN_POINT ( 'NONE',  ( 0.3376760108279234784, -6.376774720514417183, 20.09898898868105732 ) ) ;
#93471 = CARTESIAN_POINT ( 'NONE',  ( -18.80638259998596951, 8.471300643254643603, -1.500000000000002220 ) ) ;
#93472 = CARTESIAN_POINT ( 'NONE',  ( 21.54666897473465070, 1.519730039111064412, 11.49999999999999645 ) ) ;
#93473 = ORIENTED_EDGE ( 'NONE', *, *, #22218, .F. ) ;
#93474 = CYLINDRICAL_SURFACE ( 'NONE', #35309, 10.80000000000000782 ) ;
#93475 = VECTOR ( 'NONE', #38085, 999.9999999999998863 ) ;
#93476 = DIRECTION ( 'NONE',  ( 0.000000000000000000, -0.000000000000000000, -1.000000000000000000 ) ) ;
#93477 = CARTESIAN_POINT ( 'NONE',  ( -22.26391555059773353, 2.265117081278330780, 11.49999999999998934 ) ) ;
#93478 = CARTESIAN_POINT ( 'NONE',  ( -71.52287095715007581, -24.65952944569304606, 1.056160979905697239 ) ) ;
#93479 = CARTESIAN_POINT ( 'NONE',  ( -120.6228709571500559, -24.14406661707769786, 10.28769366152061160 ) ) ;
#93480 = ORIENTED_EDGE ( 'NONE', *, *, #96911, .T. ) ;
#93481 = CARTESIAN_POINT ( 'NONE',  ( 32.52533654608641456, -5.023480152701085721, -11.79063777444543781 ) ) ;
#93482 = CARTESIAN_POINT ( 'NONE',  ( -108.5228709571500616, -29.50248528299804818, 1.056150453629043584 ) ) ;
#93483 = AXIS2_PLACEMENT_3D ( 'NONE', #12400, #67216, #34754 ) ;
#93484 = CARTESIAN_POINT ( 'NONE',  ( -11.35812032211249090, 17.58211214940072864, -1.500000000000002220 ) ) ;
#93485 = ORIENTED_EDGE ( 'NONE', *, *, #25488, .F. ) ;
#93486 = EDGE_CURVE ( 'NONE', #54063, #25694, #77734, .T. ) ;
#93487 = CARTESIAN_POINT ( 'NONE',  ( 31.04236049493789906, -5.965225279485572685, 19.84760796525321780 ) ) ;
#93488 = CC_DESIGN_PERSON_AND_ORGANIZATION_ASSIGNMENT ( #32274, #47007, ( #3602 ) ) ;
#93489 = ORIENTED_EDGE ( 'NONE', *, *, #37308, .F. ) ;
#93490 = B_SPLINE_CURVE_WITH_KNOTS ( 'NONE', 3,
 ( #13004, #43970, #83013, #84018 ),
 .UNSPECIFIED., .F., .F.,
 ( 4, 4 ),
 ( 0.008354480413380572026, 0.009203042238611652825 ),
 .UNSPECIFIED. ) ;
#93491 = CARTESIAN_POINT ( 'NONE',  ( -128.6228709571500417, -24.64965695001469115, 8.947790433994173398 ) ) ;
#93492 = CARTESIAN_POINT ( 'NONE',  ( 3.428800225705347149, -20.88102749682517612, -1.500000000000002220 ) ) ;
#93493 = EDGE_LOOP ( 'NONE', ( #29363, #78077, #6313, #48944, #82006, #65813 ) ) ;
#93494 = CARTESIAN_POINT ( 'NONE',  ( -89.62287095715004170, -29.50247984919015209, -1.443849546365051806 ) ) ;
#93495 = CARTESIAN_POINT ( 'NONE',  ( -21.66901994843296819, -2.608494568651300138, 11.49999999999998934 ) ) ;
#93496 = CARTESIAN_POINT ( 'NONE',  ( -6.901944873432418248, -6.376774720514410077, 19.15221817653406688 ) ) ;
#93497 = CARTESIAN_POINT ( 'NONE',  ( 0.000000000000000000, -1.473225279485573802, 0.000000000000000000 ) ) ;
#93498 = CARTESIAN_POINT ( 'NONE',  ( -110.6228709571500701, -23.48783264082479505, -1.443836473390060160 ) ) ;
#93499 = CARTESIAN_POINT ( 'NONE',  ( 20.45693200876408469, 7.529271608661172621, -1.500000000000002220 ) ) ;
#93500 = CARTESIAN_POINT ( 'NONE',  ( 3.176458874063926352, 5.965225279485592225, -28.85257003503889095 ) ) ;
#93501 = ORIENTED_EDGE ( 'NONE', *, *, #81843, .F. ) ;
#93502 = CARTESIAN_POINT ( 'NONE',  ( 7.477175500793984853, -5.876774720514417183, 20.66439772633092176 ) ) ;
#93503 = DIRECTION ( 'NONE',  ( -0.000000000000000000, 1.000000000000000000, -0.000000000000000000 ) ) ;
#93504 = ORIENTED_EDGE ( 'NONE', *, *, #78480, .T. ) ;
#93505 = ADVANCED_FACE ( 'NONE', ( #48321 ), #63054, .F. ) ;
#93506 = AXIS2_PLACEMENT_3D ( 'NONE', #63866, #24760, #10543 ) ;
#93507 = VERTEX_POINT ( 'NONE', #18362 ) ;
#93508 = ORIENTED_EDGE ( 'NONE', *, *, #7328, .T. ) ;
#93509 = CARTESIAN_POINT ( 'NONE',  ( -58.52287095715006160, -24.64965694238407323, 8.947790433994201820 ) ) ;
#93510 = DIRECTION ( 'NONE',  ( -1.000000000000000000, -0.000000000000000000, -0.000000000000000000 ) ) ;
#93511 = CARTESIAN_POINT ( 'NONE',  ( 12.26186175617451113, -17.30295086655154080, -1.500000000000002220 ) ) ;
#93512 = CARTESIAN_POINT ( 'NONE',  ( -94.62561019970178222, -24.51314013834315375, 0.6176544820404151759 ) ) ;
#93513 = FACE_BOUND ( 'NONE', #21856, .T. ) ;
#93514 = AXIS2_PLACEMENT_3D ( 'NONE', #86975, #80873, #72772 ) ;
#93515 = DIRECTION ( 'NONE',  ( 0.000000000000000000, 0.000000000000000000, -1.000000000000000000 ) ) ;
#93516 = CARTESIAN_POINT ( 'NONE',  ( 7.305494252837257285, 17.95555029072639286, 11.49999999999998934 ) ) ;
#93517 = CARTESIAN_POINT ( 'NONE',  ( -41.88795169677845109, -25.25978494880519776, 3.590542803917028181 ) ) ;
#93518 = ORIENTED_EDGE ( 'NONE', *, *, #99013, .F. ) ;
#93519 = CARTESIAN_POINT ( 'NONE',  ( 10.22484414329051994, 16.58839404647166660, 11.49999999999999645 ) ) ;
#93520 = LINE ( 'NONE', #100115, #17969 ) ;
#93521 = CIRCLE ( 'NONE', #35242, 251.4258649670780699 ) ;
#93522 = EDGE_CURVE ( 'NONE', #17108, #16636, #9747, .T. ) ;
#93523 = CARTESIAN_POINT ( 'NONE',  ( -80.33862689906705157, -25.12417942247672542, 7.094867700071801231 ) ) ;
#93524 = ORIENTED_EDGE ( 'NONE', *, *, #24946, .F. ) ;
#93525 = CARTESIAN_POINT ( 'NONE',  ( -27.96875734969026084, -3.316774720514426456, 0.7300228001186309656 ) ) ;
#93526 = CARTESIAN_POINT ( 'NONE',  ( -97.62287095715005592, -29.50250786944525672, 11.44777988621623166 ) ) ;
#93527 = CARTESIAN_POINT ( 'NONE',  ( -30.50620355600309708, -23.47593905652042778, -1.426910232161149983 ) ) ;
#93528 = CARTESIAN_POINT ( 'NONE',  ( -93.59138280458586223, -24.15620529776628445, 10.23563542870659404 ) ) ;
#93529 = CARTESIAN_POINT ( 'NONE',  ( -6.620539020842763911, -18.51205181221761720, -1.500000000000002220 ) ) ;
#93530 = CARTESIAN_POINT ( 'NONE',  ( -41.46611000704998418, -25.27805945495849826, 4.188173683520152402 ) ) ;
#93531 = ORIENTED_EDGE ( 'NONE', *, *, #30131, .F. ) ;
#93532 = CARTESIAN_POINT ( 'NONE',  ( 21.36531308999010648, 3.172564587314818052, -1.500000000000002220 ) ) ;
#93533 = CARTESIAN_POINT ( 'NONE',  ( -40.57216908292625845, -25.00158670708910336, 2.256160236439222366 ) ) ;
#93534 = PLANE ( 'NONE',  #55289 ) ;
#93535 = CARTESIAN_POINT ( 'NONE',  ( -22.28253579152010033, 6.022996098971622914, -1.500000000000002220 ) ) ;
#93536 = EDGE_CURVE ( 'NONE', #93401, #23628, #30780, .T. ) ;
#93537 = CALENDAR_DATE ( 2026, 9, 10 ) ;
#93538 = CARTESIAN_POINT ( 'NONE',  ( -57.52287095715005449, -29.50248528299804818, 1.056150453629034924 ) ) ;
#93539 = CARTESIAN_POINT ( 'NONE',  ( -49.62287095715005592, -29.50250786944525672, 11.44777988621624054 ) ) ;
#93540 = LINE ( 'NONE', #207, #21741 ) ;
#93541 = CARTESIAN_POINT ( 'NONE',  ( -24.90875734969025501, -5.965225279485572685, 26.43402280011862615 ) ) ;
#93542 = CARTESIAN_POINT ( 'NONE',  ( -110.2102236481481015, -25.18562194707735813, 3.298800634353756589 ) ) ;
#93543 = CARTESIAN_POINT ( 'NONE',  ( -129.5221661632653536, -23.73766607897671221, -1.055555164236443577 ) ) ;
#93544 = CARTESIAN_POINT ( 'NONE',  ( -111.3738206124644279, -25.29779372368820134, 4.292346609405336189 ) ) ;
#93545 = CARTESIAN_POINT ( 'NONE',  ( -13.91458393394894166, 14.26456941660895339, 11.49999999999998934 ) ) ;
#93546 = EDGE_CURVE ( 'NONE', #15184, #42104, #5120, .T. ) ;
#93547 = CARTESIAN_POINT ( 'NONE',  ( -69.52287095715006160, -23.47593901973090169, -1.443836447538996870 ) ) ;
#93548 = CARTESIAN_POINT ( 'NONE',  ( -11.71124675921804403, 15.99993322257668282, -1.500000000000002220 ) ) ;
#93549 = VECTOR ( 'NONE', #25622, 1000.000000000000000 ) ;
#93550 = CARTESIAN_POINT ( 'NONE',  ( -0.2112149364088803105, -5.876774720514410077, 19.49357334786886398 ) ) ;
#93551 = B_SPLINE_CURVE_WITH_KNOTS ( 'NONE', 3,
 ( #79544, #50111, #81049, #19638 ),
 .UNSPECIFIED., .F., .F.,
 ( 4, 4 ),
 ( 0.000000000000000000, 0.0001000000000000167422 ),
 .UNSPECIFIED. ) ;
#93552 = CARTESIAN_POINT ( 'NONE',  ( -40.25203966287474344, -25.29116520055095663, 2.839406929231615528 ) ) ;
#93553 = CARTESIAN_POINT ( 'NONE',  ( -35.62287095715005592, -23.47596703998600276, 11.44779298504227505 ) ) ;
#93554 = CARTESIAN_POINT ( 'NONE',  ( -19.90621922972506397, 5.769413876575915978, 11.49999999999999645 ) ) ;
#93555 = AXIS2_PLACEMENT_3D ( 'NONE', #96410, #42642, #65490 ) ;
#93556 = CARTESIAN_POINT ( 'NONE',  ( -7.627782137226129855, -5.876774720514413630, 20.04377961306771994 ) ) ;
#93557 = CARTESIAN_POINT ( 'NONE',  ( -88.62287095715007013, -23.94994826722515668, -0.6494450866351709761 ) ) ;
#93558 = CARTESIAN_POINT ( 'NONE',  ( -6.081610112697643622, 21.96313418072945822, 11.49999999999999645 ) ) ;
#93559 = ORIENTED_EDGE ( 'NONE', *, *, #34440, .F. ) ;
#93560 = B_SPLINE_SURFACE_WITH_KNOTS ( 'NONE', 3, 3, ( 
 ( #32946, #26822, #65420, #11589 ),
 ( #33940, #88233, #33435, #87731 ),
 ( #49186, #88732, #50171, #73012 ),
 ( #55797, #24817, #48176, #94833 ),
 ( #25825, #79104, #81108, #57302 ),
 ( #18697, #64919, #86720, #79608 ),
 ( #96334, #42067, #40562, #3499 ),
 ( #25323, #95833, #72016, #10596 ),
 ( #41563, #56798, #26328, #80109 ),
 ( #49679, #64421, #71515, #80607 ) ),
 .UNSPECIFIED., .F., .F., .F.,
 ( 4, 3, 3, 4 ),
 ( 4, 4 ),
 ( 0.0004766839783818981654, 0.1491231665100171688, 0.2234464077758347988, 0.2977696490416524289 ),
 ( 0.3995422531334771321, 0.4007930632633419643 ),
 .UNSPECIFIED. ) ;
#93561 = LINE ( 'NONE', #24055, #5791 ) ;
#93562 = CARTESIAN_POINT ( 'NONE',  ( -74.62287095715005592, -23.48786465467241058, 11.44779295918254469 ) ) ;
#93563 = VERTEX_POINT ( 'NONE', #71156 ) ;
#93564 = CARTESIAN_POINT ( 'NONE',  ( -19.95319933381289701, -3.276446921841525306, 11.49999999999998934 ) ) ;
#93565 = CARTESIAN_POINT ( 'NONE',  ( 9.071512145086501278, -0.9000000000000000222, 2.133776825740807753E-15 ) ) ;
#93566 = CARTESIAN_POINT ( 'NONE',  ( -110.5228709571500616, -23.85229601348997264, 10.88205029486208630 ) ) ;
#93567 = ORIENTED_EDGE ( 'NONE', *, *, #87604, .F. ) ;
#93568 = AXIS2_PLACEMENT_3D ( 'NONE', #82682, #60375, #53250 ) ;
#93569 = VERTEX_POINT ( 'NONE', #79249 ) ;
#93570 = CARTESIAN_POINT ( 'NONE',  ( -2.499999999999993339, 19.99999999999999645, 2.100000000000000089 ) ) ;
#93571 = CARTESIAN_POINT ( 'NONE',  ( -21.13427563780003382, 8.902639844219676135, -1.500000000000002220 ) ) ;
#93572 = CARTESIAN_POINT ( 'NONE',  ( -51.29636648399702636, -25.18439796746319814, 3.969959851941196938 ) ) ;
#93573 = CARTESIAN_POINT ( 'NONE',  ( 11.61936018155104833, -18.21891831228114356, -1.500000000000002220 ) ) ;
#93574 = CARTESIAN_POINT ( 'NONE',  ( -104.6228709571500559, -23.48783264082478794, -1.443836473390062158 ) ) ;
#93575 = CARTESIAN_POINT ( 'NONE',  ( -20.02981537788295441, -6.213780249082809348, 11.49999999999999645 ) ) ;
#93576 = ORIENTED_EDGE ( 'NONE', *, *, #44028, .T. ) ;
#93577 = LINE ( 'NONE', #59795, #82583 ) ;
#93578 = CARTESIAN_POINT ( 'NONE',  ( -68.94044447473358161, -25.24754525613202460, 6.138838922787388519 ) ) ;
#93579 = CARTESIAN_POINT ( 'NONE',  ( -1.213202359833694732, 22.00568734548514627, -1.500000000000002220 ) ) ;
#93580 = CIRCLE ( 'NONE', #25521, 27.94799999999999685 ) ;
#93581 = CARTESIAN_POINT ( 'NONE',  ( -98.52287095715006160, -24.64965694238575011, 8.947790433994194714 ) ) ;
#93582 = CARTESIAN_POINT ( 'NONE',  ( -66.55620429048337883, -24.64965694238574656, 8.947790433994198267 ) ) ;
#93584 = ORIENTED_EDGE ( 'NONE', *, *, #13147, .T. ) ;
#93583 = EDGE_CURVE ( 'NONE', #53349, #13741, #92285, .T. ) ;
#93585 = DIRECTION ( 'NONE',  ( 0.000000000000000000, -1.000000000000000000, 0.000000000000000000 ) ) ;
#93586 = CARTESIAN_POINT ( 'NONE',  ( -122.6228709571500417, -24.50321055353805377, 9.387540953477525818 ) ) ;
#93587 = ORIENTED_EDGE ( 'NONE', *, *, #94892, .T. ) ;
#93588 = CARTESIAN_POINT ( 'NONE',  ( 3.552794897967157528, -6.376774720514401196, 18.18650940196788568 ) ) ;
#93589 = EDGE_LOOP ( 'NONE', ( #62561, #24864, #64929, #49498, #57766, #51692 ) ) ;
#93590 = VECTOR ( 'NONE', #25396, 1000.000000000000227 ) ;
#93591 = ORIENTED_EDGE ( 'NONE', *, *, #69966, .F. ) ;
#93592 = CARTESIAN_POINT ( 'NONE',  ( 26.73860345374794534, -5.058662225110310828, -7.113848178280766099 ) ) ;
#93593 = CARTESIAN_POINT ( 'NONE',  ( -95.62287095715002749, -25.00182538069145721, 7.747789668545097541 ) ) ;
#93594 = CARTESIAN_POINT ( 'NONE',  ( -36.52733198375308632, -24.65952944569304606, 1.056160979905694353 ) ) ;
#93595 = CARTESIAN_POINT ( 'NONE',  ( 16.11427877760282001, 12.65940972936023812, -1.500000000000002220 ) ) ;
#93596 = ORIENTED_EDGE ( 'NONE', *, *, #22103, .T. ) ;
#93597 = CARTESIAN_POINT ( 'NONE',  ( -99.83650425372744053, -25.30067960901012825, 5.350007036700404228 ) ) ;
#93598 = CARTESIAN_POINT ( 'NONE',  ( -44.49966819881763769, -24.15543982623906771, -0.2315651400026670914 ) ) ;
#93599 = FACE_OUTER_BOUND ( 'NONE', #87844, .T. ) ;
#93600 = CARTESIAN_POINT ( 'NONE',  ( 22.08996893241407378, 3.065900275835479860, -1.500000000000002220 ) ) ;
#93601 = CARTESIAN_POINT ( 'NONE',  ( -70.56836343276164314, -25.13731425188323954, 7.077682618907291889 ) ) ;
#93602 = CARTESIAN_POINT ( 'NONE',  ( -27.33175959122838350, -24.62075588168795903, 8.217702253644940669 ) ) ;
#93603 = ORIENTED_EDGE ( 'NONE', *, *, #44413, .F. ) ;
#93604 = CARTESIAN_POINT ( 'NONE',  ( -28.17037414371105086, -24.65651949530377962, 1.683498270968381005 ) ) ;
#93605 = CARTESIAN_POINT ( 'NONE',  ( 7.160000000000000142, 8.500000000000000000, 6.788828319098143993 ) ) ;
#93606 = CARTESIAN_POINT ( 'NONE',  ( -14.80784184970232431, -14.63167926507950689, 11.49999999999998934 ) ) ;
#93607 = EDGE_LOOP ( 'NONE', ( #32028, #69932, #88533, #86452 ) ) ;
#93608 = B_SPLINE_CURVE_WITH_KNOTS ( 'NONE', 3,
 ( #47861, #1182, #8791, #94020 ),
 .UNSPECIFIED., .F., .F.,
 ( 4, 4 ),
 ( 0.8904217528559288386, 0.8994281841280442613 ),
 .UNSPECIFIED. ) ;
#93610 = ORIENTED_EDGE ( 'NONE', *, *, #83449, .F. ) ;
#93609 = CARTESIAN_POINT ( 'NONE',  ( -51.58953762381672448, -24.64898659630367206, 1.056161002820380279 ) ) ;
#93611 = EDGE_CURVE ( 'NONE', #21327, #98355, #94811, .T. ) ;
#93612 = ORIENTED_EDGE ( 'NONE', *, *, #63457, .F. ) ;
#93613 = CARTESIAN_POINT ( 'NONE',  ( -51.38881019666819583, -25.12217764763901329, 6.651362562939564071 ) ) ;
#93614 = CARTESIAN_POINT ( 'NONE',  ( 19.96068868648078620, -6.529529906025321573, -1.500000000000002220 ) ) ;
#93615 = EDGE_CURVE ( 'NONE', #72949, #42580, #14812, .T. ) ;
#93616 = VERTEX_POINT ( 'NONE', #31578 ) ;
#93617 = CARTESIAN_POINT ( 'NONE',  ( -110.6228709571500985, -24.62226745350443124, 0.9660975649729638404 ) ) ;
#93618 = LINE ( 'NONE', #62702, #17225 ) ;
#93619 = CARTESIAN_POINT ( 'NONE',  ( -29.49875734969025842, -0.3587747205144265483, 17.86602280011862476 ) ) ;
#93620 = LINE ( 'NONE', #68805, #58272 ) ;
#93621 = CARTESIAN_POINT ( 'NONE',  ( -59.53434381846648904, -24.65952944569304961, 1.056160979905697905 ) ) ;
#93622 = CARTESIAN_POINT ( 'NONE',  ( -57.52287095715004739, -23.73907113216988307, -1.053371485793252571 ) ) ;
#93624 = ORIENTED_EDGE ( 'NONE', *, *, #49137, .F. ) ;
#93623 = CARTESIAN_POINT ( 'NONE',  ( -19.97062832128981213, -9.750827054148329509, 11.49999999999999645 ) ) ;
#93625 = CARTESIAN_POINT ( 'NONE',  ( -98.93782592301593581, -25.29244077744215247, 5.755742261006358440 ) ) ;
#93626 = DIRECTION ( 'NONE',  ( 3.773278334444167608E-23, -1.000000000000000000, 0.000000000000000000 ) ) ;
#93627 = EDGE_LOOP ( 'NONE', ( #6091, #5499, #15403, #2167 ) ) ;
#93628 = CARTESIAN_POINT ( 'NONE',  ( -18.33335541821337245, -13.34141728429830742, -1.500000000000002220 ) ) ;
#93629 = AXIS2_PLACEMENT_3D ( 'NONE', #12028, #4926, #52098 ) ;
#93630 = ADVANCED_FACE ( 'NONE', ( #86372 ), #47316, .T. ) ;
#93631 = EDGE_CURVE ( 'NONE', #18728, #71622, #54930, .T. ) ;
#93633 = ORIENTED_EDGE ( 'NONE', *, *, #65723, .F. ) ;
#93632 = DIRECTION ( 'NONE',  ( -3.773278334453080206E-23, 0.9999999999976377785, 2.173523156925979975E-06 ) ) ;
#93634 = EDGE_LOOP ( 'NONE', ( #29953, #94077, #19492, #35235 ) ) ;
#93635 = EDGE_CURVE ( 'NONE', #49044, #65549, #30649, .T. ) ;
#93636 = DIRECTION ( 'NONE',  ( 0.000000000000000000, 1.000000000000000000, 0.000000000000000000 ) ) ;
#93637 = CARTESIAN_POINT ( 'NONE',  ( -10.68008619461380704, -17.10268970254769982, -1.500000000000002220 ) ) ;
#93638 = CARTESIAN_POINT ( 'NONE',  ( -80.62287095715005592, -23.85196035786901092, -0.8779234886474913679 ) ) ;
#93639 = ORIENTED_EDGE ( 'NONE', *, *, #52810, .T. ) ;
#93640 = CARTESIAN_POINT ( 'NONE',  ( -108.6228709571500417, -23.47596703998600631, 11.44779298504227860 ) ) ;
#93641 = CARTESIAN_POINT ( 'NONE',  ( 14.42577177192597482, -17.14957960503723911, -1.500000000000002220 ) ) ;
#93642 = EDGE_CURVE ( 'NONE', #47809, #81499, #89956, .T. ) ;
#93643 = B_SPLINE_CURVE_WITH_KNOTS ( 'NONE', 3,
 ( #44542, #75466, #5970, #6476, #53661, #67888 ),
 .UNSPECIFIED., .F., .F.,
 ( 4, 2, 4 ),
 ( 1.570755371634092017E-05, 0.001396183895866087970, 0.002776660238015834711 ),
 .UNSPECIFIED. ) ;
#93644 = ORIENTED_EDGE ( 'NONE', *, *, #77702, .T. ) ;
#93645 = EDGE_LOOP ( 'NONE', ( #78001, #60864, #42885, #87453 ) ) ;
#93646 = DIRECTION ( 'NONE',  ( -1.000000000000000000, -0.000000000000000000, -0.000000000000000000 ) ) ;
#93647 = CARTESIAN_POINT ( 'NONE',  ( -119.6228709571500559, -23.72773821059535493, 11.05748984161097503 ) ) ;
#93648 = CARTESIAN_POINT ( 'NONE',  ( -39.47555198290115186, -25.30229325268190976, 4.430735662431675159 ) ) ;
#93649 = CARTESIAN_POINT ( 'NONE',  ( 13.91401389203221406, -5.965225279485572685, 158.0376437107427137 ) ) ;
#93650 = VECTOR ( 'NONE', #28279, 1000.000000000000114 ) ;
#93651 = B_SPLINE_CURVE_WITH_KNOTS ( 'NONE', 3,
 ( #60508, #52881, #83820, #16809, #32539, #77688 ),
 .UNSPECIFIED., .F., .F.,
 ( 4, 2, 4 ),
 ( 1.570755371633875854E-05, 0.001396183895866086235, 0.002776660238015833410 ),
 .UNSPECIFIED. ) ;
#93652 = CARTESIAN_POINT ( 'NONE',  ( -97.25033046169170348, -24.47827083238275847, 0.5637492489085987879 ) ) ;
#93653 = CARTESIAN_POINT ( 'NONE',  ( -9.112395119859147741, -17.30902560603237106, -1.500000000000002220 ) ) ;
#93654 = LINE ( 'NONE', #77920, #66907 ) ;
#93655 = ORIENTED_EDGE ( 'NONE', *, *, #1196, .T. ) ;
#93656 = CARTESIAN_POINT ( 'NONE',  ( 15.57385778016992894, -14.83193121981731544, -1.500000000000002220 ) ) ;
#93657 = CARTESIAN_POINT ( 'NONE',  ( -62.52287095715010423, -24.35013146730203815, 9.818937971375104823 ) ) ;
#93658 = DIRECTION ( 'NONE',  ( 0.000000000000000000, 1.000000000000000000, 0.000000000000000000 ) ) ;
#93659 = DIRECTION ( 'NONE',  ( -0.000000000000000000, 0.000000000000000000, 1.000000000000000000 ) ) ;
#93660 = CARTESIAN_POINT ( 'NONE',  ( -4.929522925832171332, -6.376774720514426953, -28.63504101147569614 ) ) ;
#93661 = CARTESIAN_POINT ( 'NONE',  ( 7.824713763024562674, 21.46283361357968289, -1.500000000000002220 ) ) ;
#93662 = ADVANCED_FACE ( 'NONE', ( #74150 ), #66569, .T. ) ;
#93663 = VECTOR ( 'NONE', #75262, 1000.000000000000227 ) ;
#93664 = EDGE_CURVE ( 'NONE', #71246, #30854, #95605, .T. ) ;
#93665 = APPROVAL_STATUS ( 'not_yet_approved' ) ;
#93666 = CARTESIAN_POINT ( 'NONE',  ( -101.5562042904833930, -23.47593901973091235, -1.443836447539001089 ) ) ;
#93667 = CARTESIAN_POINT ( 'NONE',  ( -2.188401442307694289, -5.876774720514411854, 19.46153846153846700 ) ) ;
#93668 = CARTESIAN_POINT ( 'NONE',  ( -15.86121933104946535, 12.22609501325904624, 11.49999999999999645 ) ) ;
#93669 = CARTESIAN_POINT ( 'NONE',  ( -79.67189865184847974, -25.31594350486923872, 4.664461505014560139 ) ) ;
#93670 = CARTESIAN_POINT ( 'NONE',  ( -10.34999999999999254, 4.999999999999999112, 2.100000000000000089 ) ) ;
#93671 = CIRCLE ( 'NONE', #56472, 6.594667762285749468 ) ;
#93672 = CYLINDRICAL_SURFACE ( 'NONE', #65206, 28.45799999999999486 ) ;
#93673 = CARTESIAN_POINT ( 'NONE',  ( 13.91401389203221406, 6.475225279485573360, 27.24920385068457662 ) ) ;
#93674 = EDGE_LOOP ( 'NONE', ( #61334, #88918, #53804, #95756 ) ) ;
#93675 = DIRECTION ( 'NONE',  ( 0.000000000000000000, -2.173523156925980399E-06, 0.9999999999976378895 ) ) ;
#93676 = EDGE_CURVE ( 'NONE', #1756, #13745, #42226, .T. ) ;
#93677 = CARTESIAN_POINT ( 'NONE',  ( -20.93004649427559016, -6.003493321846349318, 11.49999999999998934 ) ) ;
#93678 = CARTESIAN_POINT ( 'NONE',  ( -56.62287095715004881, -24.66019654487199020, 8.947790411086131712 ) ) ;
#93679 = CARTESIAN_POINT ( 'NONE',  ( 8.085132396474181249, 17.94908993440701295, -1.500000000000002220 ) ) ;
#93680 = CARTESIAN_POINT ( 'NONE',  ( -124.6228709571500559, -29.50248528299804818, 1.056150453629045360 ) ) ;
#93681 = EDGE_CURVE ( 'NONE', #16362, #42205, #80250, .T. ) ;
#93682 = ADVANCED_FACE ( 'NONE', ( #36086, #34096, #97963, #90368 ), #73159, .F. ) ;
#93683 = CARTESIAN_POINT ( 'NONE',  ( -40.58380419742159262, -25.18557147773197968, 3.298448857756749231 ) ) ;
#93684 = COORDINATED_UNIVERSAL_TIME_OFFSET ( 0, 0, .AHEAD. ) ;
#93685 = CYLINDRICAL_SURFACE ( 'NONE', #93728, 4.450000000000000178 ) ;
#93686 = CARTESIAN_POINT ( 'NONE',  ( -73.62287095715007013, -23.96177878511307568, 10.65340807706329862 ) ) ;
#93687 = CARTESIAN_POINT ( 'NONE',  ( 18.81462172601333549, -8.267562025728075525, 11.49999999999999645 ) ) ;
#93688 = DIRECTION ( 'NONE',  ( -0.03244919754393515293, 0.000000000000000000, 0.9994733861282923959 ) ) ;
#93689 = DIRECTION ( 'NONE',  ( -0.000000000000000000, -0.000000000000000000, -1.000000000000000000 ) ) ;
#93690 = CARTESIAN_POINT ( 'NONE',  ( -15.94491270116497184, -16.04792668696150315, 11.49999999999999645 ) ) ;
#93691 = VERTEX_POINT ( 'NONE', #12731 ) ;
#93692 = FACE_OUTER_BOUND ( 'NONE', #50056, .T. ) ;
#93693 = CARTESIAN_POINT ( 'NONE',  ( -37.52287095715006870, -24.50216790748204687, 0.6166512839542470648 ) ) ;
#93694 = CARTESIAN_POINT ( 'NONE',  ( -125.5892681715929342, -24.73531770709095312, 8.716586749053508498 ) ) ;
#93695 = B_SPLINE_CURVE_WITH_KNOTS ( 'NONE', 3,
 ( #48139, #84680, #1461, #69462 ),
 .UNSPECIFIED., .F., .F.,
 ( 4, 4 ),
 ( 0.3107218788879825278, 0.3197283101600981170 ),
 .UNSPECIFIED. ) ;
#93696 = CARTESIAN_POINT ( 'NONE',  ( -85.62287095715001328, -24.92579138211019796, 1.929029949965662460 ) ) ;
#93697 = CARTESIAN_POINT ( 'NONE',  ( -25.54628175542703161, -24.93063037130169235, 5.501430938224779688 ) ) ;
#93698 = CARTESIAN_POINT ( 'NONE',  ( -2.762050907158362989, -6.376774720514415407, 19.89644244529369033 ) ) ;
#93699 = ORIENTED_EDGE ( 'NONE', *, *, #11498, .T. ) ;
#93700 = CARTESIAN_POINT ( 'NONE',  ( -79.38647268321243189, -25.26750025236339070, 5.652477768429786664 ) ) ;
#93701 = CARTESIAN_POINT ( 'NONE',  ( 7.682656365740156090, -21.48159684637525046, 11.49999999999998934 ) ) ;
#93702 = CARTESIAN_POINT ( 'NONE',  ( 4.647383884978952828, -5.876774720514412742, 19.72975307774251164 ) ) ;
#93703 = B_SPLINE_SURFACE_WITH_KNOTS ( 'NONE', 3, 3, ( 
 ( #8036, #86661, #24754, #92764 ),
 ( #86163, #16644, #32886, #34755 ),
 ( #16146, #32378, #71454, #70445 ),
 ( #424, #39991, #46615, #77537 ),
 ( #62340, #80928, #19021, #9038 ),
 ( #15647, #78534, #85158, #93772 ),
 ( #63354, #31376, #93266, #47117 ) ),
 .UNSPECIFIED., .F., .F., .F.,
 ( 4, 3, 4 ),
 ( 4, 4 ),
 ( 0.0004766839783822478748, 0.1029713700210899419, 0.2054660560637976419 ),
 ( 0.08951676878467576537, 0.09057079621334723774 ),
 .UNSPECIFIED. ) ;
#93704 = CARTESIAN_POINT ( 'NONE',  ( -96.50858727277388027, -24.51314013834316086, 0.6176544820404197278 ) ) ;
#93705 = CARTESIAN_POINT ( 'NONE',  ( -86.52287095715003318, -24.33927499327855770, 9.819080762295811837 ) ) ;
#93706 = CARTESIAN_POINT ( 'NONE',  ( 6.968497804723354783, -21.30229754059623559, 11.49999999999999645 ) ) ;
#93707 = ORIENTED_EDGE ( 'NONE', *, *, #25474, .T. ) ;
#93708 = CARTESIAN_POINT ( 'NONE',  ( -70.62287095715005592, -23.85229601348997264, 10.88205029486207920 ) ) ;
#93709 = CARTESIAN_POINT ( 'NONE',  ( -3.149188516569510377, 21.71089317892358395, -1.500000000000002220 ) ) ;
#93710 = B_SPLINE_CURVE_WITH_KNOTS ( 'NONE', 3,
 ( #17874, #26495, #2664, #34607 ),
 .UNSPECIFIED., .F., .F.,
 ( 4, 4 ),
 ( 0.7210148590621303644, 0.7300212903342458981 ),
 .UNSPECIFIED. ) ;
#93711 = DIRECTION ( 'NONE',  ( 0.000000000000000000, 0.5144957554275265688, -0.8574929257125440962 ) ) ;
#93712 = CARTESIAN_POINT ( 'NONE',  ( -44.48765446362095588, -24.51419770103159479, 9.386484678747171628 ) ) ;
#93713 = CARTESIAN_POINT ( 'NONE',  ( -74.58953762381673869, -23.48786465467241058, 11.44779295918254469 ) ) ;
#93714 = EDGE_LOOP ( 'NONE', ( #55667, #6299, #60946, #7914 ) ) ;
#93715 = LINE ( 'NONE', #57189, #26567 ) ;
#93716 = CARTESIAN_POINT ( 'NONE',  ( 9.543201319291914093E-14, -6.376774720514426953, 18.21871304725679508 ) ) ;
#93717 = ORIENTED_EDGE ( 'NONE', *, *, #65280, .T. ) ;
#93718 = CARTESIAN_POINT ( 'NONE',  ( -7.302954156136775232, -19.11528491071161540, 11.49999999999998934 ) ) ;
#93719 = VERTEX_POINT ( 'NONE', #95986 ) ;
#93720 = VERTEX_POINT ( 'NONE', #3650 ) ;
#93721 = ORIENTED_EDGE ( 'NONE', *, *, #55776, .F. ) ;
#93722 = ORIENTED_EDGE ( 'NONE', *, *, #32659, .T. ) ;
#93723 = CARTESIAN_POINT ( 'NONE',  ( 5.395019145045520048, -22.42585393411717121, 11.49999999999998934 ) ) ;
#93724 = CARTESIAN_POINT ( 'NONE',  ( -94.52287095715006160, -29.50250243563736774, 8.947779886222139822 ) ) ;
#93725 = CARTESIAN_POINT ( 'NONE',  ( 5.353267490507026771, -19.58905154090721368, -1.500000000000002220 ) ) ;
#93726 = ORIENTED_EDGE ( 'NONE', *, *, #66202, .F. ) ;
#93727 = FACE_OUTER_BOUND ( 'NONE', #20393, .T. ) ;
#93728 = AXIS2_PLACEMENT_3D ( 'NONE', #38905, #86077, #30796 ) ;
#93729 = CARTESIAN_POINT ( 'NONE',  ( -92.64086922289898496, -23.48783264082478084, -1.443836473390064157 ) ) ;
#93730 = DIRECTION ( 'NONE',  ( 0.000000000000000000, 0.9999999999976377785, 2.173523156925979128E-06 ) ) ;
#93731 = CARTESIAN_POINT ( 'NONE',  ( 4.653733606810938284, -6.376774720514411854, 19.95301661664751336 ) ) ;
#93733 = ORIENTED_EDGE ( 'NONE', *, *, #95584, .F. ) ;
#93732 = CARTESIAN_POINT ( 'NONE',  ( 21.49998558720804809, 0.1351929536555107336, 11.49999999999999645 ) ) ;
#93734 = DIRECTION ( 'NONE',  ( 0.000000000000000000, -0.9999999999976377785, -2.173523156925979128E-06 ) ) ;
#93735 = CARTESIAN_POINT ( 'NONE',  ( -29.52287095715006160, -24.56560739788454129, 1.056161319240904728 ) ) ;
#93736 = ORIENTED_EDGE ( 'NONE', *, *, #86197, .T. ) ;
#93737 = B_SPLINE_CURVE_WITH_KNOTS ( 'NONE', 3,
 ( #88630, #25719, #46691, #70013, #72909, #19099, #48582, #57198, #57685, #23832, #77110 ),
 .UNSPECIFIED., .F., .F.,
 ( 4, 1, 1, 1, 1, 1, 1, 1, 4 ),
 ( 0.000000000000000000, 0.1105883385953350950, 0.2245417540535963874, 0.3425034940501046066, 0.4643240984173571118, 0.5907560327017662427, 0.7222274753555133486, 0.8588428362087243695, 1.000000000000000000 ),
 .UNSPECIFIED. ) ;
#93738 = CARTESIAN_POINT ( 'NONE',  ( 15.70846742882596025, 13.54617332914617478, 11.49999999999998934 ) ) ;
#93739 = ORIENTED_EDGE ( 'NONE', *, *, #12968, .F. ) ;
#93741 = ORIENTED_EDGE ( 'NONE', *, *, #35271, .T. ) ;
#93740 = CARTESIAN_POINT ( 'NONE',  ( -28.98875734969026041, 5.965225279485572685, 25.61802280011862720 ) ) ;
#93742 = ADVANCED_FACE ( 'NONE', ( #59426 ), #50819, .T. ) ;
#93743 = CARTESIAN_POINT ( 'NONE',  ( -41.55302297196116967, -23.96169478059712787, 10.65365249895718591 ) ) ;
#93745 = CARTESIAN_POINT ( 'NONE',  ( -48.52287095715004028, -23.73907113217710574, -1.053371485780553174 ) ) ;
#93744 = B_SPLINE_CURVE_WITH_KNOTS ( 'NONE', 3,
 ( #30988, #46218, #14254, #29986 ),
 .UNSPECIFIED., .F., .F.,
 ( 4, 4 ),
 ( 0.000000000000000000, 1.000000000000000000 ),
 .UNSPECIFIED. ) ;
#93746 = ORIENTED_EDGE ( 'NONE', *, *, #40918, .F. ) ;
#93747 = ORIENTED_EDGE ( 'NONE', *, *, #16061, .F. ) ;
#93748 = ADVANCED_FACE ( 'NONE', ( #35598 ), #26484, .F. ) ;
#93749 = CARTESIAN_POINT ( 'NONE',  ( -109.6228709571500559, -23.47596703998600631, 11.44779298504227860 ) ) ;
#93750 = AXIS2_PLACEMENT_3D ( 'NONE', #72006, #46665, #47165 ) ;
#93751 = CARTESIAN_POINT ( 'NONE',  ( -92.62287095715005592, -29.50247984919015209, -1.443849546365051806 ) ) ;
#93752 = CARTESIAN_POINT ( 'NONE',  ( 22.81105451610979173, -6.475225279485573360, -18.46691820600746681 ) ) ;
#93753 = CARTESIAN_POINT ( 'NONE',  ( 22.04941498731238525, 0.3350016526185666255, 11.49999999999999645 ) ) ;
#93754 = ADVANCED_FACE ( 'NONE', ( #81258 ), #20340, .T. ) ;
#93755 = CARTESIAN_POINT ( 'NONE',  ( -89.60222329899340821, -23.48786465467241058, 11.44779295918254114 ) ) ;
#93756 = CARTESIAN_POINT ( 'NONE',  ( -20.69567741759225399, -9.018594580484563750, -1.500000000000002220 ) ) ;
#93757 = EDGE_CURVE ( 'NONE', #50276, #95120, #34596, .T. ) ;
#93758 = CARTESIAN_POINT ( 'NONE',  ( 20.48634023128459347, 4.603634630958829632, 11.49999999999998934 ) ) ;
#93759 = EDGE_CURVE ( 'NONE', #65481, #37559, #16085, .T. ) ;
#93760 = CARTESIAN_POINT ( 'NONE',  ( 9.071512145086501278, 0.000000000000000000, -3.687490859131163479 ) ) ;
#93762 = VERTEX_POINT ( 'NONE', #58928 ) ;
#93761 = CARTESIAN_POINT ( 'NONE',  ( -100.3686125512453344, -25.31369796955044649, 5.218484686103943559 ) ) ;
#93763 = VECTOR ( 'NONE', #23933, 1000.000000000000000 ) ;
#93764 = ORIENTED_EDGE ( 'NONE', *, *, #68022, .F. ) ;
#93765 = EDGE_CURVE ( 'NONE', #85538, #93093, #65536, .T. ) ;
#93766 = CARTESIAN_POINT ( 'NONE',  ( -80.62287095715008434, -24.62226745350438151, 0.9660975649728147374 ) ) ;
#93767 = FACE_OUTER_BOUND ( 'NONE', #61909, .T. ) ;
#93768 = ORIENTED_EDGE ( 'NONE', *, *, #29018, .T. ) ;
#93769 = CARTESIAN_POINT ( 'NONE',  ( 6.139388171429570384, 20.22809724653347985, 11.49999999999998934 ) ) ;
#93770 = PLANE ( 'NONE',  #70880 ) ;
#93771 = CARTESIAN_POINT ( 'NONE',  ( -58.85623904670280382, -25.31249728293746060, 5.276660823416808199 ) ) ;
#93772 = CARTESIAN_POINT ( 'NONE',  ( -121.5186340557655029, -24.51314013834315375, 0.6176544820404190617 ) ) ;
#93773 = CARTESIAN_POINT ( 'NONE',  ( -51.62287095715005592, -23.47593901973091235, -1.443836447539009749 ) ) ;
#93774 = CARTESIAN_POINT ( 'NONE',  ( -101.5228709571501327, -24.34917612406837861, 0.1852690917426578765 ) ) ;
#93775 = CARTESIAN_POINT ( 'NONE',  ( 7.537409830304743430, 20.87355781386819942, -1.500000000000002220 ) ) ;
#93776 = CARTESIAN_POINT ( 'NONE',  ( -81.55064642742604519, -24.15620529776628089, 10.23563542870661180 ) ) ;
#93777 = EDGE_CURVE ( 'NONE', #61899, #99097, #17163, .T. ) ;
#93778 = VERTEX_POINT ( 'NONE', #69031 ) ;
#93779 = DIRECTION ( 'NONE',  ( 0.000000000000000000, 0.000000000000000000, -1.000000000000000000 ) ) ;
#93780 = DIRECTION ( 'NONE',  ( -1.000000000000000000, -3.491481338843133355E-15, -2.352173255807796056E-16 ) ) ;
#93781 = CARTESIAN_POINT ( 'NONE',  ( -40.25429027579533425, -25.30394352446274553, 5.534647984323703973 ) ) ;
#93782 = CARTESIAN_POINT ( 'NONE',  ( -100.5472838704266820, -24.73486907724917927, 1.287355809206965240 ) ) ;
#93783 = CARTESIAN_POINT ( 'NONE',  ( 11.19917779851249939, -2.682774720514424782, -27.04477526052296099 ) ) ;
#93784 = EDGE_CURVE ( 'NONE', #19391, #93232, #68535, .T. ) ;
#93785 = CARTESIAN_POINT ( 'NONE',  ( 19.40022266231057202, 1.907866353064612053, 11.49999999999998934 ) ) ;
#93786 = CARTESIAN_POINT ( 'NONE',  ( 21.30238844577196389, 2.035401582669650544, -1.500000000000002220 ) ) ;
#93787 = CARTESIAN_POINT ( 'NONE',  ( -62.53912049199733758, -24.51314013834316441, 0.6176544820404141767 ) ) ;
#93788 = CARTESIAN_POINT ( 'NONE',  ( -60.56964542493874859, -23.48786465467241413, 11.44779295918254824 ) ) ;
#93789 = DIRECTION ( 'NONE',  ( 0.000000000000000000, 0.000000000000000000, -1.000000000000000000 ) ) ;
#93790 = CARTESIAN_POINT ( 'NONE',  ( -100.9649361822203133, -25.27360005675012999, 3.436944093663774957 ) ) ;
#93791 = CARTESIAN_POINT ( 'NONE',  ( 16.14549698687068968, 15.95341496147077720, -1.500000000000002220 ) ) ;
#93792 = EDGE_CURVE ( 'NONE', #95598, #30477, #59985, .T. ) ;
#93793 = B_SPLINE_CURVE_WITH_KNOTS ( 'NONE', 3,
 ( #64459, #55828, #2536, #25860, #78623, #56834, #17243, #63957, #24358, #71044, #47707, #87767, #48211, #18249 ),
 .UNSPECIFIED., .F., .F.,
 ( 4, 2, 2, 2, 2, 2, 4 ),
 ( 1.734723475976807094E-18, 0.0001838431575664456984, 0.0003676863151328896621, 0.0007353726302657787820, 0.001103058945398667848, 0.001286902102965092973, 0.001470745260531517882 ),
 .UNSPECIFIED. ) ;
#93794 = DIRECTION ( 'NONE',  ( -1.000000000000000000, 0.000000000000000000, 0.000000000000000000 ) ) ;
#93795 = CARTESIAN_POINT ( 'NONE',  ( -98.62287095715005592, -24.34917612406837861, 0.1852690917426657036 ) ) ;
#93796 = CARTESIAN_POINT ( 'NONE',  ( -10.37884456512175291, 16.95428827495986823, 11.49999999999999645 ) ) ;
#93797 = FACE_OUTER_BOUND ( 'NONE', #22514, .T. ) ;
#93798 = CIRCLE ( 'NONE', #82423, 4.080000000000000071 ) ;
#93800 = B_SPLINE_CURVE_WITH_KNOTS ( 'NONE', 3,
 ( #77931, #8443, #39392, #70346 ),
 .UNSPECIFIED., .F., .F.,
 ( 4, 4 ),
 ( 0.6902788356978080131, 0.6992852669699235468 ),
 .UNSPECIFIED. ) ;
#93799 = CARTESIAN_POINT ( 'NONE',  ( -88.62287095715004170, -24.64898659630367916, 1.056161002820827921 ) ) ;
#93801 = DIRECTION ( 'NONE',  ( -3.773278334453079030E-23, 0.9999999999976377785, 2.173523156925979128E-06 ) ) ;
#93802 = VERTEX_POINT ( 'NONE', #99959 ) ;
#93803 = CARTESIAN_POINT ( 'NONE',  ( 29.73860345376319003, 5.356471260711259674, 19.84760796525321780 ) ) ;
#93804 = FACE_OUTER_BOUND ( 'NONE', #47268, .T. ) ;
#93805 = CARTESIAN_POINT ( 'NONE',  ( -117.5228709571500332, -24.66019654487200441, 8.947790411086108620 ) ) ;
#93806 = CARTESIAN_POINT ( 'NONE',  ( 2.849777056880220982, 21.50153301832798647, -1.500000000000002220 ) ) ;
#93807 = CARTESIAN_POINT ( 'NONE',  ( -56.63256087942864525, -24.35071581493543391, 9.817618358456030592 ) ) ;
#93808 = CIRCLE ( 'NONE', #4723, 91.74549126261079834 ) ;
#93809 = CARTESIAN_POINT ( 'NONE',  ( 19.32586673001642197, -2.567307930040524599, -1.500000000000002220 ) ) ;
#93810 = CARTESIAN_POINT ( 'NONE',  ( -55.57509330567962991, -25.00182538069146432, 7.747789668545041586 ) ) ;
#93811 = EDGE_CURVE ( 'NONE', #73380, #48269, #13731, .T. ) ;
#93812 = ORIENTED_EDGE ( 'NONE', *, *, #37526, .T. ) ;
#93813 = AXIS2_PLACEMENT_3D ( 'NONE', #65658, #71248, #57539 ) ;
#93814 = CARTESIAN_POINT ( 'NONE',  ( 7.100489274569507181, 19.11111018586187527, 11.49999999999999645 ) ) ;
#93815 = CARTESIAN_POINT ( 'NONE',  ( -80.62512171223323776, -24.92564183028979130, 1.928384488918253536 ) ) ;
#93816 = EDGE_CURVE ( 'NONE', #43961, #63898, #86176, .T. ) ;
#93817 = LINE ( 'NONE', #46657, #50868 ) ;
#93818 = VERTEX_POINT ( 'NONE', #53819 ) ;
#93819 = CARTESIAN_POINT ( 'NONE',  ( -40.94445540056845800, -25.20887482615457742, 3.394058116165219907 ) ) ;
#93820 = CARTESIAN_POINT ( 'NONE',  ( 32.84232313084928023, 4.840274619472680229, -11.71291885348849782 ) ) ;
#93821 = CARTESIAN_POINT ( 'NONE',  ( -48.87464133331025806, -25.25214680837418868, 6.106125007117622516 ) ) ;
#93822 = VECTOR ( 'NONE', #59794, 1000.000000000000114 ) ;
#93823 = CARTESIAN_POINT ( 'NONE',  ( -40.64047108292161425, -24.52399227489126687, 9.353111116836521077 ) ) ;
#93824 = CARTESIAN_POINT ( 'NONE',  ( -52.62287095715005592, -24.64898659630367561, 1.056161002820821038 ) ) ;
#93825 = CARTESIAN_POINT ( 'NONE',  ( 19.93115673323400117, -2.579441489355707606, -1.500000000000002220 ) ) ;
#93826 = B_SPLINE_CURVE_WITH_KNOTS ( 'NONE', 3,
 ( #83580, #28305, #28803, #52147, #91689, #68372 ),
 .UNSPECIFIED., .F., .F.,
 ( 4, 2, 4 ),
 ( 0.002936590050694640099, 0.005175337996430707382, 0.007414085942166775967 ),
 .UNSPECIFIED. ) ;
#93827 = EDGE_CURVE ( 'NONE', #28958, #40199, #30469, .T. ) ;
#93828 = CARTESIAN_POINT ( 'NONE',  ( -109.5940810882278100, -23.73766607897670156, -1.055555164236452681 ) ) ;
#93829 = ORIENTED_EDGE ( 'NONE', *, *, #52665, .F. ) ;
#93830 = DIRECTION ( 'NONE',  ( 0.000000000000000000, 0.000000000000000000, -1.000000000000000000 ) ) ;
#93831 = CARTESIAN_POINT ( 'NONE',  ( 16.68310095749102118, 15.68496000196893370, 11.49999999999999645 ) ) ;
#93832 = CARTESIAN_POINT ( 'NONE',  ( -10.65177407370799045, -20.06881281718593613, -1.500000000000002220 ) ) ;
#93833 = VERTEX_POINT ( 'NONE', #13232 ) ;
#93834 = CARTESIAN_POINT ( 'NONE',  ( -30.47287095715006799, -25.10154806753639889, 7.245676043324505322 ) ) ;
#93835 = CARTESIAN_POINT ( 'NONE',  ( -96.52287095715006160, -29.50250786944525672, 11.44777988621623166 ) ) ;
#93836 = CARTESIAN_POINT ( 'NONE',  ( -40.14865555004231368, -25.20037933810821684, 3.331970962322966301 ) ) ;
#93837 = CARTESIAN_POINT ( 'NONE',  ( -30.57287095715006586, -24.92127980078614158, 8.082355342557208999 ) ) ;
#93838 = CARTESIAN_POINT ( 'NONE',  ( -128.6243654585905176, -23.48786465467241769, 11.44779295918253403 ) ) ;
#93839 = AXIS2_PLACEMENT_3D ( 'NONE', #2852, #34293, #3358 ) ;
#93840 = DIRECTION ( 'NONE',  ( 0.000000000000000000, 1.000000000000000000, 0.000000000000000000 ) ) ;
#93841 = ORIENTED_EDGE ( 'NONE', *, *, #90424, .F. ) ;
#93842 = CARTESIAN_POINT ( 'NONE',  ( 19.91419669613914678, 4.404666692190684962, -1.500000000000002220 ) ) ;
#93843 = ORIENTED_EDGE ( 'NONE', *, *, #3401, .F. ) ;
#93844 = B_SPLINE_CURVE_WITH_KNOTS ( 'NONE', 3,
 ( #83359, #28583, #37197, #28093, #74262, #44819, #99077, #45317, #67167, #5246, #37690, #44323, #30070, #50936 ),
 .UNSPECIFIED., .F., .F.,
 ( 4, 2, 2, 2, 2, 2, 4 ),
 ( 4.336808689942017736E-18, 0.0002426843972675349858, 0.0004853687945350656347, 0.0009707375890701099106, 0.001456106383605154132, 0.001698790780872676135, 0.001941475178140198571 ),
 .UNSPECIFIED. ) ;
#93845 = CARTESIAN_POINT ( 'NONE',  ( -21.75629724252761577, 7.406401271465676395, -1.500000000000002220 ) ) ;
#93846 = DIRECTION ( 'NONE',  ( -0.000000000000000000, 1.000000000000000000, -0.000000000000000000 ) ) ;
#93847 = PLANE ( 'NONE',  #51738 ) ;
#93848 = ORIENTED_EDGE ( 'NONE', *, *, #16327, .T. ) ;
#93849 = CARTESIAN_POINT ( 'NONE',  ( -126.5228709571500616, -29.50248528299804818, 1.056150453629047137 ) ) ;
#93850 = DIRECTION ( 'NONE',  ( 0.000000000000000000, 0.000000000000000000, -1.000000000000000000 ) ) ;
#93852 = ORIENTED_EDGE ( 'NONE', *, *, #83668, .T. ) ;
#93851 = CARTESIAN_POINT ( 'NONE',  ( 21.17668642892995834, 2.279540523802085605, 11.49999999999999645 ) ) ;
#93853 = ORIENTED_EDGE ( 'NONE', *, *, #86992, .F. ) ;
#93854 = CARTESIAN_POINT ( 'NONE',  ( -4.330935931041660858, -21.79039167146679290, 11.49999999999998934 ) ) ;
#93855 = CARTESIAN_POINT ( 'NONE',  ( -7.851838630353038972, -19.11370409007043847, 11.49999999999998934 ) ) ;
#93856 = ORIENTED_EDGE ( 'NONE', *, *, #86430, .T. ) ;
#93857 = CARTESIAN_POINT ( 'NONE',  ( -109.5136315545911856, -25.27682841784137935, 5.394825679379001926 ) ) ;
#93858 = EDGE_CURVE ( 'NONE', #79844, #42155, #52215, .T. ) ;
#93859 = CARTESIAN_POINT ( 'NONE',  ( -70.78925874883387337, -25.32724624944561853, 4.398071659717722959 ) ) ;
#93860 = ORIENTED_EDGE ( 'NONE', *, *, #66917, .T. ) ;
#93861 = EDGE_CURVE ( 'NONE', #17304, #41475, #53484, .T. ) ;
#93862 = LINE ( 'NONE', #95867, #85066 ) ;
#93863 = VECTOR ( 'NONE', #7339, 1000.000000000000114 ) ;
#93864 = ORIENTED_EDGE ( 'NONE', *, *, #8299, .T. ) ;
#93866 = EDGE_CURVE ( 'NONE', #1645, #34336, #28965, .T. ) ;
#93865 = CARTESIAN_POINT ( 'NONE',  ( -58.62366816843541528, -24.66019654487199730, 8.947790411086117501 ) ) ;
#93867 = PLANE ( 'NONE',  #53625 ) ;
#93868 = CARTESIAN_POINT ( 'NONE',  ( -19.30504728598367237, -7.930543132070424051, -1.500000000000002220 ) ) ;
#93869 = CARTESIAN_POINT ( 'NONE',  ( 12.58402814888991372, -17.87355554032721372, 11.49999999999999645 ) ) ;
#93870 = EDGE_CURVE ( 'NONE', #21622, #72523, #83250, .T. ) ;
#93871 = CARTESIAN_POINT ( 'NONE',  ( -102.6228709571500843, -24.51387760970724372, 9.387446482453405849 ) ) ;
#93872 = DIRECTION ( 'NONE',  ( -0.4725087886537609472, 0.000000000000000000, -0.8813259582271223413 ) ) ;
#93873 = CARTESIAN_POINT ( 'NONE',  ( 22.48569338394020534, -0.9006126209707296937, 11.49999999999998934 ) ) ;
#93874 = AXIS2_PLACEMENT_3D ( 'NONE', #25484, #63573, #3663 ) ;
#93875 = EDGE_CURVE ( 'NONE', #43355, #39879, #60441, .T. ) ;
#93876 = PLANE ( 'NONE',  #2830 ) ;
#93877 = CARTESIAN_POINT ( 'NONE',  ( -50.52287095715005449, -24.15516710230293640, 10.28746687063726029 ) ) ;
#93878 = CARTESIAN_POINT ( 'NONE',  ( -78.62287095715007013, -23.48783264082478439, -1.443836473390065711 ) ) ;
#93879 = ORIENTED_EDGE ( 'NONE', *, *, #26083, .T. ) ;
#93880 = VECTOR ( 'NONE', #13325, 1000.000000000000000 ) ;
#93881 = ORIENTED_EDGE ( 'NONE', *, *, #14770, .F. ) ;
#93882 = VECTOR ( 'NONE', #66546, 1000.000000000000000 ) ;
#93883 = ORIENTED_EDGE ( 'NONE', *, *, #70858, .F. ) ;
#93884 = ORIENTED_EDGE ( 'NONE', *, *, #13569, .F. ) ;
#93885 = CARTESIAN_POINT ( 'NONE',  ( 3.659817510876246960, 21.07357064420920878, -1.500000000000002220 ) ) ;
#93886 = CARTESIAN_POINT ( 'NONE',  ( -3.695635658436464244, 22.08213133993951161, 11.49999999999999645 ) ) ;
#93887 = ORIENTED_EDGE ( 'NONE', *, *, #64854, .F. ) ;
#93888 = CARTESIAN_POINT ( 'NONE',  ( 9.758084087097168791, -18.66043984184860349, 11.49999999999998934 ) ) ;
#93889 = CARTESIAN_POINT ( 'NONE',  ( -30.40154451732978913, -25.30207583497731250, 6.147639284700202822 ) ) ;
#93890 = CARTESIAN_POINT ( 'NONE',  ( -8.813339738934139689, -17.91118242276673911, -1.500000000000002220 ) ) ;
#93891 = CARTESIAN_POINT ( 'NONE',  ( -20.27875734969026311, 3.456774720514426136, 24.00402280011862288 ) ) ;
#93892 = CARTESIAN_POINT ( 'NONE',  ( -49.21454750704995007, -25.13877828889947352, 7.069183601642414772 ) ) ;
#93893 = CARTESIAN_POINT ( 'NONE',  ( 19.14557405504459453, -10.84957060938160289, -1.500000000000002220 ) ) ;
#93894 = CARTESIAN_POINT ( 'NONE',  ( -83.52287095715006160, -24.64898659630367916, 1.056161002820826145 ) ) ;
#93895 = EDGE_LOOP ( 'NONE', ( #2443, #58502, #21006, #10996 ) ) ;
#93896 = CARTESIAN_POINT ( 'NONE',  ( -30.64643901537730741, -23.50397814795999096, 11.46586199002818418 ) ) ;
#93897 = CARTESIAN_POINT ( 'NONE',  ( -54.58953762381671737, -23.47596703998600276, 11.44779298504227505 ) ) ;
#93898 = CARTESIAN_POINT ( 'NONE',  ( -20.61801493038525379, 2.926015819835423581, 11.49999999999999645 ) ) ;
#93899 = CARTESIAN_POINT ( 'NONE',  ( 31.61557479013570315, -6.410763075590560689, 26.52166531862750176 ) ) ;
#93900 = CARTESIAN_POINT ( 'NONE',  ( 11.62916340711181284, -5.965225279485572685, 28.75961759920349792 ) ) ;
#93901 = CARTESIAN_POINT ( 'NONE',  ( -25.92875734969025814, 3.316774720514426456, 24.50402280011861933 ) ) ;
#93902 = CARTESIAN_POINT ( 'NONE',  ( -6.620899627221215944, -20.26055204357936290, 11.49999999999998934 ) ) ;
#93903 = DIRECTION ( 'NONE',  ( 1.000000000000000000, 3.773278334444167608E-23, 8.201307833595939069E-29 ) ) ;
#93904 = DIRECTION ( 'NONE',  ( 1.000000000000000000, 0.000000000000000000, 0.000000000000000000 ) ) ;
#93905 = DIRECTION ( 'NONE',  ( 0.000000000000000000, -2.173523156925979552E-06, 0.9999999999976378895 ) ) ;
#93906 = LINE ( 'NONE', #86795, #81583 ) ;
#93907 = CARTESIAN_POINT ( 'NONE',  ( -17.96456891314058879, -13.58578184957126034, -1.500000000000002220 ) ) ;
#93908 = CYLINDRICAL_SURFACE ( 'NONE', #23118, 1.249999999999997558 ) ;
#93909 = EDGE_LOOP ( 'NONE', ( #72407, #52569, #99584, #63558 ) ) ;
#93910 = CARTESIAN_POINT ( 'NONE',  ( -79.39735417168856202, -25.30496935757056676, 4.861733025172510381 ) ) ;
#93911 = CARTESIAN_POINT ( 'NONE',  ( 2.903846153846159517, -5.876774720514415407, 19.99999999999999289 ) ) ;
#93912 = CARTESIAN_POINT ( 'NONE',  ( 13.13437215454093199, 14.66711140016434278, 11.49999999999999645 ) ) ;
#93913 = CARTESIAN_POINT ( 'NONE',  ( -55.62287095715004170, -25.00182538069145011, 7.747789668545097541 ) ) ;
#93914 = DIRECTION ( 'NONE',  ( -1.000000000000000000, -3.773278334444167608E-23, -8.201307837791369499E-29 ) ) ;
#93915 = ORIENTED_EDGE ( 'NONE', *, *, #42293, .F. ) ;
#93916 = CARTESIAN_POINT ( 'NONE',  ( -99.51916590676324859, -23.73766607897671577, -1.055555164236429366 ) ) ;
#93917 = CARTESIAN_POINT ( 'NONE',  ( -55.62287095715005592, -23.84047902841601285, -0.8780736468305797571 ) ) ;
#93918 = CARTESIAN_POINT ( 'NONE',  ( -30.57287095715006231, -23.47594215783195537, -5.102550391006585557E-05 ) ) ;
#93919 = EDGE_CURVE ( 'NONE', #61427, #71750, #89776, .T. ) ;
#93920 = FACE_OUTER_BOUND ( 'NONE', #38531, .T. ) ;
#93921 = CARTESIAN_POINT ( 'NONE',  ( -0.9724026449420489771, -19.73431249065222204, -1.500000000000002220 ) ) ;
#93922 = ORIENTED_EDGE ( 'NONE', *, *, #13692, .T. ) ;
#93923 = CARTESIAN_POINT ( 'NONE',  ( 15.73562052650688514, -12.66937975264744587, 11.49999999999999645 ) ) ;
#93924 = CARTESIAN_POINT ( 'NONE',  ( 6.055070915967790235, 6.376774720520797857, -28.43998667026512095 ) ) ;
#93926 = EDGE_CURVE ( 'NONE', #89711, #20834, #40596, .T. ) ;
#93925 = VECTOR ( 'NONE', #64661, 1000.000000000000227 ) ;
#93927 = CALENDAR_DATE ( 2026, 9, 10 ) ;
#93928 = ADVANCED_FACE ( 'NONE', ( #39078 ), #23438, .T. ) ;
#93929 = ORIENTED_EDGE ( 'NONE', *, *, #89394, .T. ) ;
#93930 = CARTESIAN_POINT ( 'NONE',  ( -107.6228709571500843, -24.51283580621364422, 0.6167428607019860287 ) ) ;
#93931 = CARTESIAN_POINT ( 'NONE',  ( -65.52287095715006160, -23.48786465467241058, 11.44779295918254647 ) ) ;
#93932 = CARTESIAN_POINT ( 'NONE',  ( -59.62287095715006302, -23.48786465467241058, 11.44779295918254824 ) ) ;
#93933 = LINE ( 'NONE', #16309, #17721 ) ;
#93934 = VECTOR ( 'NONE', #21932, 1000.000000000000114 ) ;
#93935 = CARTESIAN_POINT ( 'NONE',  ( -79.62287095715005592, -29.50248528299804818, 1.056150453629038477 ) ) ;
#93936 = DIRECTION ( 'NONE',  ( 1.000000000000000000, 3.773278334444167608E-23, 8.201307833595939069E-29 ) ) ;
#93937 = CARTESIAN_POINT ( 'NONE',  ( -18.86779840422491716, -6.689013621249945807, 11.49999999999998934 ) ) ;
#93938 = CARTESIAN_POINT ( 'NONE',  ( -99.77116551335946326, -25.27532895947881642, 2.990445617998676031 ) ) ;
#93939 = CARTESIAN_POINT ( 'NONE',  ( -45.52197096335316928, -23.48786465467240347, 11.44779295918255002 ) ) ;
#93940 = ORIENTED_EDGE ( 'NONE', *, *, #76950, .T. ) ;
#93941 = AXIS2_PLACEMENT_3D ( 'NONE', #55836, #94873, #56343 ) ;
#93942 = AXIS2_PLACEMENT_3D ( 'NONE', #52429, #61547, #22938 ) ;
#93943 = CARTESIAN_POINT ( 'NONE',  ( 8.524890150443020786, -5.131488666162827172, -25.99302514158824096 ) ) ;
#93944 = CARTESIAN_POINT ( 'NONE',  ( -109.3750630267952317, -25.18430312985891462, 4.026263409152782025 ) ) ;
#93945 = DIRECTION ( 'NONE',  ( -3.773278334453079030E-23, 0.9999999999976377785, 2.173523156925979128E-06 ) ) ;
#93946 = FACE_OUTER_BOUND ( 'NONE', #16894, .T. ) ;
#93947 = AXIS2_PLACEMENT_3D ( 'NONE', #69996, #84716, #32437 ) ;
#93948 = CYLINDRICAL_SURFACE ( 'NONE', #39933, 1.000000000000000222 ) ;
#93949 = CARTESIAN_POINT ( 'NONE',  ( -83.59947554517194135, -23.73766607897670511, -1.055555164236457122 ) ) ;
#93950 = AXIS2_PLACEMENT_3D ( 'NONE', #7165, #8176, #7672 ) ;
#93951 = CARTESIAN_POINT ( 'NONE',  ( -2.806649551956928335, -5.876774720514411854, 19.35116211686183618 ) ) ;
#93952 = CARTESIAN_POINT ( 'NONE',  ( -73.62287095715007013, -23.73907113216990794, -1.053371485793229700 ) ) ;
#93953 = ORIENTED_EDGE ( 'NONE', *, *, #86761, .T. ) ;
#93954 = CARTESIAN_POINT ( 'NONE',  ( 6.844040470191356640, -19.11863935190610064, 11.49999999999998934 ) ) ;
#93955 = CARTESIAN_POINT ( 'NONE',  ( 31.63608487984670958, 3.398012287350409277, 27.34773272911736797 ) ) ;
#93956 = CARTESIAN_POINT ( 'NONE',  ( -59.65601704802426752, -23.48786465467240703, 11.44779295918255180 ) ) ;
#93957 = ORIENTED_EDGE ( 'NONE', *, *, #14833, .F. ) ;
#93958 = ADVANCED_FACE ( 'NONE', ( #64458 ), #79638, .F. ) ;
#93959 = CARTESIAN_POINT ( 'NONE',  ( -94.55620429048339304, -23.47596703998600631, 11.44779298504227683 ) ) ;
#93960 = CARTESIAN_POINT ( 'NONE',  ( 19.60372117168125072, 4.849774137724135237, -1.500000000000002220 ) ) ;
#93961 = CARTESIAN_POINT ( 'NONE',  ( 20.71511372717374755, 4.256074106246791722, 11.49999999999999645 ) ) ;
#93962 = CARTESIAN_POINT ( 'NONE',  ( -19.88706384024380824, 9.709922325909349894, -1.500000000000002220 ) ) ;
#93963 = CARTESIAN_POINT ( 'NONE',  ( -14.18348626307465743, -14.89297910716571849, -1.500000000000002220 ) ) ;
#93964 = B_SPLINE_CURVE_WITH_KNOTS ( 'NONE', 3,
 ( #36685, #51919, #83347, #67650, #27082, #52414 ),
 .UNSPECIFIED., .F., .F.,
 ( 4, 2, 4 ),
 ( 0.000000000000000000, 0.001380901958385387894, 0.002761803916770775788 ),
 .UNSPECIFIED. ) ;
#93965 = DIRECTION ( 'NONE',  ( -3.773278334453079030E-23, 0.9999999999976377785, 2.173523156925979128E-06 ) ) ;
#93966 = ORIENTED_EDGE ( 'NONE', *, *, #84226, .F. ) ;
#93967 = CARTESIAN_POINT ( 'NONE',  ( -116.5562042904833646, -24.64965694238575011, 8.947790433994187609 ) ) ;
#93968 = ORIENTED_EDGE ( 'NONE', *, *, #98126, .T. ) ;
#93969 = FACE_OUTER_BOUND ( 'NONE', #20248, .T. ) ;
#93970 = CARTESIAN_POINT ( 'NONE',  ( -110.6228709571501128, -24.63345952396255356, 9.038047939301508293 ) ) ;
#93971 = ORIENTED_EDGE ( 'NONE', *, *, #20660, .T. ) ;
#93973 = VERTEX_POINT ( 'NONE', #47706 ) ;
#93972 = EDGE_CURVE ( 'NONE', #82993, #48082, #9635, .T. ) ;
#93974 = VERTEX_POINT ( 'NONE', #39583 ) ;
#93975 = CARTESIAN_POINT ( 'NONE',  ( -103.6228709571500559, -23.48786465467241769, 11.44779295918254114 ) ) ;
#93976 = FACE_OUTER_BOUND ( 'NONE', #97637, .T. ) ;
#93977 = CARTESIAN_POINT ( 'NONE',  ( 0.3545156366401029935, -6.376774720514413630, 20.17598923696321478 ) ) ;
#93978 = CARTESIAN_POINT ( 'NONE',  ( 12.98984941077313415, -16.12360325096057423, -1.500000000000002220 ) ) ;
#93979 = CARTESIAN_POINT ( 'NONE',  ( 13.45394552336293614, 17.01807010946250287, 11.49999999999999645 ) ) ;
#93980 = ORIENTED_EDGE ( 'NONE', *, *, #28693, .F. ) ;
#93981 = EDGE_CURVE ( 'NONE', #27297, #24485, #1023, .T. ) ;
#93982 = LINE ( 'NONE', #84372, #41829 ) ;
#93983 = CARTESIAN_POINT ( 'NONE',  ( -6.660000000000001030, 0.000000000000000000, 0.000000000000000000 ) ) ;
#93984 = CARTESIAN_POINT ( 'NONE',  ( -17.59303920844588376, -13.82112144285918731, -1.500000000000002220 ) ) ;
#93985 = EDGE_CURVE ( 'NONE', #80499, #41151, #54745, .T. ) ;
#93986 = CARTESIAN_POINT ( 'NONE',  ( -47.55322324058889194, -23.96169478059712432, 10.65365249895718591 ) ) ;
#93987 = FACE_OUTER_BOUND ( 'NONE', #20362, .T. ) ;
#93988 = EDGE_LOOP ( 'NONE', ( #38963, #25045, #24589, #51933 ) ) ;
#93989 = CARTESIAN_POINT ( 'NONE',  ( -35.57452074104147499, -23.48786465467240347, 11.44779295918255180 ) ) ;
#93990 = EDGE_CURVE ( 'NONE', #10184, #89509, #91024, .T. ) ;
#93991 = EDGE_CURVE ( 'NONE', #6499, #57568, #71626, .T. ) ;
#93992 = ORIENTED_EDGE ( 'NONE', *, *, #9386, .T. ) ;
#93993 = VECTOR ( 'NONE', #76860, 1000.000000000000114 ) ;
#93994 = CARTESIAN_POINT ( 'NONE',  ( -70.52287095715007581, -23.48783264082477018, -1.443836473390089914 ) ) ;
#93995 = EDGE_LOOP ( 'NONE', ( #47592, #34957, #12782, #55200 ) ) ;
#93996 = B_SPLINE_CURVE_WITH_KNOTS ( 'NONE', 3,
 ( #42611, #96880, #27372, #58332, #19737, #84520, #30230, #53094 ),
 .UNSPECIFIED., .F., .F.,
 ( 4, 2, 2, 4 ),
 ( -0.001240666984356060716, -0.0002401179793396601269, 0.0007604310256767404623, 0.002761529035709539039 ),
 .UNSPECIFIED. ) ;
#93997 = CARTESIAN_POINT ( 'NONE',  ( -101.2228709571500644, -23.47596703998600631, 11.44779298504227683 ) ) ;
#93998 = CARTESIAN_POINT ( 'NONE',  ( -6.524719417830534773, 20.15472526627327454, -1.500000000000002220 ) ) ;
#93999 = VERTEX_POINT ( 'NONE', #81652 ) ;
#94000 = CARTESIAN_POINT ( 'NONE',  ( -50.64241578966740320, -24.40034930558991277, 0.3402023900116070698 ) ) ;
#94001 = CARTESIAN_POINT ( 'NONE',  ( -6.457742198559264679, -20.83860622980983024, -1.500000000000002220 ) ) ;
#94002 = CARTESIAN_POINT ( 'NONE',  ( -7.640838998533831194, -6.376774720514417183, 20.32624910079993086 ) ) ;
#94003 = AXIS2_PLACEMENT_3D ( 'NONE', #67054, #57448, #50322 ) ;
#94004 = CARTESIAN_POINT ( 'NONE',  ( 6.698292889820671725, -6.376774720514424288, 21.80822233811499444 ) ) ;
#94005 = CARTESIAN_POINT ( 'NONE',  ( -116.6228709571500559, -24.65952944569305316, 1.056160979905706121 ) ) ;
#94006 = CARTESIAN_POINT ( 'NONE',  ( -21.69466673205137752, 2.402554924997643226, -1.500000000000002220 ) ) ;
#94007 = CARTESIAN_POINT ( 'NONE',  ( -95.52287095715007581, -24.15431212366388536, -0.2830839119429101047 ) ) ;
#94008 = ORIENTED_EDGE ( 'NONE', *, *, #74793, .T. ) ;
#94009 = ADVANCED_FACE ( 'NONE', ( #64957 ), #20140, .T. ) ;
#94010 = CARTESIAN_POINT ( 'NONE',  ( 7.190659024148910561, -5.876774720514414518, 19.91543959911579620 ) ) ;
#94011 = DIRECTION ( 'NONE',  ( 0.000000000000000000, 0.000000000000000000, 1.000000000000000000 ) ) ;
#94012 = EDGE_LOOP ( 'NONE', ( #97149, #52741, #27227, #93116 ) ) ;
#94013 = AXIS2_PLACEMENT_3D ( 'NONE', #18822, #87847, #80736 ) ;
#94014 = CARTESIAN_POINT ( 'NONE',  ( -110.0174630698386693, -25.31122420432532394, 5.385070121809086174 ) ) ;
#94015 = ORIENTED_EDGE ( 'NONE', *, *, #21227, .T. ) ;
#94016 = VECTOR ( 'NONE', #3923, 1000.000000000000000 ) ;
#94017 = EDGE_LOOP ( 'NONE', ( #37193, #31815, #95229 ) ) ;
#94018 = CARTESIAN_POINT ( 'NONE',  ( -27.75920500495050192, -24.77795200822517430, 2.278718183652751250 ) ) ;
#94019 = AXIS2_PLACEMENT_3D ( 'NONE', #26343, #64436, #65929 ) ;
#94020 = CARTESIAN_POINT ( 'NONE',  ( -120.5228709571500616, -23.47593901973090524, -1.443836447538996204 ) ) ;
#94021 = CARTESIAN_POINT ( 'NONE',  ( 14.73992482348874411, 15.29747818672187165, -1.500000000000002220 ) ) ;
#94022 = CARTESIAN_POINT ( 'NONE',  ( 0.000000000000000000, -16.94322527948557422, 3.500000000000000000 ) ) ;
#94023 = FACE_OUTER_BOUND ( 'NONE', #32714, .T. ) ;
#94024 = FACE_OUTER_BOUND ( 'NONE', #54658, .T. ) ;
#94025 = CARTESIAN_POINT ( 'NONE',  ( -40.62287095715005592, -23.48786465467240347, 11.44779295918255180 ) ) ;
#94026 = AXIS2_PLACEMENT_3D ( 'NONE', #70574, #17793, #47242 ) ;
#94027 = CARTESIAN_POINT ( 'NONE',  ( 19.37663158793545293, -0.8356294931911363300, -1.500000000000002220 ) ) ;
#94028 = LINE ( 'NONE', #26021, #55529 ) ;
#94029 = VERTEX_POINT ( 'NONE', #18248 ) ;
#94030 = CARTESIAN_POINT ( 'NONE',  ( 19.40022266231057202, 1.907866353064612053, 11.49999999999999645 ) ) ;
#94031 = DIRECTION ( 'NONE',  ( 1.000000000000000000, 0.000000000000000000, 0.000000000000000000 ) ) ;
#94032 = CARTESIAN_POINT ( 'NONE',  ( -79.49204124755721068, -25.20847803697028411, 6.537282351667380809 ) ) ;
#94033 = EDGE_CURVE ( 'NONE', #40045, #25965, #82584, .T. ) ;
#94034 = ORIENTED_EDGE ( 'NONE', *, *, #54540, .T. ) ;
#94035 = CARTESIAN_POINT ( 'NONE',  ( 4.931367317174526477, -6.376774720514420736, 20.61012727089847019 ) ) ;
#94036 = CARTESIAN_POINT ( 'NONE',  ( -89.52215898723319754, -23.48783264082478084, -1.443836473390068598 ) ) ;
#94037 = CARTESIAN_POINT ( 'NONE',  ( -91.62287095714998486, -24.33927499327853639, 9.819080762295815390 ) ) ;
#94038 = EDGE_CURVE ( 'NONE', #32327, #99093, #44784, .T. ) ;
#94039 = DIRECTION ( 'NONE',  ( 0.000000000000000000, -1.000000000000000000, 0.000000000000000000 ) ) ;
#94040 = CARTESIAN_POINT ( 'NONE',  ( -18.74838588596843181, -5.942601993926947657, -1.500000000000002220 ) ) ;
#94041 = ORIENTED_EDGE ( 'NONE', *, *, #8029, .F. ) ;
#94042 = CARTESIAN_POINT ( 'NONE',  ( 21.32721141102669193, -3.434809268862642817, -1.500000000000002220 ) ) ;
#94043 = CARTESIAN_POINT ( 'NONE',  ( -85.52287095715003318, -25.00182538069145011, 7.747789668545101094 ) ) ;
#94044 = CARTESIAN_POINT ( 'NONE',  ( -20.77875734969026311, 5.356774720514425603, 0.7300228001186309656 ) ) ;
#94045 = CARTESIAN_POINT ( 'NONE',  ( 8.651921485055520833, -21.43433228965458781, -1.500000000000002220 ) ) ;
#94046 = ADVANCED_FACE ( 'NONE', ( #80148 ), #15340, .T. ) ;
#94047 = APPROVAL_ROLE ( '' ) ;
#94048 = EDGE_CURVE ( 'NONE', #93616, #19525, #45641, .T. ) ;
#94049 = CARTESIAN_POINT ( 'NONE',  ( 3.206569032998081603, -6.376774720514424288, 21.19686455982786200 ) ) ;
#94050 = CARTESIAN_POINT ( 'NONE',  ( 26.25551457520356635, 4.772774720514425972, -10.59759736550661913 ) ) ;
#94051 = FACE_OUTER_BOUND ( 'NONE', #60797, .T. ) ;
#94052 = CARTESIAN_POINT ( 'NONE',  ( -104.5228709571500474, -24.33927499327855060, 9.819080762295804732 ) ) ;
#94053 = CARTESIAN_POINT ( 'NONE',  ( -110.8797149084312537, -25.29823833487873586, 2.935127919112444861 ) ) ;
#94054 = CARTESIAN_POINT ( 'NONE',  ( -98.52287095715007581, -23.47593901973090524, -1.443836447538996648 ) ) ;
#94055 = CARTESIAN_POINT ( 'NONE',  ( -114.5511084051358921, -24.66019654487200441, 8.947790411086106843 ) ) ;
#94056 = CARTESIAN_POINT ( 'NONE',  ( 5.901097582950029619, 19.04237314665466485, -1.500000000000002220 ) ) ;
#94057 = CARTESIAN_POINT ( 'NONE',  ( -75.55240587615696768, -24.15602025860895807, 10.28564288303536678 ) ) ;
#94058 = CARTESIAN_POINT ( 'NONE',  ( -12.90690225449951001, 15.05119527412115055, -1.500000000000002220 ) ) ;
#94059 = ORIENTED_EDGE ( 'NONE', *, *, #28413, .T. ) ;
#94060 = CARTESIAN_POINT ( 'NONE',  ( -56.50842078106121136, -23.96119346886880663, -0.6495511937832126881 ) ) ;
#94061 = CARTESIAN_POINT ( 'NONE',  ( -123.5562042904833930, -23.47596703998600631, 11.44779298504227683 ) ) ;
#94062 = FACE_OUTER_BOUND ( 'NONE', #40699, .T. ) ;
#94063 = CARTESIAN_POINT ( 'NONE',  ( -6.500255983836059848, -19.66680810221124887, 11.49999999999999645 ) ) ;
#94064 = DIRECTION ( 'NONE',  ( -3.773278334453080206E-23, 0.9999999999976377785, 2.173523156925979975E-06 ) ) ;
#94065 = AXIS2_PLACEMENT_3D ( 'NONE', #24486, #49352, #33108 ) ;
#94066 = PRODUCT_DEFINITION ( 'UNKNOWN', '', #91188, #5341 ) ;
#94067 = CARTESIAN_POINT ( 'NONE',  ( -40.58953762381673158, -24.99132157543083466, 2.256160258750496084 ) ) ;
#94068 = CARTESIAN_POINT ( 'NONE',  ( 21.73672277138745201, -6.736064506363727666, 11.49999999999999645 ) ) ;
#94069 = ORIENTED_EDGE ( 'NONE', *, *, #14342, .T. ) ;
#94070 = CARTESIAN_POINT ( 'NONE',  ( -69.65141362638318867, -23.48783264082476308, -1.443836473390097908 ) ) ;
#94071 = CARTESIAN_POINT ( 'NONE',  ( -100.5228709571500616, -29.50248789122583659, 2.256150453626215580 ) ) ;
#94072 = EDGE_LOOP ( 'NONE', ( #2333, #90632, #11115, #22584 ) ) ;
#94073 = B_SPLINE_CURVE_WITH_KNOTS ( 'NONE', 3,
 ( #87126, #17618, #48590, #79513, #64325, #95242 ),
 .UNSPECIFIED., .F., .F.,
 ( 4, 2, 4 ),
 ( 1.570887131794638196E-05, 0.001396322306279761073, 0.002776935741241575838 ),
 .UNSPECIFIED. ) ;
#94074 = CARTESIAN_POINT ( 'NONE',  ( 4.066846734877469949, -19.79409818376439389, 11.49999999999998934 ) ) ;
#94075 = CARTESIAN_POINT ( 'NONE',  ( -50.62287095715005592, -29.50250786944525672, 11.44777988621624054 ) ) ;
#94076 = CARTESIAN_POINT ( 'NONE',  ( -53.52287095715006870, -29.50248528299804818, 1.056150453629033370 ) ) ;
#94077 = ORIENTED_EDGE ( 'NONE', *, *, #44090, .F. ) ;
#94078 = CARTESIAN_POINT ( 'NONE',  ( -0.1447610318486398373, -21.17595468364151046, -1.479945482512687427 ) ) ;
#94079 = CARTESIAN_POINT ( 'NONE',  ( -17.45619364963476627, 14.87644265977633573, 11.49999999999998934 ) ) ;
#94080 = CARTESIAN_POINT ( 'NONE',  ( -40.53036611195729222, -25.12111198278256552, 2.835794650103506509 ) ) ;
#94081 = VECTOR ( 'NONE', #7408, 1000.000000000000000 ) ;
#94082 = CARTESIAN_POINT ( 'NONE',  ( -18.86779840422491716, -6.689013621249945807, -1.500000000000002220 ) ) ;
#94083 = CARTESIAN_POINT ( 'NONE',  ( -104.6228709571500985, -23.96127896941632685, -0.6493128931037839280 ) ) ;
#94084 = CARTESIAN_POINT ( 'NONE',  ( -12.59924929152775874, 16.77720732749412846, 11.49999999999999645 ) ) ;
#94085 = VECTOR ( 'NONE', #7489, 1000.000000000000114 ) ;
#94086 = CARTESIAN_POINT ( 'NONE',  ( -4.312370003044874167, -5.876774720514409189, 19.42522865122897358 ) ) ;
#94087 = CARTESIAN_POINT ( 'NONE',  ( -124.5545015191503637, -24.51314013834317151, 0.6176544820404232805 ) ) ;
#94088 = CARTESIAN_POINT ( 'NONE',  ( -20.57682416348112397, 7.868404785394932155, 11.49999999999998934 ) ) ;
#94089 = FACE_OUTER_BOUND ( 'NONE', #88801, .T. ) ;
#94090 = ORIENTED_EDGE ( 'NONE', *, *, #38663, .F. ) ;
#94091 = PLANE ( 'NONE',  #71758 ) ;
#94092 = CARTESIAN_POINT ( 'NONE',  ( 9.402885806365684829, 5.965225279485572685, 29.04108526060719342 ) ) ;
#94093 = ORIENTED_EDGE ( 'NONE', *, *, #6485, .T. ) ;
#94094 = PLANE ( 'NONE',  #64799 ) ;
#94095 = ORIENTED_EDGE ( 'NONE', *, *, #49391, .T. ) ;
#94096 = ORIENTED_EDGE ( 'NONE', *, *, #43165, .F. ) ;
#94097 = EDGE_CURVE ( 'NONE', #48435, #18484, #90813, .T. ) ;
#94098 = CARTESIAN_POINT ( 'NONE',  ( -118.5895376238167387, -24.66019654487200086, 8.947790411086119278 ) ) ;
#94099 = DIRECTION ( 'NONE',  ( 1.000000000000000000, -0.000000000000000000, 2.417950247244706201E-16 ) ) ;
#94100 = CARTESIAN_POINT ( 'NONE',  ( -36.62372823607387318, -24.65952944569304606, 1.056160979905696129 ) ) ;
#94101 = CARTESIAN_POINT ( 'NONE',  ( 16.50020720150075348, -12.08490501797973238, -1.500000000000002220 ) ) ;
#94102 = ORIENTED_EDGE ( 'NONE', *, *, #54881, .F. ) ;
#94103 = DIRECTION ( 'NONE',  ( -0.000000000000000000, 1.000000000000000000, -0.000000000000000000 ) ) ;
#94104 = CARTESIAN_POINT ( 'NONE',  ( -44.61592860413497874, -23.48783264082476663, -1.443836473390094799 ) ) ;
#94105 = FACE_OUTER_BOUND ( 'NONE', #12676, .T. ) ;
#94106 = CARTESIAN_POINT ( 'NONE',  ( -19.83904684311861644, 10.14288308415042827, 11.49999999999998934 ) ) ;
#94107 = CARTESIAN_POINT ( 'NONE',  ( -38.62287095715005592, -29.50247984919015209, -1.443849546365060466 ) ) ;
#94108 = CARTESIAN_POINT ( 'NONE',  ( -28.98875734969026396, -0.3587747205144265483, 2.362022800118626531 ) ) ;
#94109 = VERTEX_POINT ( 'NONE', #97427 ) ;
#94110 = B_SPLINE_CURVE_WITH_KNOTS ( 'NONE', 3,
 ( #71003, #85718, #24807, #55283 ),
 .UNSPECIFIED., .F., .F.,
 ( 4, 4 ),
 ( 0.000000000000000000, 1.000000000000000000 ),
 .UNSPECIFIED. ) ;
#94111 = CARTESIAN_POINT ( 'NONE',  ( -24.90875734969025501, -6.475225279485573360, 30.00402280011862288 ) ) ;
#94112 = CARTESIAN_POINT ( 'NONE',  ( -118.5228709571500616, -23.72747288104470442, -1.053458166803224572 ) ) ;
#94113 = EDGE_CURVE ( 'NONE', #17980, #22949, #21777, .T. ) ;
#94114 = CARTESIAN_POINT ( 'NONE',  ( -16.21995886604411297, 13.06735728859114509, 11.49999999999998934 ) ) ;
#94115 = EDGE_CURVE ( 'NONE', #37822, #53379, #27915, .T. ) ;
#94116 = ORIENTED_EDGE ( 'NONE', *, *, #7328, .F. ) ;
#94118 = ORIENTED_EDGE ( 'NONE', *, *, #43509, .F. ) ;
#94117 = CARTESIAN_POINT ( 'NONE',  ( -52.52287095715009713, -23.48783264083416356, -1.443836473375487151 ) ) ;
#94119 = ORIENTED_EDGE ( 'NONE', *, *, #95836, .T. ) ;
#94120 = CARTESIAN_POINT ( 'NONE',  ( -51.31235188911633571, -25.25854493898471276, 6.754155260380676040 ) ) ;
#94121 = CARTESIAN_POINT ( 'NONE',  ( -17.33045254171255678, -11.89390297951003816, -1.500000000000002220 ) ) ;
#94122 = VERTEX_POINT ( 'NONE', #75570 ) ;
#94123 = LINE ( 'NONE', #18007, #835 ) ;
#94124 = CARTESIAN_POINT ( 'NONE',  ( -65.05438548721848235, -6.376774720514426953, 29.49402280011861777 ) ) ;
#94125 = CARTESIAN_POINT ( 'NONE',  ( 5.325188327271017208, -5.356774720514426491, -25.45818409267644711 ) ) ;
#94126 = CARTESIAN_POINT ( 'NONE',  ( -86.64363164346322321, -23.48786465467240703, 11.44779295918254647 ) ) ;
#94127 = CARTESIAN_POINT ( 'NONE',  ( -110.1351499245318877, -25.12167980767599929, 2.838884635434631765 ) ) ;
#94128 = CYLINDRICAL_SURFACE ( 'NONE', #62700, 3.349999999999998757 ) ;
#94130 = ORIENTED_EDGE ( 'NONE', *, *, #5221, .F. ) ;
#94129 = CARTESIAN_POINT ( 'NONE',  ( -7.477829544921322125, 20.88912457518834742, 11.49999999999999645 ) ) ;
#94131 = EDGE_CURVE ( 'NONE', #77609, #6499, #93365, .T. ) ;
#94132 = DIRECTION ( 'NONE',  ( -3.773278334453079618E-23, 0.9999999999976377785, 2.173523156925979975E-06 ) ) ;
#94133 = CARTESIAN_POINT ( 'NONE',  ( -37.55620429048340014, -23.48786465467240347, 11.44779295918255180 ) ) ;
#94134 = ORIENTED_EDGE ( 'NONE', *, *, #91449, .F. ) ;
#94135 = CARTESIAN_POINT ( 'NONE',  ( -16.57510365746454184, 15.48777146884464884, 11.49999999999998934 ) ) ;
#94137 = VERTEX_POINT ( 'NONE', #43645 ) ;
#94136 = DIRECTION ( 'NONE',  ( 0.000000000000000000, 0.000000000000000000, -1.000000000000000000 ) ) ;
#94138 = ORIENTED_EDGE ( 'NONE', *, *, #24897, .T. ) ;
#94139 = DIRECTION ( 'NONE',  ( 0.000000000000000000, 0.000000000000000000, -1.000000000000000000 ) ) ;
#94140 = VECTOR ( 'NONE', #83929, 1000.000000000000114 ) ;
#94141 = CARTESIAN_POINT ( 'NONE',  ( 11.25103634530202790, -16.72154935384561725, -1.500000000000002220 ) ) ;
#94142 = LINE ( 'NONE', #24628, #81372 ) ;
#94143 = ORIENTED_EDGE ( 'NONE', *, *, #32273, .T. ) ;
#94144 = CARTESIAN_POINT ( 'NONE',  ( 15.38791554121732119, -3.579805417253313138, -28.27843079449244357 ) ) ;
#94145 = CARTESIAN_POINT ( 'NONE',  ( -21.98280116189361877, -4.439423430357301470, -1.500000000000002220 ) ) ;
#94146 = EDGE_CURVE ( 'NONE', #39688, #53441, #43766, .T. ) ;
#94147 = ORIENTED_EDGE ( 'NONE', *, *, #30454, .F. ) ;
#94148 = VERTEX_POINT ( 'NONE', #52258 ) ;
#94149 = CARTESIAN_POINT ( 'NONE',  ( -112.5880276694465181, -24.51419770103158413, 9.386484678747166299 ) ) ;
#94150 = CARTESIAN_POINT ( 'NONE',  ( -94.59406235252116346, -23.96169478059713143, 10.65365249895717881 ) ) ;
#94151 = DIRECTION ( 'NONE',  ( -3.773278334453080206E-23, 0.9999999999976377785, 2.173523156925979975E-06 ) ) ;
#94152 = CARTESIAN_POINT ( 'NONE',  ( 3.180076745125953508, 0.3587747205143968499, -28.87659520466658236 ) ) ;
#94153 = CARTESIAN_POINT ( 'NONE',  ( 12.40597316965629560, 5.152774720514427642, -26.28458722401733993 ) ) ;
#94154 = EDGE_CURVE ( 'NONE', #19978, #93020, #49896, .T. ) ;
#94155 = VECTOR ( 'NONE', #57628, 1000.000000000000114 ) ;
#94156 = CARTESIAN_POINT ( 'NONE',  ( 6.425176733589397671, 18.50107501292125178, 11.49999999999998934 ) ) ;
#94157 = FACE_OUTER_BOUND ( 'NONE', #33356, .T. ) ;
#94158 = ORIENTED_EDGE ( 'NONE', *, *, #68571, .F. ) ;
#94159 = CARTESIAN_POINT ( 'NONE',  ( 3.930203739357332360, 21.12693704021120666, 11.49999999999998934 ) ) ;
#94160 = CARTESIAN_POINT ( 'NONE',  ( -2.794871794871795156, -6.376774720514417183, 20.36318108974359475 ) ) ;
#94161 = CYLINDRICAL_SURFACE ( 'NONE', #91773, 1.000000000000000888 ) ;
#94162 = CARTESIAN_POINT ( 'NONE',  ( -65.05438548721848235, -6.376774720514426953, 0.7300228001186309656 ) ) ;
#94163 = CARTESIAN_POINT ( 'NONE',  ( -68.62287095715005592, -24.64965695001468404, 8.947790433994184056 ) ) ;
#94164 = CARTESIAN_POINT ( 'NONE',  ( 22.85142058292489153, -2.183311388647848350, -1.500000000000002220 ) ) ;
#94165 = EDGE_CURVE ( 'NONE', #73557, #29958, #18425, .T. ) ;
#94166 = ADVANCED_FACE ( 'NONE', ( #59879 ), #30907, .F. ) ;
#94167 = APPROVAL_DATE_TIME ( #30267, #32096 ) ;
#94168 = CARTESIAN_POINT ( 'NONE',  ( -96.63574071546304367, -23.73791477778911840, 11.05961554403170410 ) ) ;
#94169 = FACE_OUTER_BOUND ( 'NONE', #77879, .T. ) ;
#94170 = CARTESIAN_POINT ( 'NONE',  ( -4.446071851354966853, 19.53225066162704948, 11.49999999999999645 ) ) ;
#94171 = CARTESIAN_POINT ( 'NONE',  ( 12.40597316965629560, -5.152774720514427642, -26.28458722401733993 ) ) ;
#94172 = DIRECTION ( 'NONE',  ( 0.000000000000000000, 0.000000000000000000, 1.000000000000000000 ) ) ;
#94173 = CARTESIAN_POINT ( 'NONE',  ( 4.948119756536996761, -5.876774720514410077, 19.52858994054604125 ) ) ;
#94174 = CARTESIAN_POINT ( 'NONE',  ( 32.06540688909005610, -6.475225279485576024, -12.44045471929206137 ) ) ;
#94175 = CARTESIAN_POINT ( 'NONE',  ( -46.62287095715004881, -24.64898659630528499, 1.056161002820821038 ) ) ;
#94176 = CARTESIAN_POINT ( 'NONE',  ( 1.937016913031804455, -21.67664703184077268, -1.500000000000002220 ) ) ;
#94177 = LINE ( 'NONE', #78949, #31814 ) ;
#94178 = CARTESIAN_POINT ( 'NONE',  ( 6.560884470684795744, 18.50665934316380756, -1.500000000000002220 ) ) ;
#94179 = DIRECTION ( 'NONE',  ( 0.000000000000000000, 2.173523156925980399E-06, -0.9999999999976378895 ) ) ;
#94180 = CARTESIAN_POINT ( 'NONE',  ( -109.8661607933284472, -25.31698164407086793, 5.216081326368730231 ) ) ;
#94181 = PERSON_AND_ORGANIZATION ( #18663, #65372 ) ;
#94182 = DIRECTION ( 'NONE',  ( 1.000000000000000000, -0.000000000000000000, -0.000000000000000000 ) ) ;
#94183 = CYLINDRICAL_SURFACE ( 'NONE', #99347, 2.500000000000000444 ) ;
#94184 = CARTESIAN_POINT ( 'NONE',  ( -14.32454646668868747, 14.77526322620295929, 11.49999999999999645 ) ) ;
#94185 = CARTESIAN_POINT ( 'NONE',  ( -27.15721599100127648, -0.3587747205144061757, -10.22292133548836723 ) ) ;
#94186 = CARTESIAN_POINT ( 'NONE',  ( -120.5534794319312653, -24.63355581998386157, 0.9682620441943888823 ) ) ;
#94187 = EDGE_CURVE ( 'NONE', #73037, #88312, #30406, .T. ) ;
#94188 = CARTESIAN_POINT ( 'NONE',  ( -22.51868310087907687, -2.221351303042197411, 11.49999999999999645 ) ) ;
#94189 = VERTEX_POINT ( 'NONE', #7071 ) ;
#94190 = CARTESIAN_POINT ( 'NONE',  ( -70.29041810236439858, -25.25639601273440249, 7.100646424425399061 ) ) ;
#94191 = CARTESIAN_POINT ( 'NONE',  ( -26.38925086361725647, -24.87739167191250544, 6.668544504290081498 ) ) ;
#94192 = FACE_OUTER_BOUND ( 'NONE', #49832, .T. ) ;
#94193 = PLANE ( 'NONE',  #40221 ) ;
#94194 = EDGE_CURVE ( 'NONE', #13356, #26478, #36563, .T. ) ;
#94195 = CARTESIAN_POINT ( 'NONE',  ( -25.56960729154874556, -24.61459572358360859, 5.760628103071427475 ) ) ;
#94196 = CARTESIAN_POINT ( 'NONE',  ( -28.52287095715007581, -23.79900956871740547, 10.65359469479120058 ) ) ;
#94197 = EDGE_CURVE ( 'NONE', #60950, #93421, #63388, .T. ) ;
#94198 = EDGE_CURVE ( 'NONE', #37020, #69912, #23791, .T. ) ;
#94199 = ORIENTED_EDGE ( 'NONE', *, *, #80476, .T. ) ;
#94200 = CARTESIAN_POINT ( 'NONE',  ( -80.09072421954219578, -25.31596230203514608, 5.004106418144936619 ) ) ;
#94201 = CARTESIAN_POINT ( 'NONE',  ( 22.28265747778879202, 5.072132558558076099, -1.500000000000002220 ) ) ;
#94202 = FACE_OUTER_BOUND ( 'NONE', #57537, .T. ) ;
#94203 = CARTESIAN_POINT ( 'NONE',  ( 282.9764569301858046, -6.376774720514426953, 20.79159422840526616 ) ) ;
#94204 = CARTESIAN_POINT ( 'NONE',  ( -63.54360795143862362, -24.35071581493543036, 9.817618358456027039 ) ) ;
#94205 = CARTESIAN_POINT ( 'NONE',  ( -1.726696889551340153, 22.42386595106472669, 11.49999999999999645 ) ) ;
#94206 = ORIENTED_EDGE ( 'NONE', *, *, #71885, .F. ) ;
#94207 = CARTESIAN_POINT ( 'NONE',  ( -34.62287095715005592, -24.33927499327853639, 9.819080762295829601 ) ) ;
#94208 = B_SPLINE_CURVE_WITH_KNOTS ( 'NONE', 3,
 ( #56300, #87221, #10099, #1999 ),
 .UNSPECIFIED., .F., .F.,
 ( 4, 4 ),
 ( 0.000000000000000000, 9.999999999996123101E-05 ),
 .UNSPECIFIED. ) ;
#94209 = AXIS2_PLACEMENT_3D ( 'NONE', #38267, #68732, #99163 ) ;
#94210 = CARTESIAN_POINT ( 'NONE',  ( -13.81295463269534096, 17.03802364079049525, -1.500000000000002220 ) ) ;
#94211 = CARTESIAN_POINT ( 'NONE',  ( 32.76434349455507089, 3.489637856041424957, -3.883594654058048157 ) ) ;
#94212 = B_SPLINE_CURVE_WITH_KNOTS ( 'NONE', 3,
 ( #40074, #6728, #72033, #79123 ),
 .UNSPECIFIED., .F., .F.,
 ( 4, 4 ),
 ( 1.387778780781445676E-17, 0.0001000000000000167422 ),
 .UNSPECIFIED. ) ;
#94213 = CARTESIAN_POINT ( 'NONE',  ( -44.49964348827519700, -24.15620529776628089, 10.23563542870660470 ) ) ;
#94214 = CARTESIAN_POINT ( 'NONE',  ( -99.52287095715006160, -29.50248528299804818, 1.056150453629042030 ) ) ;
#94215 = VERTEX_POINT ( 'NONE', #70985 ) ;
#94216 = CARTESIAN_POINT ( 'NONE',  ( -112.5895376238167387, -23.48786465467241769, 11.44779295918254114 ) ) ;
#94217 = DIRECTION ( 'NONE',  ( -0.000000000000000000, -0.000000000000000000, -1.000000000000000000 ) ) ;
#94218 = VERTEX_POINT ( 'NONE', #78565 ) ;
#94219 = CARTESIAN_POINT ( 'NONE',  ( 1.259202695315177589, 20.44674571593545664, -1.500000000000002220 ) ) ;
#94220 = ORIENTED_EDGE ( 'NONE', *, *, #31399, .F. ) ;
#94221 = VERTEX_POINT ( 'NONE', #70479 ) ;
#94222 = VERTEX_POINT ( 'NONE', #62369 ) ;
#94223 = VERTEX_POINT ( 'NONE', #38020 ) ;
#94224 = ADVANCED_FACE ( 'NONE', ( #84690 ), #55769, .F. ) ;
#94225 = CARTESIAN_POINT ( 'NONE',  ( 22.94779996701378266, 2.684060219229261968, -1.500000000000002220 ) ) ;
#94226 = CARTESIAN_POINT ( 'NONE',  ( -112.5228709571500758, -24.51387760970726148, 9.387446482453407626 ) ) ;
#94227 = CARTESIAN_POINT ( 'NONE',  ( -19.77321833943668850, 4.698914572609424134, -1.500000000000002220 ) ) ;
#94228 = ORIENTED_EDGE ( 'NONE', *, *, #68739, .T. ) ;
#94229 = CARTESIAN_POINT ( 'NONE',  ( -85.62287095715004170, -29.50249982740957577, 7.747779886224967605 ) ) ;
#94230 = CARTESIAN_POINT ( 'NONE',  ( 282.9764569301858046, -5.965225279485572685, 20.79159422840526616 ) ) ;
#94231 = B_SPLINE_CURVE_WITH_KNOTS ( 'NONE', 3,
 ( #99899, #45644, #98915, #82696, #99414, #29909 ),
 .UNSPECIFIED., .F., .F.,
 ( 4, 2, 4 ),
 ( 0.000000000000000000, 0.001380901958385394833, 0.002761803916770789666 ),
 .UNSPECIFIED. ) ;
#94233 = CARTESIAN_POINT ( 'NONE',  ( -44.55620429048339304, -24.66019654487199020, 8.947790411086137041 ) ) ;
#94232 = VECTOR ( 'NONE', #25808, 1000.000000000000000 ) ;
#94234 = CARTESIAN_POINT ( 'NONE',  ( 4.413617546364139166, -5.876774720514407413, 18.86076033669171181 ) ) ;
#94236 = ORIENTED_EDGE ( 'NONE', *, *, #77590, .F. ) ;
#94235 = CARTESIAN_POINT ( 'NONE',  ( 11.78165356204951131, -17.99452314462042324, 11.49999999999999645 ) ) ;
#94237 = CARTESIAN_POINT ( 'NONE',  ( -75.51431064661339576, -23.85016227208580730, -0.8807180028928284221 ) ) ;
#94238 = CARTESIAN_POINT ( 'NONE',  ( -104.6228709571500559, -24.64898659630529210, 1.056161002820829697 ) ) ;
#94239 = CC_DESIGN_SECURITY_CLASSIFICATION ( #48909, ( #47237 ) ) ;
#94240 = ORIENTED_EDGE ( 'NONE', *, *, #10773, .F. ) ;
#94241 = CARTESIAN_POINT ( 'NONE',  ( 16.28047541435887879, -12.87082401369967677, -1.500000000000002220 ) ) ;
#94242 = EDGE_CURVE ( 'NONE', #12228, #7941, #58865, .T. ) ;
#94243 = ORIENTED_EDGE ( 'NONE', *, *, #79079, .T. ) ;
#94245 = ORIENTED_EDGE ( 'NONE', *, *, #6926, .T. ) ;
#94244 = CARTESIAN_POINT ( 'NONE',  ( -125.6264014075705546, -23.48783264082478794, -1.443836473390061936 ) ) ;
#94246 = EDGE_CURVE ( 'NONE', #62582, #45335, #72893, .T. ) ;
#94247 = CARTESIAN_POINT ( 'NONE',  ( -111.6303196403976727, -23.73791477778912551, 11.05961554403170055 ) ) ;
#94248 = DIRECTION ( 'NONE',  ( -1.000000000000000000, 0.000000000000000000, 0.000000000000000000 ) ) ;
#94249 = VERTEX_POINT ( 'NONE', #61874 ) ;
#94250 = EDGE_LOOP ( 'NONE', ( #42669, #63410, #93466, #3892 ) ) ;
#94251 = CARTESIAN_POINT ( 'NONE',  ( -6.636054160061366503, -5.876774720514411854, 19.15289935703627933 ) ) ;
#94252 = CARTESIAN_POINT ( 'NONE',  ( -42.64093939733596272, -24.15620529776628089, 10.23563542870661358 ) ) ;
#94253 = CARTESIAN_POINT ( 'NONE',  ( -43.53437882689529204, -24.51419770103157347, 9.386484678747182286 ) ) ;
#94254 = CARTESIAN_POINT ( 'NONE',  ( 4.628415685485613551, -21.52068878818806752, 11.49999999999999645 ) ) ;
#94255 = EDGE_CURVE ( 'NONE', #14282, #12529, #15682, .T. ) ;
#94256 = DIRECTION ( 'NONE',  ( 0.000000000000000000, -1.000000000000000000, 0.000000000000000000 ) ) ;
#94257 = CARTESIAN_POINT ( 'NONE',  ( -8.190886813464794969, 21.05079722441571732, -1.500000000000002220 ) ) ;
#94258 = CARTESIAN_POINT ( 'NONE',  ( 20.92198360912786015, -1.804805560479522342, 11.49999999999998934 ) ) ;
#94259 = EDGE_CURVE ( 'NONE', #29559, #80701, #8724, .T. ) ;
#94261 = ORIENTED_EDGE ( 'NONE', *, *, #51520, .F. ) ;
#94260 = CARTESIAN_POINT ( 'NONE',  ( -62.52287095715006160, -24.33832256527049154, 0.1851278514138569864 ) ) ;
#94262 = ORIENTED_EDGE ( 'NONE', *, *, #92157, .T. ) ;
#94263 = CARTESIAN_POINT ( 'NONE',  ( -69.55126625704997423, -29.50248967467915051, 3.076686136236004732 ) ) ;
#94264 = VECTOR ( 'NONE', #9659, 1000.000000000000000 ) ;
#94265 = DIRECTION ( 'NONE',  ( -0.9997753877537054468, 0.000000000000000000, 0.02119372647572819943 ) ) ;
#94266 = ORIENTED_EDGE ( 'NONE', *, *, #36138, .F. ) ;
#94267 = CARTESIAN_POINT ( 'NONE',  ( 21.14167878903947084, -0.5806874866175276706, 11.49999999999998934 ) ) ;
#94268 = CARTESIAN_POINT ( 'NONE',  ( 19.75748517575715368, -5.965225279485572685, 28.87153971905864580 ) ) ;
#94269 = CARTESIAN_POINT ( 'NONE',  ( -51.92774333234893192, -25.03148468052863862, 6.302625650274440439 ) ) ;
#94270 = CARTESIAN_POINT ( 'NONE',  ( -2.499999999999993339, 19.99999999999999645, 0.000000000000000000 ) ) ;
#94271 = CARTESIAN_POINT ( 'NONE',  ( -29.49875734969025842, 0.3587747205144262708, 23.37402280011862743 ) ) ;
#94273 = B_SPLINE_CURVE_WITH_KNOTS ( 'NONE', 3,
 ( #44814, #83857, #75733, #7224 ),
 .UNSPECIFIED., .F., .F.,
 ( 4, 4 ),
 ( 0.000000000000000000, 9.999999999998897304E-05 ),
 .UNSPECIFIED. ) ;
#94272 = CARTESIAN_POINT ( 'NONE',  ( -29.49875734969025842, -0.3587747205144262708, 23.37402280011862743 ) ) ;
#94274 = CARTESIAN_POINT ( 'NONE',  ( 21.27325221474336914, 6.521069146585026566, -1.500000000000002220 ) ) ;
#94275 = CARTESIAN_POINT ( 'NONE',  ( -29.81175120719462157, -25.24633111994858581, 4.942810988825437235 ) ) ;
#94276 = ORIENTED_EDGE ( 'NONE', *, *, #63090, .F. ) ;
#94277 = LINE ( 'NONE', #48630, #44931 ) ;
#94278 = CARTESIAN_POINT ( 'NONE',  ( -86.52287095715006160, -23.48786465467241058, 11.44779295918254292 ) ) ;
#94279 = CARTESIAN_POINT ( 'NONE',  ( -126.5896050762271869, -24.34968618360934300, 0.1864209137778884418 ) ) ;
#94280 = DIRECTION ( 'NONE',  ( 0.000000000000000000, 0.000000000000000000, 1.000000000000000000 ) ) ;
#94281 = CARTESIAN_POINT ( 'NONE',  ( -66.62287095715005592, -23.48786465467241058, 11.44779295918254647 ) ) ;
#94282 = ADVANCED_FACE ( 'NONE', ( #62889 ), #85029, .T. ) ;
#94283 = CARTESIAN_POINT ( 'NONE',  ( 19.46547125265945155, -1.073068822128883104, 11.49999999999998934 ) ) ;
#94284 = CARTESIAN_POINT ( 'NONE',  ( -19.04320821261859464, -9.809917703373946196, -1.500000000000002220 ) ) ;
#94285 = FACE_OUTER_BOUND ( 'NONE', #58547, .T. ) ;
#94286 = CARTESIAN_POINT ( 'NONE',  ( -60.59238776529559090, -24.40133493613623372, 9.663955038888268234 ) ) ;
#94287 = CARTESIAN_POINT ( 'NONE',  ( -100.6228709571500559, -23.48786465467241769, 11.44779295918254114 ) ) ;
#94288 = PLANE ( 'NONE',  #50649 ) ;
#94289 = CARTESIAN_POINT ( 'NONE',  ( -20.37646751746074969, -10.17465561509698979, -1.500000000000002220 ) ) ;
#94290 = CARTESIAN_POINT ( 'NONE',  ( -0.02075734969026423599, 6.475225279485573360, -0.08597719988137648983 ) ) ;
#94291 = CARTESIAN_POINT ( 'NONE',  ( 14.85834502026402681, 2.682774720514426559, -27.37203305628894867 ) ) ;
#94292 = CARTESIAN_POINT ( 'NONE',  ( 12.34629653512297409, 15.52844579862587437, 11.49999999999999645 ) ) ;
#94293 = CARTESIAN_POINT ( 'NONE',  ( 5.443272695963705665, -6.376774720514417183, 20.27301970143225418 ) ) ;
#94294 = CARTESIAN_POINT ( 'NONE',  ( 9.071512145086499501, 0.000000000000000000, 3.687490859131163923 ) ) ;
#94295 = CARTESIAN_POINT ( 'NONE',  ( -64.62287095715005592, -23.47593901973091235, -1.443836447539007972 ) ) ;
#94296 = EDGE_LOOP ( 'NONE', ( #16968, #28613, #16684, #26994 ) ) ;
#94297 = CARTESIAN_POINT ( 'NONE',  ( -49.34187094658451400, -25.21537169916210885, 6.482075674763354556 ) ) ;
#94298 = CARTESIAN_POINT ( 'NONE',  ( -5.988734693054777125, -5.876774720514415407, 19.95737465391042065 ) ) ;
#94300 = CARTESIAN_POINT ( 'NONE',  ( -51.52876458270549165, -25.10935885016122882, 3.420678843004004488 ) ) ;
#94299 = CC_DESIGN_APPROVAL ( #19617, ( #37589 ) ) ;
#94301 = CARTESIAN_POINT ( 'NONE',  ( 2.849777056880220982, 21.50153301832798647, 11.49999999999998934 ) ) ;
#94302 = CARTESIAN_POINT ( 'NONE',  ( -53.01255352321339842, 2.682774720514426559, 35.59556822165056644 ) ) ;
#94303 = CARTESIAN_POINT ( 'NONE',  ( 6.966380261627926451, -18.21767524041069564, -1.500000000000002220 ) ) ;
#94304 = CARTESIAN_POINT ( 'NONE',  ( -55.63443494932560895, -24.63419186844611275, 9.035850630976927533 ) ) ;
#94305 = AXIS2_PLACEMENT_3D ( 'NONE', #67343, #83037, #3572 ) ;
#94306 = B_SPLINE_CURVE_WITH_KNOTS ( 'NONE', 3,
 ( #92433, #68611, #90941, #46269 ),
 .UNSPECIFIED., .F., .F.,
 ( 4, 4 ),
 ( 0.000000000000000000, 9.999999999996123101E-05 ),
 .UNSPECIFIED. ) ;
#94307 = ORIENTED_EDGE ( 'NONE', *, *, #19850, .T. ) ;
#94308 = LOCAL_TIME ( 0, 54, 15.00000000000000000, #20050 ) ;
#94309 = CARTESIAN_POINT ( 'NONE',  ( 15.56926775127050000, -13.18612581554039132, 11.49999999999999645 ) ) ;
#94310 = CARTESIAN_POINT ( 'NONE',  ( -85.52287095715009002, -23.47593901973090524, -1.443836447538996648 ) ) ;
#94311 = DIRECTION ( 'NONE',  ( -0.000000000000000000, 1.000000000000000000, -0.000000000000000000 ) ) ;
#94312 = EDGE_CURVE ( 'NONE', #8482, #80639, #3886, .T. ) ;
#94313 = EDGE_LOOP ( 'NONE', ( #31463, #55961, #30067, #19093 ) ) ;
#94314 = CARTESIAN_POINT ( 'NONE',  ( -30.60993385648455956, -24.45056191361606679, 9.787827635114012992 ) ) ;
#94315 = CARTESIAN_POINT ( 'NONE',  ( 33.13630134430571417, 3.554473796596999691, -12.85738972836020899 ) ) ;
#94316 = CARTESIAN_POINT ( 'NONE',  ( 7.141559373243376641, -6.376774720514415407, 19.83742167145384983 ) ) ;
#94317 = CARTESIAN_POINT ( 'NONE',  ( -29.49875734969026198, -5.965225279485572685, 2.362022800118626531 ) ) ;
#94318 = CARTESIAN_POINT ( 'NONE',  ( -86.52287095715006160, -23.48783264083431277, -1.443836473375255336 ) ) ;
#94319 = CARTESIAN_POINT ( 'NONE',  ( 13.72940079880349984, -14.68433028913016791, -1.500000000000002220 ) ) ;
#94320 = CYLINDRICAL_SURFACE ( 'NONE', #22448, 1.700000000000008837 ) ;
#94321 = ORIENTED_EDGE ( 'NONE', *, *, #97082, .F. ) ;
#94322 = EDGE_CURVE ( 'NONE', #75118, #13466, #81325, .T. ) ;
#94323 = CARTESIAN_POINT ( 'NONE',  ( -48.62287095715004881, -29.50247984919015209, -1.443849546365058689 ) ) ;
#94324 = EDGE_CURVE ( 'NONE', #4924, #55530, #40172, .T. ) ;
#94325 = EDGE_CURVE ( 'NONE', #9990, #1598, #75198, .T. ) ;
#94326 = CARTESIAN_POINT ( 'NONE',  ( 22.74528686061176685, 3.085755641335488964, 11.49999999999999645 ) ) ;
#94327 = CARTESIAN_POINT ( 'NONE',  ( 2.440706796964721370, 22.61111150098722788, -1.500000000000002220 ) ) ;
#94328 = ORIENTED_EDGE ( 'NONE', *, *, #43625, .T. ) ;
#94329 = CARTESIAN_POINT ( 'NONE',  ( -31.62287095715005236, -23.47596703998600276, 11.44779298504227505 ) ) ;
#94330 = CARTESIAN_POINT ( 'NONE',  ( -75.62287095715005592, -23.48786465467241058, 11.44779295918254647 ) ) ;
#94331 = CARTESIAN_POINT ( 'NONE',  ( -97.92287095715006728, -23.47593901973090524, -1.443836447538996870 ) ) ;
#94332 = ADVANCED_FACE ( 'NONE', ( #2472 ), #48661, .F. ) ;
#94333 = CARTESIAN_POINT ( 'NONE',  ( -30.57287095715008007, -25.27567627223822555, 6.132950404913888320 ) ) ;
#94334 = PLANE ( 'NONE',  #85129 ) ;
#94335 = VECTOR ( 'NONE', #9913, 1000.000000000000000 ) ;
#94336 = PLANE ( 'NONE',  #84919 ) ;
#94337 = CARTESIAN_POINT ( 'NONE',  ( -90.62287095715004170, -23.48783264082478794, -1.443836473390063713 ) ) ;
#94338 = LINE ( 'NONE', #87227, #64739 ) ;
#94339 = VERTEX_POINT ( 'NONE', #72987 ) ;
#94340 = CARTESIAN_POINT ( 'NONE',  ( 15.56926775127050000, -13.18612581554039132, 11.49999999999998934 ) ) ;
#94341 = ORIENTED_EDGE ( 'NONE', *, *, #90655, .F. ) ;
#94342 = ADVANCED_FACE ( 'NONE', ( #33405 ), #94806, .T. ) ;
#94343 = CARTESIAN_POINT ( 'NONE',  ( -19.06187107478486098, -12.82570580458313003, -1.500000000000002220 ) ) ;
#94344 = CARTESIAN_POINT ( 'NONE',  ( -29.49875734969026198, -5.965225279485572685, 7.870022800118625206 ) ) ;
#94345 = ORIENTED_EDGE ( 'NONE', *, *, #58807, .T. ) ;
#94346 = B_SPLINE_CURVE_WITH_KNOTS ( 'NONE', 3,
 ( #94839, #41065, #72023, #8612 ),
 .UNSPECIFIED., .F., .F.,
 ( 4, 4 ),
 ( 0.08985008422344552270, 0.09885651549556107032 ),
 .UNSPECIFIED. ) ;
#94347 = FACE_OUTER_BOUND ( 'NONE', #52549, .T. ) ;
#94348 = CARTESIAN_POINT ( 'NONE',  ( 0.000000000000000000, 1.682774720514426114, -1.352392034746782823 ) ) ;
#94349 = ADVANCED_FACE ( 'NONE', ( #56772 ), #87703, .T. ) ;
#94350 = CARTESIAN_POINT ( 'NONE',  ( -117.7765765077247693, -25.21288392202306383, 6.500954737128433969 ) ) ;
#94352 = ORIENTED_EDGE ( 'NONE', *, *, #38589, .T. ) ;
#94351 = CARTESIAN_POINT ( 'NONE',  ( 20.49606604269246546, -5.804284187783010474, 11.49999999999999645 ) ) ;
#94353 = B_SPLINE_CURVE_WITH_KNOTS ( 'NONE', 3,
 ( #25187, #24188, #9970, #56164 ),
 .UNSPECIFIED., .F., .F.,
 ( 4, 4 ),
 ( 0.9494622744413409032, 0.9504630214821060408 ),
 .UNSPECIFIED. ) ;
#94354 = TOROIDAL_SURFACE ( 'NONE', #23058, 19.00000000000000000, 1.000000000000000000 ) ;
#94355 = ORIENTED_EDGE ( 'NONE', *, *, #83909, .F. ) ;
#94356 = CARTESIAN_POINT ( 'NONE',  ( -19.97062832128981213, -9.750827054148329509, 11.49999999999998934 ) ) ;
#94357 = VECTOR ( 'NONE', #10584, 1000.000000000000000 ) ;
#94358 = CARTESIAN_POINT ( 'NONE',  ( 3.034461355793923509, -20.43525710956717845, 11.49999999999998934 ) ) ;
#94359 = EDGE_CURVE ( 'NONE', #2589, #12603, #12061, .T. ) ;
#94360 = ORIENTED_EDGE ( 'NONE', *, *, #48063, .F. ) ;
#94361 = CARTESIAN_POINT ( 'NONE',  ( 0.3085469314987323020, -6.376774720514413630, 19.52341893546493523 ) ) ;
#94362 = CARTESIAN_POINT ( 'NONE',  ( -95.59855507052287749, -23.85049219812686161, 10.88485053497527133 ) ) ;
#94363 = EDGE_LOOP ( 'NONE', ( #76767, #53317, #47611, #60177, #58023, #2306 ) ) ;
#94364 = CARTESIAN_POINT ( 'NONE',  ( -65.58953762381671027, -25.00158670708909625, 2.256160236439167299 ) ) ;
#94365 = EDGE_LOOP ( 'NONE', ( #33606, #14711, #89393, #22120 ) ) ;
#94366 = CARTESIAN_POINT ( 'NONE',  ( -129.5562042904833788, -24.65952944569305316, 1.056160979905707009 ) ) ;
#94367 = CARTESIAN_POINT ( 'NONE',  ( -55.52287095715006870, -23.48786465467241058, 11.44779295918254824 ) ) ;
#94368 = CARTESIAN_POINT ( 'NONE',  ( 18.75483278694074940, -9.228467059531109129, -1.500000000000002220 ) ) ;
#94369 = CARTESIAN_POINT ( 'NONE',  ( -17.40403014803320758, -13.24600170205644289, 11.49999999999999645 ) ) ;
#94370 = EDGE_CURVE ( 'NONE', #37559, #60977, #93344, .T. ) ;
#94371 = CARTESIAN_POINT ( 'NONE',  ( -52.62287095715005592, -24.50216790748100593, 0.6166512839513587085 ) ) ;
#94372 = LINE ( 'NONE', #26368, #48341 ) ;
#94373 = CARTESIAN_POINT ( 'NONE',  ( 19.77564376705174709, 10.73071584254150856, -1.500000000000002220 ) ) ;
#94374 = ADVANCED_FACE ( 'NONE', ( #13553 ), #98285, .F. ) ;
#94375 = CARTESIAN_POINT ( 'NONE',  ( -118.5902638581781048, -24.15620529776628800, 10.23563542870659582 ) ) ;
#94376 = FACE_OUTER_BOUND ( 'NONE', #13900, .T. ) ;
#94377 = AXIS2_PLACEMENT_3D ( 'NONE', #81317, #11798, #18419 ) ;
#94378 = CARTESIAN_POINT ( 'NONE',  ( -54.52287095715006870, -24.65952944569304606, 1.056160979905693686 ) ) ;
#94379 = ORIENTED_EDGE ( 'NONE', *, *, #35008, .T. ) ;
#94380 = CC_DESIGN_APPROVAL ( #64905, ( #44192 ) ) ;
#94381 = ORIENTED_EDGE ( 'NONE', *, *, #5787, .T. ) ;
#94382 = ORIENTED_EDGE ( 'NONE', *, *, #72637, .T. ) ;
#94383 = CARTESIAN_POINT ( 'NONE',  ( -99.78066557477396259, -25.26221283775623050, 6.943018465985777432 ) ) ;
#94384 = ORIENTED_EDGE ( 'NONE', *, *, #67075, .T. ) ;
#94385 = CARTESIAN_POINT ( 'NONE',  ( -10.59417575825165159, 18.57464501519095279, -1.500000000000002220 ) ) ;
#94386 = VECTOR ( 'NONE', #75553, 1000.000000000000000 ) ;
#94387 = CARTESIAN_POINT ( 'NONE',  ( 22.31825301297700648, 1.237144038376295274, 11.49999999999999645 ) ) ;
#94388 = ORIENTED_EDGE ( 'NONE', *, *, #27874, .F. ) ;
#94389 = CARTESIAN_POINT ( 'NONE',  ( 31.55302460176084978, -5.360765615368469739, -3.312397695011010335 ) ) ;
#94390 = CARTESIAN_POINT ( 'NONE',  ( -8.945158345017247825, -19.07159632999312393, 11.49999999999998934 ) ) ;
#94391 = CARTESIAN_POINT ( 'NONE',  ( -30.41985448271246995, -24.82657567899210704, 8.370654131274083198 ) ) ;
#94392 = CARTESIAN_POINT ( 'NONE',  ( -10.29545327866581950, 17.06371652956568852, -1.500000000000002220 ) ) ;
#94393 = CARTESIAN_POINT ( 'NONE',  ( -50.48627917242625784, -24.63419186844610209, 9.035850630976920428 ) ) ;
#94394 = CARTESIAN_POINT ( 'NONE',  ( 2.976770017179964700, -6.376774720514420736, 20.68690469677381927 ) ) ;
#94395 = CARTESIAN_POINT ( 'NONE',  ( -3.902479932019291553, -21.71820464621639246, -1.500000000000002220 ) ) ;
#94396 = DIRECTION ( 'NONE',  ( 0.06474050504609950296, -0.8381167135261472501, -0.5416355246053439210 ) ) ;
#94397 = VECTOR ( 'NONE', #87030, 1000.000000000000227 ) ;
#94398 = ORIENTED_EDGE ( 'NONE', *, *, #82537, .T. ) ;
#94399 = CARTESIAN_POINT ( 'NONE',  ( -116.5926287344351806, -23.73766607897671577, -1.055555164236427590 ) ) ;
#94400 = CARTESIAN_POINT ( 'NONE',  ( -121.5228709571501184, -24.33832256527049154, 0.1851278514138670062 ) ) ;
#94401 = CARTESIAN_POINT ( 'NONE',  ( -20.33245250387252767, 4.503473919074798104, 11.49999999999999645 ) ) ;
#94402 = CARTESIAN_POINT ( 'NONE',  ( 29.57907552799942508, -3.316774720514426456, 29.21818156447044501 ) ) ;
#94403 = CARTESIAN_POINT ( 'NONE',  ( -125.5228709571500900, -24.14406661686764366, 10.28769366194080348 ) ) ;
#94404 = CARTESIAN_POINT ( 'NONE',  ( -127.5895376238167245, -23.48783264082479505, -1.443836473390056829 ) ) ;
#94405 = CARTESIAN_POINT ( 'NONE',  ( -8.160016139516647726, -19.69179572373923648, 11.49999999999998934 ) ) ;
#94406 = CARTESIAN_POINT ( 'NONE',  ( -122.5228709571500332, -23.48783264082477018, -1.443836473390084807 ) ) ;
#94407 = FACE_OUTER_BOUND ( 'NONE', #74854, .T. ) ;
#94408 = CARTESIAN_POINT ( 'NONE',  ( -108.6228709571500559, -23.47593901973091235, -1.443836447538999312 ) ) ;
#94409 = DIRECTION ( 'NONE',  ( 0.6451914333552788428, 0.000000000000000000, 0.7640209514960704107 ) ) ;
#94410 = CARTESIAN_POINT ( 'NONE',  ( 13.09772080625096891, 18.35129493929886380, -1.500000000000002220 ) ) ;
#94411 = AXIS2_PLACEMENT_3D ( 'NONE', #94912, #35024, #6930 ) ;
#94412 = B_SPLINE_SURFACE_WITH_KNOTS ( 'NONE', 3, 3, ( 
 ( #94851, #84854, #79124, #46296 ),
 ( #9619, #87238, #40580, #121 ),
 ( #2023, #56319, #17735, #48703 ),
 ( #43081, #12108, #13105, #20218 ),
 ( #34962, #50688, #44572, #11611 ),
 ( #35956, #90743, #44071, #65439 ),
 ( #20719, #67419, #13605, #51189 ),
 ( #36451, #50191, #34464, #97360 ),
 ( #3519, #66925, #51689, #65935 ),
 ( #82130, #81132, #4016, #42588 ) ),
 .UNSPECIFIED., .F., .F., .F.,
 ( 4, 3, 3, 4 ),
 ( 4, 4 ),
 ( 0.0004766839783821820095, 0.1491231665100173354, 0.2234464077758349099, 0.2977696490416524844 ),
 ( 0.3495362134072145244, 0.3507572252461916285 ),
 .UNSPECIFIED. ) ;
#94413 = PLANE ( 'NONE',  #399 ) ;
#94414 = ORIENTED_EDGE ( 'NONE', *, *, #60941, .F. ) ;
#94415 = CARTESIAN_POINT ( 'NONE',  ( 8.971512145086503409, -2.028487854913501032, 5.500000000000000000 ) ) ;
#94416 = CARTESIAN_POINT ( 'NONE',  ( -68.52287095715007581, -23.47593901973090524, -1.443836447538997092 ) ) ;
#94417 = CARTESIAN_POINT ( 'NONE',  ( 19.47230031930329730, 2.946587627359682493, 11.49999999999999645 ) ) ;
#94418 = CARTESIAN_POINT ( 'NONE',  ( -32.07722060962682065, -25.11966440015785196, 7.363003809050452375 ) ) ;
#94419 = CARTESIAN_POINT ( 'NONE',  ( 30.93860345374796594, -0.6647747205144264315, 19.84760796525321780 ) ) ;
#94420 = ORIENTED_EDGE ( 'NONE', *, *, #93631, .T. ) ;
#94421 = CARTESIAN_POINT ( 'NONE',  ( -99.63766005662118630, -23.48783264082478439, -1.443836473390062825 ) ) ;
#94422 = PLANE ( 'NONE',  #96646 ) ;
#94423 = CARTESIAN_POINT ( 'NONE',  ( -105.5228709571501327, -24.83620972994591369, 8.398175272781370992 ) ) ;
#94424 = CARTESIAN_POINT ( 'NONE',  ( 22.81105451610979173, 2.682774720514426559, -18.46691820600746681 ) ) ;
#94425 = CARTESIAN_POINT ( 'NONE',  ( 17.61170953066113398, -8.936083093766256980, -1.500000000000002220 ) ) ;
#94426 = VERTEX_POINT ( 'NONE', #98791 ) ;
#94427 = AXIS2_PLACEMENT_3D ( 'NONE', #84937, #77315, #7816 ) ;
#94428 = CARTESIAN_POINT ( 'NONE',  ( -20.17641613807547785, 1.360797614858565874, 11.49999999999999645 ) ) ;
#94429 = CARTESIAN_POINT ( 'NONE',  ( 12.98941176919429097, 3.316774720517114972, -28.15829778459866262 ) ) ;
#94430 = ORIENTED_EDGE ( 'NONE', *, *, #34432, .F. ) ;
#94431 = CARTESIAN_POINT ( 'NONE',  ( 27.86270917940689174, -5.965225279485572685, 29.02104833056109001 ) ) ;
#94432 = CARTESIAN_POINT ( 'NONE',  ( -11.64875734969026233, 0.3587747205144265483, 31.02402280011862246 ) ) ;
#94433 = CARTESIAN_POINT ( 'NONE',  ( -50.65677132892651713, -25.30358770098895249, 5.223192127046770494 ) ) ;
#94434 = CARTESIAN_POINT ( 'NONE',  ( -83.52287095715006160, -23.47593901973090524, -1.443836447538996648 ) ) ;
#94435 = EDGE_CURVE ( 'NONE', #7644, #8232, #14741, .T. ) ;
#94436 = CARTESIAN_POINT ( 'NONE',  ( -124.2228709571500502, -23.47593901973090524, -1.443836447538996204 ) ) ;
#94437 = ADVANCED_FACE ( 'NONE', ( #5453 ), #59757, .F. ) ;
#94438 = LINE ( 'NONE', #30536, #38090 ) ;
#94439 = CARTESIAN_POINT ( 'NONE',  ( -14.99618758923778117, -13.25627519679515665, 11.49999999999998934 ) ) ;
#94440 = EDGE_CURVE ( 'NONE', #33865, #96258, #75950, .T. ) ;
#94441 = CARTESIAN_POINT ( 'NONE',  ( 6.573941812937369455, 0.2639660507643281639, 9.334907998774166978E-16 ) ) ;
#94442 = CARTESIAN_POINT ( 'NONE',  ( -116.5544649402113180, -24.15620529776628800, 10.23563542870659759 ) ) ;
#94443 = ORIENTED_EDGE ( 'NONE', *, *, #50984, .F. ) ;
#94444 = ADVANCED_FACE ( 'NONE', ( #97799, #90191 ), #4959, .F. ) ;
#94445 = EDGE_CURVE ( 'NONE', #10131, #92742, #65646, .T. ) ;
#94446 = B_SPLINE_CURVE_WITH_KNOTS ( 'NONE', 3,
 ( #38747, #38248, #62108, #24523, #69715, #54992, #30642, #31138 ),
 .UNSPECIFIED., .F., .F.,
 ( 4, 2, 2, 4 ),
 ( -0.001224873891641426512, -0.0002244903592271102304, 0.0007758931731872060512, 0.002776660238015838614 ),
 .UNSPECIFIED. ) ;
#94447 = AXIS2_PLACEMENT_3D ( 'NONE', #53142, #91180, #67364 ) ;
#94449 = CARTESIAN_POINT ( 'NONE',  ( -104.6228709571500559, -23.48786465467241413, 11.44779295918254114 ) ) ;
#94448 = CC_DESIGN_SECURITY_CLASSIFICATION ( #83064, ( #100424 ) ) ;
#94450 = CARTESIAN_POINT ( 'NONE',  ( -109.8707484289256655, -25.29012748047656700, 3.397981883223208488 ) ) ;
#94451 = CARTESIAN_POINT ( 'NONE',  ( -35.46877372516544824, -24.92564183028978775, 1.928384488918258199 ) ) ;
#94452 = CARTESIAN_POINT ( 'NONE',  ( -100.5228709571500900, -24.63345952396255711, 9.038047939301508293 ) ) ;
#94453 = CARTESIAN_POINT ( 'NONE',  ( -117.0508430453642887, -25.34741532608440551, 3.801652799235187175 ) ) ;
#94454 = FACE_OUTER_BOUND ( 'NONE', #1394, .T. ) ;
#94455 = CARTESIAN_POINT ( 'NONE',  ( -49.50841769935764347, -25.26288593538659910, 3.984447754961206734 ) ) ;
#94456 = VECTOR ( 'NONE', #85195, 1000.000000000000114 ) ;
#94457 = B_SPLINE_CURVE_WITH_KNOTS ( 'NONE', 3,
 ( #97184, #68233, #90071, #52011, #20542, #90563, #83441 ),
 .UNSPECIFIED., .F., .F.,
 ( 4, 1, 1, 1, 4 ),
 ( 0.3452202732246780759, 0.4949101844912719983, 0.6446000957578658097, 0.7942900070244596211, 0.9439799182910535436 ),
 .UNSPECIFIED. ) ;
#94458 = CARTESIAN_POINT ( 'NONE',  ( -49.76238219317473721, -25.21081864179584997, 3.487169982528662615 ) ) ;
#94459 = ORIENTED_EDGE ( 'NONE', *, *, #23821, .F. ) ;
#94460 = CARTESIAN_POINT ( 'NONE',  ( 14.62039552936377085, -14.08751720214925207, 11.49999999999998934 ) ) ;
#94461 = VECTOR ( 'NONE', #63326, 1000.000000000000114 ) ;
#94462 = DIRECTION ( 'NONE',  ( 0.000000000000000000, -1.000000000000000000, 0.000000000000000000 ) ) ;
#94463 = CARTESIAN_POINT ( 'NONE',  ( -34.63527674217913699, -24.34968618360933590, 0.1864209137778841396 ) ) ;
#94464 = CARTESIAN_POINT ( 'NONE',  ( -105.6228709571500417, -23.85196035786902513, -0.8779234886474873711 ) ) ;
#94465 = ORIENTED_EDGE ( 'NONE', *, *, #23672, .T. ) ;
#94466 = CARTESIAN_POINT ( 'NONE',  ( -83.62287095715007013, -23.48786465467241769, 11.44779295918254469 ) ) ;
#94467 = CARTESIAN_POINT ( 'NONE',  ( 13.66866334921533799, -14.80927461459226890, -1.500000000000002220 ) ) ;
#94468 = EDGE_CURVE ( 'NONE', #41242, #23326, #19490, .T. ) ;
#94469 = CARTESIAN_POINT ( 'NONE',  ( -1.424071398598787397, -21.11453822904667277, 11.49999999999999645 ) ) ;
#94470 = CARTESIAN_POINT ( 'NONE',  ( 14.67205787815721862, 16.58792043909384262, -1.500000000000002220 ) ) ;
#94471 = CARTESIAN_POINT ( 'NONE',  ( -1.452656003914881477, -20.50939586048694352, 11.49999999999998934 ) ) ;
#94472 = CARTESIAN_POINT ( 'NONE',  ( -78.92287095715005307, -23.47596703998600631, 11.44779298504227860 ) ) ;
#94473 = ORIENTED_EDGE ( 'NONE', *, *, #79700, .F. ) ;
#94474 = CARTESIAN_POINT ( 'NONE',  ( 22.81105451610979173, 1.684774720501991396, -18.46691820600746681 ) ) ;
#94475 = VERTEX_POINT ( 'NONE', #51134 ) ;
#94476 = DIRECTION ( 'NONE',  ( -0.9976052577199500115, 0.000000000000000000, -0.06916465693916190594 ) ) ;
#94477 = CARTESIAN_POINT ( 'NONE',  ( 4.653846153846159517, -6.376774720514415407, 19.99999999999999289 ) ) ;
#94478 = ORIENTED_EDGE ( 'NONE', *, *, #83715, .F. ) ;
#94479 = ORIENTED_EDGE ( 'NONE', *, *, #23665, .T. ) ;
#94480 = ORIENTED_EDGE ( 'NONE', *, *, #28875, .T. ) ;
#94481 = CARTESIAN_POINT ( 'NONE',  ( -81.62287095715005592, -24.64965695001468404, 8.947790433994182280 ) ) ;
#94482 = CARTESIAN_POINT ( 'NONE',  ( -91.94687923781918926, -25.23397913219354649, 6.409327625488847602 ) ) ;
#94483 = CARTESIAN_POINT ( 'NONE',  ( 5.705253819860196529, -5.876774720514415407, 19.95963554344900714 ) ) ;
#94484 = CARTESIAN_POINT ( 'NONE',  ( 15.58315679939408582, 13.61395703526229894, -1.500000000000002220 ) ) ;
#94485 = CARTESIAN_POINT ( 'NONE',  ( 21.56569437331729233, -1.927008741106717604, 11.49999999999999645 ) ) ;
#94486 = ORIENTED_EDGE ( 'NONE', *, *, #29709, .T. ) ;
#94487 = CARTESIAN_POINT ( 'NONE',  ( -62.58953762381672448, -24.65952944569303895, 1.056160979905689024 ) ) ;
#94488 = CARTESIAN_POINT ( 'NONE',  ( -28.55620429048338593, -23.32635600711839885, 11.44779298526909983 ) ) ;
#94489 = CARTESIAN_POINT ( 'NONE',  ( 10.13505985054399083, -19.98934331558005439, -1.500000000000002220 ) ) ;
#94490 = ADVANCED_FACE ( 'NONE', ( #35905 ), #52135, .F. ) ;
#94491 = CARTESIAN_POINT ( 'NONE',  ( -47.50672211067188044, -23.96169478059712432, 10.65365249895718591 ) ) ;
#94492 = FACE_OUTER_BOUND ( 'NONE', #86744, .T. ) ;
#94493 = ORIENTED_EDGE ( 'NONE', *, *, #74563, .F. ) ;
#94494 = CARTESIAN_POINT ( 'NONE',  ( 29.57907552799943218, 3.518969226524878646, 29.21818156447044501 ) ) ;
#94495 = CARTESIAN_POINT ( 'NONE',  ( -114.6228709571500417, -23.48786465467241769, 11.44779295918253936 ) ) ;
#94496 = AXIS2_PLACEMENT_3D ( 'NONE', #33543, #64527, #95440 ) ;
#94497 = VERTEX_POINT ( 'NONE', #73974 ) ;
#94498 = EDGE_LOOP ( 'NONE', ( #18019, #19193, #32942, #17638, #50414, #34650, #73332, #7027, #69782, #27259, #21291, #81999, #62017, #90422, #63051, #57562, #91139, #18916, #67842, #54929 ) ) ;
#94499 = B_SPLINE_CURVE_WITH_KNOTS ( 'NONE', 3,
 ( #36590, #29469, #75640, #59442, #89386, #19859, #82269, #12745 ),
 .UNSPECIFIED., .F., .F.,
 ( 4, 2, 2, 4 ),
 ( -0.001240666984355839756, -0.0002401179793394981471, 0.0007604310256768434615, 0.002761529035709530365 ),
 .UNSPECIFIED. ) ;
#94500 = EDGE_CURVE ( 'NONE', #11983, #42816, #66381, .T. ) ;
#94501 = CARTESIAN_POINT ( 'NONE',  ( -70.55620429048339304, -23.48783264082478084, -1.443836473390066821 ) ) ;
#94502 = ORIENTED_EDGE ( 'NONE', *, *, #29638, .T. ) ;
#94503 = CARTESIAN_POINT ( 'NONE',  ( -68.62287095715005592, -29.50250786944525672, 11.44777988621623699 ) ) ;
#94504 = CARTESIAN_POINT ( 'NONE',  ( 13.48273455363431772, -16.43370779934446801, -1.500000000000002220 ) ) ;
#94505 = ORIENTED_EDGE ( 'NONE', *, *, #63816, .F. ) ;
#94506 = CARTESIAN_POINT ( 'NONE',  ( -50.49354941359371196, -24.40034930558990922, 0.3402023900116070698 ) ) ;
#94507 = CARTESIAN_POINT ( 'NONE',  ( 16.38291735060997567, -14.39268585342195905, -1.500000000000002220 ) ) ;
#94508 = CARTESIAN_POINT ( 'NONE',  ( -103.5550924144477705, -23.96169478059713498, 10.65365249895717881 ) ) ;
#94509 = CARTESIAN_POINT ( 'NONE',  ( 6.467769777575680834, -6.376774720514427841, 21.83821538399986650 ) ) ;
#94510 = CARTESIAN_POINT ( 'NONE',  ( 6.329711958793041049, -5.876774720514412742, 19.73172534246499765 ) ) ;
#94511 = CARTESIAN_POINT ( 'NONE',  ( 13.71991279636371175, 16.93377936151356877, -1.500000000000002220 ) ) ;
#94512 = CARTESIAN_POINT ( 'NONE',  ( -66.62287095715005592, -23.47593901973091235, -1.443836447539006196 ) ) ;
#94513 = VERTEX_POINT ( 'NONE', #28291 ) ;
#94514 = FACE_OUTER_BOUND ( 'NONE', #26378, .T. ) ;
#94515 = CARTESIAN_POINT ( 'NONE',  ( -85.51038857217308475, -24.15602025860895807, 10.28564288303535967 ) ) ;
#94516 = ORIENTED_EDGE ( 'NONE', *, *, #100021, .F. ) ;
#94517 = ORIENTED_EDGE ( 'NONE', *, *, #10830, .T. ) ;
#94518 = AXIS2_PLACEMENT_3D ( 'NONE', #80594, #65406, #58274 ) ;
#94519 = ORIENTED_EDGE ( 'NONE', *, *, #1793, .F. ) ;
#94520 = CARTESIAN_POINT ( 'NONE',  ( -28.37442136742509646, -24.86812948212714147, 2.469321321118715495 ) ) ;
#94521 = CARTESIAN_POINT ( 'NONE',  ( -82.62360240055558336, -24.65952944569304606, 1.056160979905702790 ) ) ;
#94522 = CARTESIAN_POINT ( 'NONE',  ( -6.410030533929251817, 20.24415959294862333, 11.49999999999998934 ) ) ;
#94523 = CARTESIAN_POINT ( 'NONE',  ( -94.50573621563975735, -24.65952944569304606, 1.056160979905701680 ) ) ;
#94524 = DIRECTION ( 'NONE',  ( -1.000000000000000000, -3.773278334444166432E-23, -8.201307841325785021E-29 ) ) ;
#94525 = CARTESIAN_POINT ( 'NONE',  ( -54.52287095715005449, -23.47593901973090169, -1.443836447538997092 ) ) ;
#94526 = CARTESIAN_POINT ( 'NONE',  ( -48.55620429048339304, -23.47596703998600276, 11.44779298504227505 ) ) ;
#94528 = CARTESIAN_POINT ( 'NONE',  ( 17.66168439605153395, -8.020940556088177686, -1.500000000000002220 ) ) ;
#94527 = AXIS2_PLACEMENT_3D ( 'NONE', #90570, #66267, #12447 ) ;
#94529 = CARTESIAN_POINT ( 'NONE',  ( 8.500000000000000000, -0.9000000000000000222, 3.750000000000000000 ) ) ;
#94530 = ORIENTED_EDGE ( 'NONE', *, *, #17952, .F. ) ;
#94531 = CARTESIAN_POINT ( 'NONE',  ( 19.32586673001642197, -2.567307930040524599, 11.49999999999999645 ) ) ;
#94532 = CARTESIAN_POINT ( 'NONE',  ( -5.238752036864926964, -6.376774720514410077, 19.51517878119694061 ) ) ;
#94533 = AXIS2_PLACEMENT_3D ( 'NONE', #61346, #46112, #76533 ) ;
#94534 = DIRECTION ( 'NONE',  ( 0.000000000000000000, -1.000000000000000000, -0.000000000000000000 ) ) ;
#94535 = ORIENTED_EDGE ( 'NONE', *, *, #9007, .F. ) ;
#94536 = CARTESIAN_POINT ( 'NONE',  ( -58.62287095715007013, -23.47596703998600276, 11.44779298504227683 ) ) ;
#94537 = CARTESIAN_POINT ( 'NONE',  ( -32.55620429048340014, -23.48786465467240347, 11.44779295918255713 ) ) ;
#94538 = B_SPLINE_CURVE_WITH_KNOTS ( 'NONE', 3,
 ( #27993, #57964, #73178, #34115, #26502, #20358 ),
 .UNSPECIFIED., .F., .F.,
 ( 4, 2, 4 ),
 ( 0.000000000000000000, 0.001380764517853252070, 0.002761529035706504140 ),
 .UNSPECIFIED. ) ;
#94539 = CARTESIAN_POINT ( 'NONE',  ( -103.5228709571501042, -23.47593901973090524, -1.443836447538996204 ) ) ;
#94540 = CARTESIAN_POINT ( 'NONE',  ( -93.55798342408773749, -23.73791477778911840, 11.05961554403170410 ) ) ;
#94541 = CARTESIAN_POINT ( 'NONE',  ( 6.681059570357060551, -18.48443787736713873, -1.500000000000002220 ) ) ;
#94542 = VERTEX_POINT ( 'NONE', #82574 ) ;
#94543 = DIRECTION ( 'NONE',  ( -1.000000000000000000, -0.000000000000000000, -0.000000000000000000 ) ) ;
#94544 = CARTESIAN_POINT ( 'NONE',  ( -114.5562042904833930, -23.47596703998600631, 11.44779298504227683 ) ) ;
#94545 = PERSON_AND_ORGANIZATION_ROLE ( 'creator' ) ;
#94546 = CARTESIAN_POINT ( 'NONE',  ( 3.296548071537245495, -6.376774720514426065, 21.29143507544719682 ) ) ;
#94547 = DIRECTION ( 'NONE',  ( 0.000000000000000000, 2.173523156925980399E-06, -0.9999999999976378895 ) ) ;
#94548 = CARTESIAN_POINT ( 'NONE',  ( -105.6228709571500275, -25.00182538069145721, 7.747789668545099317 ) ) ;
#94549 = CARTESIAN_POINT ( 'NONE',  ( -101.9327573176231283, -25.24367985958541638, 6.326438925865677021 ) ) ;
#94550 = EDGE_CURVE ( 'NONE', #20892, #58811, #32792, .T. ) ;
#94551 = APPLICATION_CONTEXT ( 'configuration controlled 3d designs of mechanical parts and assemblies' ) ;
#94552 = CARTESIAN_POINT ( 'NONE',  ( 5.671135738765417322, -6.376774720514422512, 20.99074880795119924 ) ) ;
#94553 = DIRECTION ( 'NONE',  ( -0.000000000000000000, 1.000000000000000000, -0.000000000000000000 ) ) ;
#94554 = CARTESIAN_POINT ( 'NONE',  ( -114.5149051635414992, -24.66019654487200441, 8.947790411086106843 ) ) ;
#94555 = CARTESIAN_POINT ( 'NONE',  ( -18.79874323561663729, 6.599581278811135654, -1.500000000000002220 ) ) ;
#94556 = AXIS2_PLACEMENT_3D ( 'NONE', #77525, #38480, #26131 ) ;
#94557 = EDGE_CURVE ( 'NONE', #35259, #32133, #13055, .T. ) ;
#94558 = CARTESIAN_POINT ( 'NONE',  ( -75.58468866288802701, -24.73531770709095312, 8.716586749053512051 ) ) ;
#94559 = CARTESIAN_POINT ( 'NONE',  ( -19.53060160647804722, 3.385818350044136338, -1.500000000000002220 ) ) ;
#94560 = ORIENTED_EDGE ( 'NONE', *, *, #99520, .F. ) ;
#94561 = CARTESIAN_POINT ( 'NONE',  ( -71.52287095715006160, -23.47593901973090169, -1.443836447538996870 ) ) ;
#94562 = EDGE_CURVE ( 'NONE', #46960, #13507, #78905, .T. ) ;
#94563 = AXIS2_PLACEMENT_3D ( 'NONE', #38993, #94780, #95289 ) ;
#94564 = ADVANCED_FACE ( 'NONE', ( #91182 ), #8452, .T. ) ;
#94565 = CARTESIAN_POINT ( 'NONE',  ( -50.67286173397793902, -25.13656437041104752, 7.082003562334411306 ) ) ;
#94566 = CARTESIAN_POINT ( 'NONE',  ( 5.271800844967073907, -6.376774720514426953, -28.56638892015272546 ) ) ;
#94567 = CARTESIAN_POINT ( 'NONE',  ( -20.69558417703438025, 1.077208295497980250, 11.49999999999999645 ) ) ;
#94568 = CARTESIAN_POINT ( 'NONE',  ( -89.81226385320383088, -29.50249917535260380, 7.447779886225679213 ) ) ;
#94569 = ADVANCED_FACE ( 'NONE', ( #99772 ), #77444, .T. ) ;
#94570 = CARTESIAN_POINT ( 'NONE',  ( -117.6228709571500559, -29.50250243563736774, 8.947779886222134493 ) ) ;
#94571 = CARTESIAN_POINT ( 'NONE',  ( -22.70586268970451371, -1.818501321912391999, 11.49999999999999645 ) ) ;
#94572 = B_SPLINE_CURVE_WITH_KNOTS ( 'NONE', 3,
 ( #47843, #45843, #38216, #69172 ),
 .UNSPECIFIED., .F., .F.,
 ( 4, 4 ),
 ( 0.000000000000000000, 0.0005192307692307857048 ),
 .UNSPECIFIED. ) ;
#94573 = VERTEX_POINT ( 'NONE', #54145 ) ;
#94574 = CARTESIAN_POINT ( 'NONE',  ( -69.54934929687469491, -24.15543982623907482, -0.2315651400026648155 ) ) ;
#94575 = CARTESIAN_POINT ( 'NONE',  ( -28.52287095715005805, -29.50248298729119867, -6.412432996800796609E-05 ) ) ;
#94576 = B_SPLINE_CURVE_WITH_KNOTS ( 'NONE', 3,
 ( #40286, #3244, #64654, #94565, #25048, #17440, #95568, #34178, #65154, #88463, #71240, #25557, #32666, #1727, #48407, #71742 ),
 .UNSPECIFIED., .F., .F.,
 ( 4, 2, 2, 2, 2, 2, 2, 4 ),
 ( 0.000000000000000000, 0.0002012173707785539726, 0.0004024347415571079452, 0.0008048694831142152398, 0.001006086853892760756, 0.001207304224671306271, 0.001408521595449852004, 0.001609738966228397520 ),
 .UNSPECIFIED. ) ;
#94577 = VERTEX_POINT ( 'NONE', #30279 ) ;
#94578 = CARTESIAN_POINT ( 'NONE',  ( -14.69473627950705108, 13.90061564059656440, -1.500000000000002220 ) ) ;
#94579 = EDGE_CURVE ( 'NONE', #36345, #51956, #60775, .T. ) ;
#94580 = CARTESIAN_POINT ( 'NONE',  ( 6.561060095583167495, -5.876774720514427841, 21.83518827598938117 ) ) ;
#94581 = CARTESIAN_POINT ( 'NONE',  ( -110.5228709571500758, -24.92604778743018556, 8.074972756849357225 ) ) ;
#94582 = ORIENTED_EDGE ( 'NONE', *, *, #72579, .F. ) ;
#94583 = DIRECTION ( 'NONE',  ( 3.773278334444167608E-23, -1.000000000000000000, 0.000000000000000000 ) ) ;
#94584 = CARTESIAN_POINT ( 'NONE',  ( -9.034649315346676701, 21.08484869742704504, 11.49999999999998934 ) ) ;
#94585 = CARTESIAN_POINT ( 'NONE',  ( -35.52287095715006870, -23.47596703998600631, 11.44779298504229281 ) ) ;
#94586 = CARTESIAN_POINT ( 'NONE',  ( 14.90458806734895703, -13.33898509196910886, -1.500000000000002220 ) ) ;
#94587 = CARTESIAN_POINT ( 'NONE',  ( -41.16195490483097075, -25.07454073646012560, 7.413582391003542327 ) ) ;
#94588 = CARTESIAN_POINT ( 'NONE',  ( 19.95448254803897115, -6.385634049875297258, 11.49999999999999645 ) ) ;
#94589 = CARTESIAN_POINT ( 'NONE',  ( -28.43316735593882072, -24.74360632443060837, 8.116853411926154394 ) ) ;
#94590 = CYLINDRICAL_SURFACE ( 'NONE', #2794, 1.249999999999997113 ) ;
#94591 = CARTESIAN_POINT ( 'NONE',  ( 22.04941498731238525, 0.3350016526185666255, 11.49999999999998934 ) ) ;
#94592 = B_SPLINE_CURVE_WITH_KNOTS ( 'NONE', 3,
 ( #3323, #34253, #65228, #71819 ),
 .UNSPECIFIED., .F., .F.,
 ( 4, 4 ),
 ( 0.000000000000000000, 9.999999999998897304E-05 ),
 .UNSPECIFIED. ) ;
#94593 = CARTESIAN_POINT ( 'NONE',  ( -69.52287095715006160, -24.65952944569304606, 1.056160979905697239 ) ) ;
#94594 = VECTOR ( 'NONE', #12051, 999.9999999999998863 ) ;
#94595 = ORIENTED_EDGE ( 'NONE', *, *, #94500, .F. ) ;
#94596 = CARTESIAN_POINT ( 'NONE',  ( -60.52287095715004739, -24.51163499207175178, 0.6490370598554290327 ) ) ;
#94597 = CARTESIAN_POINT ( 'NONE',  ( -49.93954932203694597, -25.18440119950784606, 3.376895537457810903 ) ) ;
#94598 = CARTESIAN_POINT ( 'NONE',  ( -51.62287095715005592, -24.64898659630367206, 1.056161002820821038 ) ) ;
#94599 = EDGE_LOOP ( 'NONE', ( #97573, #50043, #24976, #21213 ) ) ;
#94600 = CARTESIAN_POINT ( 'NONE',  ( 2.610950917001260141, -6.376774720514411854, 19.54489930512155027 ) ) ;
#94601 = ORIENTED_EDGE ( 'NONE', *, *, #18285, .F. ) ;
#94602 = AXIS2_PLACEMENT_3D ( 'NONE', #94162, #62236, #17042 ) ;
#94603 = ORIENTED_EDGE ( 'NONE', *, *, #24441, .T. ) ;
#94604 = FACE_OUTER_BOUND ( 'NONE', #66778, .T. ) ;
#94605 = DIRECTION ( 'NONE',  ( -3.773278334444166432E-23, 1.000000000000000000, 0.000000000000000000 ) ) ;
#94606 = CARTESIAN_POINT ( 'NONE',  ( -51.52287095715006160, -23.72747288104470087, -1.053458166803227458 ) ) ;
#94607 = CARTESIAN_POINT ( 'NONE',  ( 18.14102482237423075, -9.550406459077080967, -1.500000000000002220 ) ) ;
#94608 = EDGE_CURVE ( 'NONE', #93091, #38212, #6309, .T. ) ;
#94609 = VERTEX_POINT ( 'NONE', #85068 ) ;
#94610 = DIRECTION ( 'NONE',  ( 0.000000000000000000, -1.000000000000000000, 0.000000000000000000 ) ) ;
#94611 = CARTESIAN_POINT ( 'NONE',  ( -33.62287095715007013, -24.35013146730203104, 9.818937971375117257 ) ) ;
#94612 = CARTESIAN_POINT ( 'NONE',  ( 33.61456970919604714, 5.965225279485572685, -11.35828564741647462 ) ) ;
#94613 = CARTESIAN_POINT ( 'NONE',  ( -22.22805510923732086, 2.117028069546627922, 11.49999999999998934 ) ) ;
#94614 = CARTESIAN_POINT ( 'NONE',  ( -71.17271826174675198, -25.19999523107665595, 6.679460637636927878 ) ) ;
#94615 = CARTESIAN_POINT ( 'NONE',  ( -25.85053656567609082, -24.78713859579120893, 6.931755823712101083 ) ) ;
#94616 = ORIENTED_EDGE ( 'NONE', *, *, #58166, .T. ) ;
#94617 = DIRECTION ( 'NONE',  ( 0.000000000000000000, -2.173523156925980399E-06, 0.9999999999976378895 ) ) ;
#94618 = CARTESIAN_POINT ( 'NONE',  ( -113.5228709571500616, -23.48786465467242479, 11.44779295918253936 ) ) ;
#94619 = CARTESIAN_POINT ( 'NONE',  ( -20.61801493038525379, 2.926015819835423581, 11.49999999999998934 ) ) ;
#94620 = ORIENTED_EDGE ( 'NONE', *, *, #88664, .F. ) ;
#94622 = ORIENTED_EDGE ( 'NONE', *, *, #79461, .F. ) ;
#94621 = CARTESIAN_POINT ( 'NONE',  ( -116.5228709571500474, -23.96127896942151025, -0.6493128930935556653 ) ) ;
#94623 = ORIENTED_EDGE ( 'NONE', *, *, #73745, .T. ) ;
#94624 = CARTESIAN_POINT ( 'NONE',  ( -69.47374562227740569, -25.03149312170462792, 7.284001176654951948 ) ) ;
#94625 = CARTESIAN_POINT ( 'NONE',  ( -6.733481718715807141, 19.98004043397084928, -1.500000000000002220 ) ) ;
#94626 = EDGE_CURVE ( 'NONE', #13237, #12021, #30788, .T. ) ;
#94627 = ORIENTED_EDGE ( 'NONE', *, *, #52774, .T. ) ;
#94628 = CARTESIAN_POINT ( 'NONE',  ( -93.62287095715012697, -23.96177878511308634, 10.65340807706329507 ) ) ;
#94629 = FACE_OUTER_BOUND ( 'NONE', #17099, .T. ) ;
#94630 = CARTESIAN_POINT ( 'NONE',  ( -120.5181819260963465, -24.52399227489125266, 9.353111116836528183 ) ) ;
#94631 = CARTESIAN_POINT ( 'NONE',  ( -101.9507253916653440, -25.25419265818597125, 6.236250658476948594 ) ) ;
#94632 = CARTESIAN_POINT ( 'NONE',  ( -60.62287095715003460, -24.62285846362214770, 9.038163152653524435 ) ) ;
#94633 = PLANE ( 'NONE',  #57778 ) ;
#94634 = CARTESIAN_POINT ( 'NONE',  ( 29.80070917940689412, 6.475225279485573360, 27.39560796525321607 ) ) ;
#94636 = EDGE_LOOP ( 'NONE', ( #16141, #86717, #36824, #74753 ) ) ;
#94635 = CARTESIAN_POINT ( 'NONE',  ( 4.129723114849880083, -21.82631191821171512, 11.49999999999999645 ) ) ;
#94637 = CARTESIAN_POINT ( 'NONE',  ( -98.89486075440558466, -25.27154821674656660, 6.039256008359274119 ) ) ;
#94638 = EDGE_CURVE ( 'NONE', #13615, #45924, #39897, .T. ) ;
#94639 = CARTESIAN_POINT ( 'NONE',  ( -70.83100241438432931, -25.29887142613843309, 5.408397035483008430 ) ) ;
#94640 = VERTEX_POINT ( 'NONE', #7946 ) ;
#94641 = AXIS2_PLACEMENT_3D ( 'NONE', #5486, #36934, #59278 ) ;
#94642 = CARTESIAN_POINT ( 'NONE',  ( 17.73637878876437668, -14.10177982315242318, -1.500000000000002220 ) ) ;
#94644 = EDGE_LOOP ( 'NONE', ( #29347, #87874, #1485, #18817 ) ) ;
#94643 = CARTESIAN_POINT ( 'NONE',  ( -6.275748223059703257, -6.376774720514411854, 19.59984006504824805 ) ) ;
#94645 = AXIS2_PLACEMENT_3D ( 'NONE', #62036, #33081, #70137 ) ;
#94646 = ORIENTED_EDGE ( 'NONE', *, *, #70085, .F. ) ;
#94647 = CARTESIAN_POINT ( 'NONE',  ( 0.7051282051282027341, -6.376774720514408301, 19.19230769230768985 ) ) ;
#94648 = CC_DESIGN_PERSON_AND_ORGANIZATION_ASSIGNMENT ( #4963, #98290, ( #78282 ) ) ;
#94649 = CARTESIAN_POINT ( 'NONE',  ( -14.30055291515510518, -14.21740073472259525, 11.49999999999998934 ) ) ;
#94650 = CARTESIAN_POINT ( 'NONE',  ( -51.52287095715006870, -24.50321055353806443, 9.387540953477529371 ) ) ;
#94651 = VERTEX_POINT ( 'NONE', #22653 ) ;
#94652 = CARTESIAN_POINT ( 'NONE',  ( -42.62287095715006302, -23.73934037231756378, 11.05740245334329863 ) ) ;
#94653 = CARTESIAN_POINT ( 'NONE',  ( -20.28323820415832657, -9.445149539555593776, -1.500000000000002220 ) ) ;
#94654 = B_SPLINE_CURVE_WITH_KNOTS ( 'NONE', 3,
 ( #73152, #83627, #3149, #2643, #10747, #33581 ),
 .UNSPECIFIED., .F., .F.,
 ( 4, 2, 4 ),
 ( 6.391158118970788496E-06, 0.001387004593080784845, 0.002767618028042598960 ),
 .UNSPECIFIED. ) ;
#94655 = ORIENTED_EDGE ( 'NONE', *, *, #55317, .T. ) ;
#94656 = ORIENTED_EDGE ( 'NONE', *, *, #7752, .T. ) ;
#94657 = CARTESIAN_POINT ( 'NONE',  ( -112.5891708905303972, -24.35071581493543391, 9.817618358456018157 ) ) ;
#94658 = CARTESIAN_POINT ( 'NONE',  ( -119.6228709571500275, -24.33927499327855415, 9.819080762295815390 ) ) ;
#94659 = CARTESIAN_POINT ( 'NONE',  ( -110.5895376238167387, -25.00182538069145366, 7.747789668545099317 ) ) ;
#94660 = CARTESIAN_POINT ( 'NONE',  ( -41.52287095715005449, -23.48783264083359867, -1.443836473376375329 ) ) ;
#94661 = DIRECTION ( 'NONE',  ( 0.000000000000000000, 0.000000000000000000, -1.000000000000000000 ) ) ;
#94662 = CARTESIAN_POINT ( 'NONE',  ( -0.4769873229303308038, -19.55164744950295841, -1.500000000000002220 ) ) ;
#94663 = CARTESIAN_POINT ( 'NONE',  ( -49.64016321101554041, -25.30016906297147017, 4.382939044608830770 ) ) ;
#94664 = EDGE_LOOP ( 'NONE', ( #10009, #82218, #86239, #57313 ) ) ;
#94665 = CARTESIAN_POINT ( 'NONE',  ( 0.6623178260406717976, 21.47796536025111536, 11.49999999999998934 ) ) ;
#94666 = CARTESIAN_POINT ( 'NONE',  ( -128.5562987298943369, -23.48783264082478794, -1.443836473390056829 ) ) ;
#94667 = DIRECTION ( 'NONE',  ( -0.7689940216596065081, -4.164321980682960499E-15, 0.6392559695863502256 ) ) ;
#94668 = CARTESIAN_POINT ( 'NONE',  ( -101.7379430823953896, -25.25923547149210791, 3.830416064291135569 ) ) ;
#94669 = LINE ( 'NONE', #86058, #32596 ) ;
#94670 = CARTESIAN_POINT ( 'NONE',  ( 18.56524475492553705, -13.42312393814442650, -1.500000000000002220 ) ) ;
#94671 = DATE_AND_TIME ( #79446, #299 ) ;
#94672 = DIRECTION ( 'NONE',  ( 0.000000000000000000, -1.000000000000000000, 0.000000000000000000 ) ) ;
#94673 = CARTESIAN_POINT ( 'NONE',  ( -92.62287095715005592, -24.50216790748205753, 0.6166512839542542812 ) ) ;
#94674 = CARTESIAN_POINT ( 'NONE',  ( -1.591348192139008466, -19.94584644712825039, 11.49999999999999645 ) ) ;
#94675 = CARTESIAN_POINT ( 'NONE',  ( 5.090559816868301724, 3.309281602496330521, -27.56260619295190040 ) ) ;
#94676 = FACE_OUTER_BOUND ( 'NONE', #77857, .T. ) ;
#94677 = CARTESIAN_POINT ( 'NONE',  ( 29.80070917940689412, -5.965225279485572685, 27.39560796525321607 ) ) ;
#94678 = CARTESIAN_POINT ( 'NONE',  ( -20.27875734969026311, -4.543225279485573864, 24.00402280011862288 ) ) ;
#94679 = FACE_OUTER_BOUND ( 'NONE', #83562, .T. ) ;
#94680 = CARTESIAN_POINT ( 'NONE',  ( 19.84127317031322946, -0.4231496731191971561, 11.49999999999998934 ) ) ;
#94681 = CARTESIAN_POINT ( 'NONE',  ( -19.00758693998263738, -10.61793046214600089, 11.49999999999998934 ) ) ;
#94682 = LINE ( 'NONE', #56143, #77136 ) ;
#94683 = CARTESIAN_POINT ( 'NONE',  ( 9.442166470422634461, 17.27452087139410963, -1.500000000000002220 ) ) ;
#94684 = PLANE ( 'NONE',  #10296 ) ;
#94685 = CARTESIAN_POINT ( 'NONE',  ( -32.52287095715006160, -29.50250786944525672, 11.44777988621624409 ) ) ;
#94686 = DATE_AND_TIME ( #57155, #76611 ) ;
#94687 = ADVANCED_FACE ( 'NONE', ( #45527 ), #85568, .F. ) ;
#94688 = CARTESIAN_POINT ( 'NONE',  ( -103.5228709571500900, -24.33832256527049154, 0.1851278514138670062 ) ) ;
#94689 = CARTESIAN_POINT ( 'NONE',  ( 30.09341516180546350, 1.477225279485574028, -11.39311774897855933 ) ) ;
#94690 = CARTESIAN_POINT ( 'NONE',  ( -10.57813111170615983, 17.65445453266677234, 11.49999999999999645 ) ) ;
#94691 = DIRECTION ( 'NONE',  ( 0.8246584009594636333, 0.5656310827093757876, 0.000000000000000000 ) ) ;
#94692 = ADVANCED_FACE ( 'NONE', ( #32286 ), #91677, .F. ) ;
#94693 = B_SPLINE_CURVE_WITH_KNOTS ( 'NONE', 3,
 ( #91160, #84049, #75927, #14026, #19767, #52607 ),
 .UNSPECIFIED., .F., .F.,
 ( 4, 2, 4 ),
 ( 1.570887131794176733E-05, 0.001396322306279758688, 0.002776935741241575838 ),
 .UNSPECIFIED. ) ;
#94694 = VECTOR ( 'NONE', #46263, 1000.000000000000114 ) ;
#94695 = CARTESIAN_POINT ( 'NONE',  ( -120.5526916197902665, -24.83618233451451118, 1.606449574219542598 ) ) ;
#94696 = CARTESIAN_POINT ( 'NONE',  ( 21.71239400539012721, -6.292901409244172406, 11.49999999999999645 ) ) ;
#94697 = VERTEX_POINT ( 'NONE', #76446 ) ;
#94698 = CARTESIAN_POINT ( 'NONE',  ( -69.78016143783460734, -25.25639569820748065, 6.955938088137161301 ) ) ;
#94699 = CARTESIAN_POINT ( 'NONE',  ( -72.52287095715010423, -23.48783264082476308, -1.443836473390092578 ) ) ;
#94700 = FACE_OUTER_BOUND ( 'NONE', #10833, .T. ) ;
#94701 = CARTESIAN_POINT ( 'NONE',  ( -26.99920202386822865, -24.77267274619866910, 2.471679651391708088 ) ) ;
#94702 = EDGE_CURVE ( 'NONE', #38526, #63440, #67965, .T. ) ;
#94703 = DIRECTION ( 'NONE',  ( -3.773278334444166432E-23, 1.000000000000000000, 0.000000000000000000 ) ) ;
#94704 = VECTOR ( 'NONE', #35953, 1000.000000000000114 ) ;
#94705 = CARTESIAN_POINT ( 'NONE',  ( -28.52287095715005805, -23.32378116302990279, 11.44779301262222049 ) ) ;
#94706 = ORIENTED_EDGE ( 'NONE', *, *, #10457, .F. ) ;
#94707 = CARTESIAN_POINT ( 'NONE',  ( 17.26854690438276307, -15.35948741044508559, 11.49999999999999645 ) ) ;
#94708 = CARTESIAN_POINT ( 'NONE',  ( 17.70901601935662839, 14.43836031950349152, 11.49999999999998934 ) ) ;
#94709 = DIRECTION ( 'NONE',  ( 0.7512896232465892110, -0.000000000000000000, 0.6599726524652350657 ) ) ;
#94710 = CARTESIAN_POINT ( 'NONE',  ( -106.6228709571500559, -24.66019654487199730, 8.947790411086122830 ) ) ;
#94711 = CARTESIAN_POINT ( 'NONE',  ( -82.54134713839933113, -24.66019654487199730, 8.947790411086122830 ) ) ;
#94712 = CARTESIAN_POINT ( 'NONE',  ( 12.95044643391442030, 18.39415735498938176, 11.49999999999999645 ) ) ;
#94713 = ORIENTED_EDGE ( 'NONE', *, *, #65486, .F. ) ;
#94714 = CARTESIAN_POINT ( 'NONE',  ( -30.57287095715006231, -29.50250786944500803, 11.44777977285526838 ) ) ;
#94715 = CARTESIAN_POINT ( 'NONE',  ( -8.471812324360341151, -20.26817064352238162, -1.500000000000002220 ) ) ;
#94716 = CARTESIAN_POINT ( 'NONE',  ( -82.52287095715006160, -29.50248528299804818, 1.056150453629038477 ) ) ;
#94717 = CARTESIAN_POINT ( 'NONE',  ( -44.53462723111864818, -24.51419770103159479, 9.386484678747171628 ) ) ;
#94718 = CARTESIAN_POINT ( 'NONE',  ( -61.52287095715006160, -24.66019654487199730, 8.947790411086121054 ) ) ;
#94719 = ORIENTED_EDGE ( 'NONE', *, *, #19862, .T. ) ;
#94720 = DIRECTION ( 'NONE',  ( 1.000000000000000000, 0.000000000000000000, 0.000000000000000000 ) ) ;
#94721 = DIRECTION ( 'NONE',  ( 0.000000000000000000, 0.000000000000000000, -1.000000000000000000 ) ) ;
#94722 = EDGE_LOOP ( 'NONE', ( #22779, #41200, #79242, #97983 ) ) ;
#94723 = CARTESIAN_POINT ( 'NONE',  ( -1.317410511717131971, -20.46822056820986546, -1.500000000000002220 ) ) ;
#94724 = ORIENTED_EDGE ( 'NONE', *, *, #82823, .F. ) ;
#94725 = ORIENTED_EDGE ( 'NONE', *, *, #97562, .F. ) ;
#94726 = VERTEX_POINT ( 'NONE', #92180 ) ;
#94727 = ORIENTED_EDGE ( 'NONE', *, *, #13673, .F. ) ;
#94728 = CARTESIAN_POINT ( 'NONE',  ( 11.81885653190370888, -19.86314957129924608, -1.500000000000002220 ) ) ;
#94729 = CARTESIAN_POINT ( 'NONE',  ( -10.24059822343757808, -6.376774720514426953, 0.000000000000000000 ) ) ;
#94730 = CARTESIAN_POINT ( 'NONE',  ( -5.191926799570463658, 19.71030214607805675, -1.500000000000002220 ) ) ;
#94731 = ORIENTED_EDGE ( 'NONE', *, *, #90686, .F. ) ;
#94732 = FACE_OUTER_BOUND ( 'NONE', #43832, .T. ) ;
#94733 = FACE_OUTER_BOUND ( 'NONE', #17739, .T. ) ;
#94734 = EDGE_CURVE ( 'NONE', #94858, #55468, #46515, .T. ) ;
#94735 = FACE_OUTER_BOUND ( 'NONE', #43027, .T. ) ;
#94736 = CARTESIAN_POINT ( 'NONE',  ( 4.518205171808153509, -5.876774720514407413, 19.05004583296150500 ) ) ;
#94738 = ORIENTED_EDGE ( 'NONE', *, *, #4338, .T. ) ;
#94737 = CARTESIAN_POINT ( 'NONE',  ( -12.84383942963603964, -17.20202612561282862, 11.49999999999999645 ) ) ;
#94739 = CARTESIAN_POINT ( 'NONE',  ( -75.58469511993916967, -24.73486907724918282, 1.287355809206967683 ) ) ;
#94740 = LINE ( 'NONE', #96252, #11840 ) ;
#94741 = AXIS2_PLACEMENT_3D ( 'NONE', #92794, #36638, #46139 ) ;
#94742 = VERTEX_POINT ( 'NONE', #15055 ) ;
#94743 = CARTESIAN_POINT ( 'NONE',  ( -11.67826063220891086, 17.12864047899337550, -1.500000000000002220 ) ) ;
#94745 = EDGE_CURVE ( 'NONE', #22830, #61303, #37756, .T. ) ;
#94744 = ORIENTED_EDGE ( 'NONE', *, *, #37643, .F. ) ;
#94747 = ORIENTED_EDGE ( 'NONE', *, *, #50704, .F. ) ;
#94746 = CARTESIAN_POINT ( 'NONE',  ( -71.62287095715005592, -23.48783264082478084, -1.443836473390067487 ) ) ;
#94748 = DIRECTION ( 'NONE',  ( 1.000000000000000000, 0.000000000000000000, 0.000000000000000000 ) ) ;
#94749 = DIRECTION ( 'NONE',  ( 0.000000000000000000, 1.000000000000000000, 0.000000000000000000 ) ) ;
#94750 = EDGE_LOOP ( 'NONE', ( #11395, #68174, #93856, #38793 ) ) ;
#94751 = ORIENTED_EDGE ( 'NONE', *, *, #667, .T. ) ;
#94752 = CARTESIAN_POINT ( 'NONE',  ( -40.52287095715006160, -24.63287334234178161, 0.9662140553045331925 ) ) ;
#94753 = CARTESIAN_POINT ( 'NONE',  ( -42.56072409594817429, -23.73791477778911485, 11.05961554403171299 ) ) ;
#94754 = CARTESIAN_POINT ( 'NONE',  ( -43.62370922560796060, -24.66019654487199375, 8.947790411086121054 ) ) ;
#94756 = VERTEX_POINT ( 'NONE', #7441 ) ;
#94755 = CARTESIAN_POINT ( 'NONE',  ( 16.16784302627978320, -14.93143893958281154, 11.49999999999999645 ) ) ;
#94757 = CARTESIAN_POINT ( 'NONE',  ( -47.62287095715005592, -23.96177878511308634, 10.65340807706330217 ) ) ;
#94758 = CARTESIAN_POINT ( 'NONE',  ( -16.68516988606489448, 15.22057433622007316, 11.49999999999998934 ) ) ;
#94759 = CARTESIAN_POINT ( 'NONE',  ( 19.96068868648078620, -6.529529906025321573, 11.49999999999998934 ) ) ;
#94761 = ORIENTED_EDGE ( 'NONE', *, *, #17827, .T. ) ;
#94760 = CARTESIAN_POINT ( 'NONE',  ( -30.49303573129054357, -23.47596703998576118, 11.44779287168131710 ) ) ;
#94762 = ORIENTED_EDGE ( 'NONE', *, *, #89441, .F. ) ;
#94763 = DIRECTION ( 'NONE',  ( -0.000000000000000000, 1.000000000000000000, -0.000000000000000000 ) ) ;
#94764 = AXIS2_PLACEMENT_3D ( 'NONE', #79476, #17073, #63783 ) ;
#94765 = ADVANCED_FACE ( 'NONE', ( #69352 ), #100269, .F. ) ;
#94766 = B_SPLINE_CURVE_WITH_KNOTS ( 'NONE', 3,
 ( #63568, #25477, #3164, #34105 ),
 .UNSPECIFIED., .F., .F.,
 ( 4, 4 ),
 ( 0.000000000000000000, 0.0001000000000000028644 ),
 .UNSPECIFIED. ) ;
#94767 = CARTESIAN_POINT ( 'NONE',  ( -57.58746848899791360, -24.35071581493543036, 9.817618358456028815 ) ) ;
#94768 = ORIENTED_EDGE ( 'NONE', *, *, #15749, .T. ) ;
#94769 = CARTESIAN_POINT ( 'NONE',  ( 12.34367313097222763, -17.18290682204727915, 11.49999999999998934 ) ) ;
#94770 = DIRECTION ( 'NONE',  ( 0.000000000000000000, 0.000000000000000000, -1.000000000000000000 ) ) ;
#94771 = CARTESIAN_POINT ( 'NONE',  ( -60.73340568811573803, -25.03722704563418944, 7.590184509431679771 ) ) ;
#94772 = CARTESIAN_POINT ( 'NONE',  ( -75.62287095715004170, -23.84047902841601640, -0.8780736468305718745 ) ) ;
#94773 = DIRECTION ( 'NONE',  ( 0.000000000000000000, 0.000000000000000000, 1.000000000000000000 ) ) ;
#94774 = CARTESIAN_POINT ( 'NONE',  ( -101.5228709571500048, -23.73907113216990084, -1.053371485793246354 ) ) ;
#94775 = CARTESIAN_POINT ( 'NONE',  ( -21.14947813473477822, 6.846651710974520633, -1.500000000000002220 ) ) ;
#94776 = CARTESIAN_POINT ( 'NONE',  ( -114.5916530783749323, -23.96119346886881729, -0.6495511937831860427 ) ) ;
#94777 = VECTOR ( 'NONE', #10636, 1000.000000000000114 ) ;
#94778 = VERTEX_POINT ( 'NONE', #64775 ) ;
#94779 = CARTESIAN_POINT ( 'NONE',  ( -25.92875734969025814, -3.316774720514426456, 0.7300228001186309656 ) ) ;
#94780 = DIRECTION ( 'NONE',  ( -0.000000000000000000, -1.000000000000000000, -0.000000000000000000 ) ) ;
#94781 = CARTESIAN_POINT ( 'NONE',  ( -126.5222601566329530, -23.48783264082477018, -1.443836473390087249 ) ) ;
#94782 = ADVANCED_FACE ( 'NONE', ( #11449 ), #2859, .T. ) ;
#94783 = CARTESIAN_POINT ( 'NONE',  ( -71.62287095715005592, -23.48783264082478084, -1.443836473390067487 ) ) ;
#94784 = LINE ( 'NONE', #85677, #63161 ) ;
#94785 = CARTESIAN_POINT ( 'NONE',  ( 1.793504005174451077, 19.40006364325761012, -1.500000000000002220 ) ) ;
#94786 = CARTESIAN_POINT ( 'NONE',  ( -21.12015818079280649, -3.594773940630530795, -1.500000000000002220 ) ) ;
#94787 = LINE ( 'NONE', #48640, #83895 ) ;
#94788 = CARTESIAN_POINT ( 'NONE',  ( -60.63370354675536333, -24.63419186845290199, 9.035850630957110496 ) ) ;
#94789 = DIRECTION ( 'NONE',  ( 0.000000000000000000, -0.8406134417706495610, -0.5416355246053408123 ) ) ;
#94790 = CARTESIAN_POINT ( 'NONE',  ( -77.49793897276390453, -24.65952944569304606, 1.056160979905701458 ) ) ;
#94791 = CARTESIAN_POINT ( 'NONE',  ( 2.440706796964721370, 22.61111150098722788, -1.500000000000002220 ) ) ;
#94792 = DIRECTION ( 'NONE',  ( 0.8415104435810858430, 1.975826385823533048E-23, -0.5402408475337314719 ) ) ;
#94793 = CARTESIAN_POINT ( 'NONE',  ( -102.5930987670637791, -23.96119346886881729, -0.6495511937831878191 ) ) ;
#94794 = CARTESIAN_POINT ( 'NONE',  ( -80.52287095715006160, -24.99132157543083821, 2.256160258750667502 ) ) ;
#94795 = CARTESIAN_POINT ( 'NONE',  ( -0.3680779360730609406, 19.82951397037014729, 11.49999999999999645 ) ) ;
#94796 = CARTESIAN_POINT ( 'NONE',  ( 5.329826657887789310, -6.376774720514418959, 20.66144943787464783 ) ) ;
#94797 = ADVANCED_FACE ( 'NONE', ( #33791 ), #63256, .F. ) ;
#94798 = FACE_OUTER_BOUND ( 'NONE', #79802, .T. ) ;
#94799 = CARTESIAN_POINT ( 'NONE',  ( -51.52287095715008292, -23.47593901973090169, -1.443836447538997092 ) ) ;
#94800 = ADVANCED_FACE ( 'NONE', ( #48024 ), #41922, .F. ) ;
#94801 = ORIENTED_EDGE ( 'NONE', *, *, #58412, .F. ) ;
#94802 = DIRECTION ( 'NONE',  ( -0.000000000000000000, 2.173523156925979552E-06, -0.9999999999976378895 ) ) ;
#94803 = LINE ( 'NONE', #15679, #3782 ) ;
#94804 = CARTESIAN_POINT ( 'NONE',  ( -75.58953762381673869, -24.99132157543084176, 2.256160258750496084 ) ) ;
#94805 = CARTESIAN_POINT ( 'NONE',  ( -21.46818342838279392, -2.986162219498790904, -1.500000000000002220 ) ) ;
#94806 = CYLINDRICAL_SURFACE ( 'NONE', #70706, 5.500000000000001776 ) ;
#94807 = CARTESIAN_POINT ( 'NONE',  ( 10.93668938013857783, -16.14717738681254033, -1.500000000000002220 ) ) ;
#94808 = CARTESIAN_POINT ( 'NONE',  ( -123.6228709571500559, -24.66019654487200086, 8.947790411086117501 ) ) ;
#94809 = ORIENTED_EDGE ( 'NONE', *, *, #47177, .T. ) ;
#94810 = AXIS2_PLACEMENT_3D ( 'NONE', #42426, #27181, #73358 ) ;
#94811 = B_SPLINE_CURVE_WITH_KNOTS ( 'NONE', 3,
 ( #24467, #85873, #40702, #17359, #71655, #2155, #64067, #95486 ),
 .UNSPECIFIED., .F., .F.,
 ( 4, 2, 2, 4 ),
 ( -0.001240666984355833034, -0.0002401179793394905577, 0.0007604310256768519183, 0.002761529035709536003 ),
 .UNSPECIFIED. ) ;
#94812 = CARTESIAN_POINT ( 'NONE',  ( -1.067026067711715154, -20.38227831319515460, 11.49999999999999645 ) ) ;
#94813 = CARTESIAN_POINT ( 'NONE',  ( 8.071512145086503054, -2.028487854913504140, 5.500000000000000000 ) ) ;
#94814 = EDGE_CURVE ( 'NONE', #50535, #59834, #94177, .T. ) ;
#94815 = CARTESIAN_POINT ( 'NONE',  ( 7.462166178408539352, 6.475225279485573360, -27.67315496249664974 ) ) ;
#94816 = EDGE_CURVE ( 'NONE', #77603, #32014, #63768, .T. ) ;
#94817 = ORIENTED_EDGE ( 'NONE', *, *, #24180, .T. ) ;
#94818 = CARTESIAN_POINT ( 'NONE',  ( -80.51244414166535535, -25.03284467579916495, 7.563174216508125269 ) ) ;
#94819 = CARTESIAN_POINT ( 'NONE',  ( 33.63447098073278596, 3.363532777116247541, -11.63841935007238426 ) ) ;
#94820 = CARTESIAN_POINT ( 'NONE',  ( -75.55620429048340725, -23.47596703998600276, 11.44779298504227683 ) ) ;
#94821 = DIRECTION ( 'NONE',  ( 0.000000000000000000, -1.000000000000000000, 0.000000000000000000 ) ) ;
#94822 = CARTESIAN_POINT ( 'NONE',  ( 29.73860345376319003, 1.477225279485574028, -1.272392034746785860 ) ) ;
#94823 = EDGE_CURVE ( 'NONE', #13993, #18934, #50031, .T. ) ;
#94824 = CARTESIAN_POINT ( 'NONE',  ( -109.5961215800431745, -23.48783264082476663, -1.443836473390089470 ) ) ;
#94825 = VERTEX_POINT ( 'NONE', #33280 ) ;
#94826 = FACE_OUTER_BOUND ( 'NONE', #7878, .T. ) ;
#94827 = EDGE_CURVE ( 'NONE', #7414, #95483, #74074, .T. ) ;
#94828 = CARTESIAN_POINT ( 'NONE',  ( -22.24355531667433539, 5.575215412481045796, 11.49999999999999645 ) ) ;
#94829 = CARTESIAN_POINT ( 'NONE',  ( -4.508144621425604903, 22.28865971958312997, 11.49999999999998934 ) ) ;
#94830 = VERTEX_POINT ( 'NONE', #86573 ) ;
#94831 = CARTESIAN_POINT ( 'NONE',  ( -110.5109840011334086, -24.92592662359561473, 8.075495903018000021 ) ) ;
#94832 = CARTESIAN_POINT ( 'NONE',  ( -48.52287095715006160, -24.64898659630367561, 1.056161002820821038 ) ) ;
#94833 = CARTESIAN_POINT ( 'NONE',  ( -90.50790128547902214, -24.40034930558990922, 0.3402023900116079580 ) ) ;
#94834 = DIRECTION ( 'NONE',  ( -3.773278334453079618E-23, 0.9999999999976377785, 2.173523156925979975E-06 ) ) ;
#94835 = AXIS2_PLACEMENT_3D ( 'NONE', #28941, #75596, #36547 ) ;
#94836 = DIRECTION ( 'NONE',  ( 0.9975640502598241977, -0.06975647374412546897, -0.000000000000000000 ) ) ;
#94837 = CARTESIAN_POINT ( 'NONE',  ( -27.32356460660396635, -24.75521138200594251, 2.326351302823062461 ) ) ;
#94838 = CARTESIAN_POINT ( 'NONE',  ( -122.5201565697420705, -24.15543982623907482, -0.2315651400026565998 ) ) ;
#94839 = CARTESIAN_POINT ( 'NONE',  ( -39.62287095715005592, -23.47593901973091235, -1.443836447539011525 ) ) ;
#94840 = ORIENTED_EDGE ( 'NONE', *, *, #12786, .T. ) ;
#94841 = CARTESIAN_POINT ( 'NONE',  ( -18.82316870354832616, 7.800066519331792847, -1.500000000000002220 ) ) ;
#94842 = VERTEX_POINT ( 'NONE', #3364 ) ;
#94843 = ORIENTED_EDGE ( 'NONE', *, *, #56004, .T. ) ;
#94844 = CARTESIAN_POINT ( 'NONE',  ( 21.12055942831636202, -9.126644407798330860, -1.500000000000002220 ) ) ;
#94845 = DIRECTION ( 'NONE',  ( 0.000000000000000000, -0.000000000000000000, 1.000000000000000000 ) ) ;
#94846 = AXIS2_PLACEMENT_3D ( 'NONE', #88907, #11271, #64595 ) ;
#94847 = ORIENTED_EDGE ( 'NONE', *, *, #41434, .T. ) ;
#94848 = DIRECTION ( 'NONE',  ( -0.9161084732596777025, 0.000000000000000000, 0.4009304992412306978 ) ) ;
#94849 = DIRECTION ( 'NONE',  ( -0.000000000000000000, 1.000000000000000000, -0.000000000000000000 ) ) ;
#94850 = VECTOR ( 'NONE', #83862, 1000.000000000000000 ) ;
#94851 = CARTESIAN_POINT ( 'NONE',  ( -95.64416171314925919, -23.48783264082477373, -1.443836473390088804 ) ) ;
#94852 = DIRECTION ( 'NONE',  ( -0.000000000000000000, -0.000000000000000000, -1.000000000000000000 ) ) ;
#94854 = ORIENTED_EDGE ( 'NONE', *, *, #55005, .F. ) ;
#94853 = CARTESIAN_POINT ( 'NONE',  ( -21.15786647118399699, 2.672229404501205163, 11.49999999999999645 ) ) ;
#94855 = ORIENTED_EDGE ( 'NONE', *, *, #13227, .T. ) ;
#94856 = CARTESIAN_POINT ( 'NONE',  ( -2.380169663812839342, 22.11153957539610104, 11.49999999999998934 ) ) ;
#94857 = CARTESIAN_POINT ( 'NONE',  ( 9.220172233967117492, 18.46515239161685784, 11.49999999999998934 ) ) ;
#94858 = VERTEX_POINT ( 'NONE', #2352 ) ;
#94859 = EDGE_CURVE ( 'NONE', #39472, #74167, #41535, .T. ) ;
#94860 = PLANE ( 'NONE',  #918 ) ;
#94861 = EDGE_CURVE ( 'NONE', #41242, #28943, #40407, .T. ) ;
#94862 = CARTESIAN_POINT ( 'NONE',  ( -68.92598737797662523, -25.11539253604531297, 2.804427796191110378 ) ) ;
#94863 = ORIENTED_EDGE ( 'NONE', *, *, #81750, .T. ) ;
#94864 = CARTESIAN_POINT ( 'NONE',  ( -65.52287095715006160, -25.00158670708909625, 2.256160236439166411 ) ) ;
#94865 = ORIENTED_EDGE ( 'NONE', *, *, #26195, .T. ) ;
#94866 = CARTESIAN_POINT ( 'NONE',  ( -56.52287095715006870, -24.64965694238407323, 8.947790433994201820 ) ) ;
#94867 = CARTESIAN_POINT ( 'NONE',  ( -6.911038104174170194, -19.68591361114308214, -1.500000000000002220 ) ) ;
#94868 = CARTESIAN_POINT ( 'NONE',  ( 13.92123049006271707, -16.85212209846622855, 11.49999999999999645 ) ) ;
#94869 = CARTESIAN_POINT ( 'NONE',  ( -26.50032570333037185, -24.77993642618010739, 6.891654967618674021 ) ) ;
#94870 = PLANE ( 'NONE',  #4602 ) ;
#94871 = CARTESIAN_POINT ( 'NONE',  ( -5.125883829288005344, 21.89707322345674712, -1.500000000000002220 ) ) ;
#94872 = CARTESIAN_POINT ( 'NONE',  ( -26.31589504439661198, -24.97067121658517763, 6.467908153096676216 ) ) ;
#94873 = DIRECTION ( 'NONE',  ( 0.000000000000000000, 0.000000000000000000, -1.000000000000000000 ) ) ;
#94874 = CARTESIAN_POINT ( 'NONE',  ( 3.960462906497916435, -5.876774720514426953, 21.82884394085917279 ) ) ;
#94875 = ORIENTED_EDGE ( 'NONE', *, *, #59997, .F. ) ;
#94876 = VECTOR ( 'NONE', #83708, 1000.000000000000114 ) ;
#94877 = VERTEX_POINT ( 'NONE', #88087 ) ;
#94878 = EDGE_LOOP ( 'NONE', ( #75236, #65432, #30094, #56461 ) ) ;
#94879 = CARTESIAN_POINT ( 'NONE',  ( -52.65920731591500470, -23.48783264082478439, -1.443836473390069708 ) ) ;
#94880 = EDGE_LOOP ( 'NONE', ( #28616, #41741, #65359, #7724 ) ) ;
#94881 = B_SPLINE_CURVE_WITH_KNOTS ( 'NONE', 3,
 ( #23583, #70779, #54553, #15974, #32204, #46944 ),
 .UNSPECIFIED., .F., .F.,
 ( 4, 2, 4 ),
 ( 0.000000000000000000, 0.001380764517854764966, 0.002761529035709529931 ),
 .UNSPECIFIED. ) ;
#94882 = EDGE_CURVE ( 'NONE', #22347, #96941, #18559, .T. ) ;
#94883 = CARTESIAN_POINT ( 'NONE',  ( -16.30254408640404051, -13.89340296626662230, -1.500000000000002220 ) ) ;
#94884 = CARTESIAN_POINT ( 'NONE',  ( -18.94483701893047467, 11.91932228829616669, 11.49999999999999645 ) ) ;
#94885 = VERTEX_POINT ( 'NONE', #32786 ) ;
#94886 = CARTESIAN_POINT ( 'NONE',  ( 31.29611288755342002, -5.755914996345237178, -2.011851919325042370 ) ) ;
#94887 = CARTESIAN_POINT ( 'NONE',  ( 20.15827220212406701, 6.050813824765241655, 11.49999999999998934 ) ) ;
#94888 = CARTESIAN_POINT ( 'NONE',  ( -30.56645522924517167, -24.05349334839690556, 10.47557002954947336 ) ) ;
#94889 = CARTESIAN_POINT ( 'NONE',  ( -19.91179686852411734, 0.6080443046932394457, -1.500000000000002220 ) ) ;
#94890 = CARTESIAN_POINT ( 'NONE',  ( -127.5228709571500616, -29.50247984919015209, -1.443849546365044922 ) ) ;
#94891 = LINE ( 'NONE', #26390, #6970 ) ;
#94892 = EDGE_CURVE ( 'NONE', #9907, #72214, #94682, .T. ) ;
#94893 = CARTESIAN_POINT ( 'NONE',  ( 10.81757466760856801, -19.22619917341675588, -1.500000000000002220 ) ) ;
#94894 = ORIENTED_EDGE ( 'NONE', *, *, #55288, .F. ) ;
#94895 = CARTESIAN_POINT ( 'NONE',  ( -116.6262420726256153, -24.15543982623908548, -0.2315651400026406959 ) ) ;
#94896 = EDGE_CURVE ( 'NONE', #90018, #7123, #65274, .T. ) ;
#94897 = DIRECTION ( 'NONE',  ( 0.000000000000000000, 2.173523156925980399E-06, -0.9999999999976378895 ) ) ;
#94898 = CARTESIAN_POINT ( 'NONE',  ( 20.34438994040483806, -4.565235006643893811, 11.49999999999999645 ) ) ;
#94899 = EDGE_CURVE ( 'NONE', #93240, #29476, #35009, .T. ) ;
#94900 = EDGE_CURVE ( 'NONE', #58571, #38564, #92200, .T. ) ;
#94901 = DIRECTION ( 'NONE',  ( 0.000000000000000000, -1.000000000000000000, 0.000000000000000000 ) ) ;
#94902 = CARTESIAN_POINT ( 'NONE',  ( -125.5228709571501184, -23.84081130425357742, 10.88220057483160019 ) ) ;
#94903 = ADVANCED_FACE ( 'NONE', ( #5832 ), #28674, .T. ) ;
#94904 = CARTESIAN_POINT ( 'NONE',  ( -20.27875734969026311, -6.143225279485574397, 24.00402280011862288 ) ) ;
#94905 = CARTESIAN_POINT ( 'NONE',  ( -21.15786647118399699, 2.672229404501205163, 11.49999999999998934 ) ) ;
#94906 = CARTESIAN_POINT ( 'NONE',  ( -97.62287095715009855, -23.73934037231757443, 11.05740245334328797 ) ) ;
#94907 = LINE ( 'NONE', #9677, #93250 ) ;
#94908 = DIRECTION ( 'NONE',  ( 0.000000000000000000, 0.000000000000000000, -1.000000000000000000 ) ) ;
#94909 = CARTESIAN_POINT ( 'NONE',  ( -4.993225604111834137, -0.3587747205143964613, -29.11654937215279304 ) ) ;
#94910 = CARTESIAN_POINT ( 'NONE',  ( 11.79716412695777272, 19.27136520130675024, -1.500000000000002220 ) ) ;
#94911 = AXIS2_PLACEMENT_3D ( 'NONE', #22072, #76848, #5370 ) ;
#94912 = CARTESIAN_POINT ( 'NONE',  ( 5.202077965628057576, -7.402934475628873363E-15, 2.038091937962834166 ) ) ;
#94913 = ORIENTED_EDGE ( 'NONE', *, *, #86238, .T. ) ;
#94914 = AXIS2_PLACEMENT_3D ( 'NONE', #28996, #21370, #52344 ) ;
#94915 = CARTESIAN_POINT ( 'NONE',  ( -35.62287095715007013, -23.85229601348995843, 10.88205029486209696 ) ) ;
#94916 = CARTESIAN_POINT ( 'NONE',  ( -31.65923204074635322, -23.73791477778911130, 11.05961554403171299 ) ) ;
#94917 = CARTESIAN_POINT ( 'NONE',  ( 17.66836560233463516, 8.693963128369697202, 11.49999999999999645 ) ) ;
#94918 = CARTESIAN_POINT ( 'NONE',  ( -40.92287095715006728, -23.47593901973090169, -1.443836447538997980 ) ) ;
#94919 = CARTESIAN_POINT ( 'NONE',  ( -119.5228709571500758, -23.95044443724993144, 10.65354141964648882 ) ) ;
#94920 = EDGE_CURVE ( 'NONE', #40199, #4283, #34796, .T. ) ;
#94921 = EDGE_CURVE ( 'NONE', #80400, #79347, #69205, .T. ) ;
#94922 = ORIENTED_EDGE ( 'NONE', *, *, #87867, .T. ) ;
#94923 = VECTOR ( 'NONE', #93023, 1000.000000000000000 ) ;
#94924 = CARTESIAN_POINT ( 'NONE',  ( -99.55766089306172262, -23.73766607897671577, -1.055555164236429366 ) ) ;
#94925 = DIRECTION ( 'NONE',  ( -1.000000000000000000, 0.000000000000000000, -0.000000000000000000 ) ) ;
#94926 = CARTESIAN_POINT ( 'NONE',  ( -124.6228709571500559, -24.64898659630368627, 1.056161002820833028 ) ) ;
#94927 = PLANE ( 'NONE',  #21008 ) ;
#94929 = FACE_OUTER_BOUND ( 'NONE', #74808, .T. ) ;
#94928 = VECTOR ( 'NONE', #65649, 1000.000000000000000 ) ;
#94930 = B_SPLINE_CURVE_WITH_KNOTS ( 'NONE', 3,
 ( #2818, #4809, #18524, #33758, #35761, #11418, #34757, #4313 ),
 .UNSPECIFIED., .F., .F.,
 ( 4, 2, 2, 4 ),
 ( -0.001240666984355850598, -0.0002401179793395079049, 0.0007604310256768347879, 0.002761529035709519957 ),
 .UNSPECIFIED. ) ;
#94931 = CARTESIAN_POINT ( 'NONE',  ( 31.41423154468143153, -4.132774720514426292, -0.3119954678742140053 ) ) ;
#94932 = CARTESIAN_POINT ( 'NONE',  ( 16.04393857186779115, -11.51807295290239885, -1.500000000000002220 ) ) ;
#94933 = ORIENTED_EDGE ( 'NONE', *, *, #18090, .T. ) ;
#94934 = CARTESIAN_POINT ( 'NONE',  ( -6.993686169601437186, 18.98418669460116348, 11.49999999999999645 ) ) ;
#94935 = CARTESIAN_POINT ( 'NONE',  ( 12.48433401490028949, 6.376774720514426953, -25.05541855807676299 ) ) ;
#94936 = EDGE_CURVE ( 'NONE', #34838, #92190, #75833, .T. ) ;
#94937 = EDGE_CURVE ( 'NONE', #24503, #62807, #92090, .T. ) ;
#94938 = VERTEX_POINT ( 'NONE', #74349 ) ;
#94939 = LINE ( 'NONE', #42178, #5416 ) ;
#94940 = CARTESIAN_POINT ( 'NONE',  ( -72.55620429048340725, -23.47596703998600276, 11.44779298504227683 ) ) ;
#94941 = CARTESIAN_POINT ( 'NONE',  ( -100.4498239493576648, -25.03145178868323129, 7.563174219535599541 ) ) ;
#94942 = CARTESIAN_POINT ( 'NONE',  ( 13.10664265030973930, -0.3587747205144256601, -28.18129937523770678 ) ) ;
#94943 = PLANE ( 'NONE',  #57083 ) ;
#94944 = CARTESIAN_POINT ( 'NONE',  ( -24.90875734969025501, -5.965225279485572685, 30.00402280011862288 ) ) ;
#94945 = CARTESIAN_POINT ( 'NONE',  ( -17.62595516807937557, -9.487554784798948759, 11.49999999999998934 ) ) ;
#94946 = ADVANCED_FACE ( 'NONE', ( #12936 ), #68821, .T. ) ;
#94947 = CARTESIAN_POINT ( 'NONE',  ( -58.62287095715004881, -24.64898659630367916, 1.056161002820822592 ) ) ;
#94948 = CARTESIAN_POINT ( 'NONE',  ( -116.5926300250966250, -23.73791477778912551, 11.05961554403170055 ) ) ;
#94949 = VERTEX_POINT ( 'NONE', #58632 ) ;
#94950 = ADVANCED_FACE ( 'NONE', ( #12444 ), #51022, .F. ) ;
#94951 = EDGE_CURVE ( 'NONE', #82135, #57944, #66765, .T. ) ;
#94952 = CARTESIAN_POINT ( 'NONE',  ( -104.6228709571500559, -24.35013146730204170, 9.818937971375104823 ) ) ;
#94953 = CARTESIAN_POINT ( 'NONE',  ( -35.53623699164313621, -24.52300882791529446, 0.6510814631126419227 ) ) ;
#94954 = DIRECTION ( 'NONE',  ( 0.000000000000000000, 1.408054769461693696E-16, -1.000000000000000000 ) ) ;
#94955 = DIRECTION ( 'NONE',  ( 0.000000000000000000, -2.173523156925980399E-06, 0.9999999999976378895 ) ) ;
#94956 = CARTESIAN_POINT ( 'NONE',  ( -73.62362702054829811, -24.65952944569304606, 1.056160979905700126 ) ) ;
#94957 = PLANE ( 'NONE',  #44581 ) ;
#94958 = EDGE_CURVE ( 'NONE', #26695, #21027, #44410, .T. ) ;
#94959 = CARTESIAN_POINT ( 'NONE',  ( -73.62287095715009855, -24.34917612406837861, 0.1852690917426641770 ) ) ;
#94960 = VERTEX_POINT ( 'NONE', #98669 ) ;
#94961 = CARTESIAN_POINT ( 'NONE',  ( -6.898722100468609675, -19.10483383855023476, 11.49999999999998934 ) ) ;
#94962 = FACE_OUTER_BOUND ( 'NONE', #79248, .T. ) ;
#94963 = CARTESIAN_POINT ( 'NONE',  ( -127.5556650442294995, -24.15620529776629155, 10.23563542870658694 ) ) ;
#94964 = CARTESIAN_POINT ( 'NONE',  ( -107.5228709571501042, -24.66019654487199730, 8.947790411086115725 ) ) ;
#94965 = VECTOR ( 'NONE', #9130, 1000.000000000000114 ) ;
#94966 = CARTESIAN_POINT ( 'NONE',  ( -2.814730745656462307, 14.91141199530731853, 8.673617379884035472E-16 ) ) ;
#94967 = CARTESIAN_POINT ( 'NONE',  ( -15.68702345270385834, -14.21367052863537417, 11.49999999999999645 ) ) ;
#94968 = CARTESIAN_POINT ( 'NONE',  ( -21.57569705560537088, 4.917917830663471435, -1.500000000000002220 ) ) ;
#94969 = CARTESIAN_POINT ( 'NONE',  ( -18.72588118538106272, -8.511115862834014223, -1.500000000000002220 ) ) ;
#94970 = CIRCLE ( 'NONE', #51241, 1.249999999999998446 ) ;
#94971 = VERTEX_POINT ( 'NONE', #84946 ) ;
#94972 = CARTESIAN_POINT ( 'NONE',  ( 13.91401389203221406, -6.475225279485573360, 27.75920385068456042 ) ) ;
#94973 = VERTEX_POINT ( 'NONE', #70230 ) ;
#94974 = CARTESIAN_POINT ( 'NONE',  ( -54.57824925133036942, -24.65952944569304606, 1.056160979905696573 ) ) ;
#94975 = CARTESIAN_POINT ( 'NONE',  ( -74.62287095715005592, -29.50248528299804818, 1.056150453629036701 ) ) ;
#94976 = ORIENTED_EDGE ( 'NONE', *, *, #44196, .F. ) ;
#94977 = VECTOR ( 'NONE', #65817, 1000.000000000000000 ) ;
#94978 = VERTEX_POINT ( 'NONE', #31656 ) ;
#94979 = AXIS2_PLACEMENT_3D ( 'NONE', #38378, #83551, #76924 ) ;
#94980 = ORIENTED_EDGE ( 'NONE', *, *, #5097, .T. ) ;
#94981 = DIRECTION ( 'NONE',  ( 0.000000000000000000, 2.173523156925980399E-06, -0.9999999999976378895 ) ) ;
#94982 = CARTESIAN_POINT ( 'NONE',  ( 7.139069293134643779, -5.876774720514421624, 20.58118917620081945 ) ) ;
#94983 = CARTESIAN_POINT ( 'NONE',  ( 5.627902640648289712, -5.876774720514413630, 20.02890049923285787 ) ) ;
#94984 = CARTESIAN_POINT ( 'NONE',  ( 7.508984785159893427, -19.29828013722326929, -1.500000000000002220 ) ) ;
#94985 = CIRCLE ( 'NONE', #23714, 0.8500000000000017542 ) ;
#94986 = CARTESIAN_POINT ( 'NONE',  ( -21.63489631200954122, -1.325961216813365429, 11.49999999999999645 ) ) ;
#94987 = EDGE_LOOP ( 'NONE', ( #123, #64066, #23727, #54602 ) ) ;
#94988 = CARTESIAN_POINT ( 'NONE',  ( 32.59332756141815679, 2.682774720514426559, -11.41404606144462086 ) ) ;
#94989 = CARTESIAN_POINT ( 'NONE',  ( -110.4124944177896168, -25.11072899458616803, 2.834579673487489959 ) ) ;
#94990 = CARTESIAN_POINT ( 'NONE',  ( 22.37589550080693712, 1.095942408959037273, 11.49999999999998934 ) ) ;
#94991 = CARTESIAN_POINT ( 'NONE',  ( -47.65344956067661997, -23.73791477778911485, 11.05961554403170766 ) ) ;
#94992 = CARTESIAN_POINT ( 'NONE',  ( -61.52287095715006160, -24.64965694238407323, 8.947790433994201820 ) ) ;
#94993 = ORIENTED_EDGE ( 'NONE', *, *, #32591, .T. ) ;
#94994 = CARTESIAN_POINT ( 'NONE',  ( 29.75874681941402855, 6.376774720514429617, 26.36094095093186596 ) ) ;
#94995 = CARTESIAN_POINT ( 'NONE',  ( 32.60294298177596062, -6.475225279485573360, -11.48871326860665043 ) ) ;
#94996 = ORIENTED_EDGE ( 'NONE', *, *, #16020, .F. ) ;
#94997 = B_SPLINE_CURVE_WITH_KNOTS ( 'NONE', 3,
 ( #73384, #96703, #21070, #44431 ),
 .UNSPECIFIED., .F., .F.,
 ( 4, 4 ),
 ( 0.6792605734346469637, 0.6802613204754125453 ),
 .UNSPECIFIED. ) ;
#94998 = ORIENTED_EDGE ( 'NONE', *, *, #34804, .F. ) ;
#94999 = CARTESIAN_POINT ( 'NONE',  ( -70.92287095715008149, -23.47596703998600631, 11.44779298504227683 ) ) ;
#95000 = VERTEX_POINT ( 'NONE', #62628 ) ;
#95001 = CARTESIAN_POINT ( 'NONE',  ( -101.5228709571500758, -23.47596703998600631, 11.44779298504228215 ) ) ;
#95002 = EDGE_CURVE ( 'NONE', #76045, #32852, #45902, .T. ) ;
#95003 = CARTESIAN_POINT ( 'NONE',  ( 20.49604761983493972, 5.601127818285958071, -1.500000000000002220 ) ) ;
#95004 = B_SPLINE_CURVE_WITH_KNOTS ( 'NONE', 3,
 ( #76886, #53093, #37364, #54092, #24115, #61210, #22111, #99725 ),
 .UNSPECIFIED., .F., .F.,
 ( 4, 2, 2, 4 ),
 ( -0.001224554619866354303, -0.0002241820295893731229, 0.0007761905606876080572, 0.002776935741241574537 ),
 .UNSPECIFIED. ) ;
#95005 = ORIENTED_EDGE ( 'NONE', *, *, #55442, .F. ) ;
#95006 = CARTESIAN_POINT ( 'NONE',  ( -50.47721621591080066, -24.92564183028979130, 1.928384488918255535 ) ) ;
#95007 = EDGE_CURVE ( 'NONE', #15801, #45491, #24446, .T. ) ;
#95008 = CARTESIAN_POINT ( 'NONE',  ( -19.11951126197014261, -10.51958540666066533, 11.49999999999998934 ) ) ;
#95009 = CARTESIAN_POINT ( 'NONE',  ( -103.5510008564771454, -24.35071581493543391, 9.817618358456027039 ) ) ;
#95010 = CARTESIAN_POINT ( 'NONE',  ( -107.5228709571501042, -23.47593901973090524, -1.443836447538996426 ) ) ;
#95011 = DIRECTION ( 'NONE',  ( 0.000000000000000000, -2.173523156925980399E-06, 0.9999999999976378895 ) ) ;
#95012 = CARTESIAN_POINT ( 'NONE',  ( 3.337383349182757364, -21.60657791699550856, -1.500000000000002220 ) ) ;
#95013 = CARTESIAN_POINT ( 'NONE',  ( -30.57287095715005165, -24.38734503390291053, 9.674897050867153681 ) ) ;
#95014 = ORIENTED_EDGE ( 'NONE', *, *, #1690, .F. ) ;
#95015 = FACE_OUTER_BOUND ( 'NONE', #70048, .T. ) ;
#95016 = CARTESIAN_POINT ( 'NONE',  ( -85.54661622668413656, -24.52399227489127043, 9.353111116836526406 ) ) ;
#95017 = ORIENTED_EDGE ( 'NONE', *, *, #42140, .T. ) ;
#95018 = EDGE_CURVE ( 'NONE', #21576, #54707, #3813, .T. ) ;
#95019 = CIRCLE ( 'NONE', #39899, 3.060000000000000497 ) ;
#95020 = EDGE_CURVE ( 'NONE', #7104, #40542, #23530, .T. ) ;
#95021 = VERTEX_POINT ( 'NONE', #15430 ) ;
#95022 = EDGE_CURVE ( 'NONE', #46454, #38937, #14637, .T. ) ;
#95023 = EDGE_LOOP ( 'NONE', ( #13500, #12351, #89051, #49618 ) ) ;
#95024 = CARTESIAN_POINT ( 'NONE',  ( -89.43576144935767047, -25.12049752546737835, 2.832404795212221771 ) ) ;
#95025 = ADVANCED_FACE ( 'NONE', ( #7823 ), #47398, .T. ) ;
#95026 = CARTESIAN_POINT ( 'NONE',  ( -82.59968302428518427, -23.73766607897671221, -1.055555164236435362 ) ) ;
#95027 = CARTESIAN_POINT ( 'NONE',  ( 18.67678363807796416, 10.12720680154768971, -1.500000000000002220 ) ) ;
#95028 = FACE_OUTER_BOUND ( 'NONE', #62294, .T. ) ;
#95029 = CARTESIAN_POINT ( 'NONE',  ( -30.59800378598952264, -24.75991027412949563, 1.063373454495736725 ) ) ;
#95030 = LINE ( 'NONE', #9282, #76124 ) ;
#95031 = DIRECTION ( 'NONE',  ( 0.000000000000000000, 0.000000000000000000, -1.000000000000000000 ) ) ;
#95032 = CARTESIAN_POINT ( 'NONE',  ( 7.147005326088517130, -18.03964237587283037, -1.500000000000002220 ) ) ;
#95033 = CARTESIAN_POINT ( 'NONE',  ( -45.62627816233564459, -24.92564183028979130, 1.928384488918256645 ) ) ;
#95034 = EDGE_LOOP ( 'NONE', ( #85310, #89024, #9682, #87858 ) ) ;
#95035 = CARTESIAN_POINT ( 'NONE',  ( 16.17817332762582794, -10.88531698672339942, 11.49999999999999645 ) ) ;
#95036 = CARTESIAN_POINT ( 'NONE',  ( -5.382328594919684406, -5.876774720514411854, 19.61227901093090864 ) ) ;
#95037 = CARTESIAN_POINT ( 'NONE',  ( 16.26279755680689476, -5.965225279485572685, -27.67997040356619110 ) ) ;
#95038 = EDGE_CURVE ( 'NONE', #79658, #8748, #38770, .T. ) ;
#95039 = ORIENTED_EDGE ( 'NONE', *, *, #8668, .T. ) ;
#95040 = CARTESIAN_POINT ( 'NONE',  ( 4.736659488006659480, -5.876774720514419847, 21.25082490164487581 ) ) ;
#95041 = CARTESIAN_POINT ( 'NONE',  ( 31.79364159983995464, -6.376774720514426953, -11.59305536555894278 ) ) ;
#95042 = VECTOR ( 'NONE', #21523, 1000.000000000000000 ) ;
#95043 = LINE ( 'NONE', #11309, #14748 ) ;
#95044 = LINE ( 'NONE', #10310, #70414 ) ;
#95046 = ADVANCED_FACE ( 'NONE', ( #24041 ), #6331, .T. ) ;
#95045 = CARTESIAN_POINT ( 'NONE',  ( 9.421224358276909072, -17.24829524558457194, 11.49999999999998934 ) ) ;
#95047 = B_SPLINE_CURVE_WITH_KNOTS ( 'NONE', 3,
 ( #65342, #57707, #19121, #97252, #79526, #41473 ),
 .UNSPECIFIED., .F., .F.,
 ( 4, 2, 4 ),
 ( 0.000000000000000000, 0.001380764517853253371, 0.002761529035706506742 ),
 .UNSPECIFIED. ) ;
#95048 = ORIENTED_EDGE ( 'NONE', *, *, #8693, .T. ) ;
#95049 = PLANE ( 'NONE',  #22923 ) ;
#95050 = CARTESIAN_POINT ( 'NONE',  ( -22.22199965279648737, -6.226755796435518242, -1.500000000000002220 ) ) ;
#95051 = AXIS2_PLACEMENT_3D ( 'NONE', #62513, #1111, #64040 ) ;
#95052 = B_SPLINE_CURVE_WITH_KNOTS ( 'NONE', 3,
 ( #82256, #51822, #35600, #44208 ),
 .UNSPECIFIED., .F., .F.,
 ( 4, 4 ),
 ( 0.000000000000000000, 9.999999999998897304E-05 ),
 .UNSPECIFIED. ) ;
#95053 = APPROVAL_DATE_TIME ( #64132, #7222 ) ;
#95054 = DIRECTION ( 'NONE',  ( 0.000000000000000000, -2.173523156925980399E-06, 0.9999999999976378895 ) ) ;
#95055 = CARTESIAN_POINT ( 'NONE',  ( -105.6228709571501128, -24.62285846362216191, 9.038163152653526211 ) ) ;
#95056 = CARTESIAN_POINT ( 'NONE',  ( -110.2249299094570034, -25.11071250048269121, 2.834488755612520894 ) ) ;
#95057 = CARTESIAN_POINT ( 'NONE',  ( -29.52287095715006160, -23.38909342368989641, 11.44779306042727285 ) ) ;
#95058 = CARTESIAN_POINT ( 'NONE',  ( -79.91736924226242422, -25.29489613318244068, 6.057562805997258160 ) ) ;
#95059 = CIRCLE ( 'NONE', #28643, 2.249999999999998668 ) ;
#95061 = CARTESIAN_POINT ( 'NONE',  ( 6.326958800731953048, -6.376774720514426065, 21.47849181751607972 ) ) ;
#95060 = AXIS2_PLACEMENT_3D ( 'NONE', #37702, #21960, #93476 ) ;
#95062 = FACE_OUTER_BOUND ( 'NONE', #7871, .T. ) ;
#95063 = B_SPLINE_CURVE_WITH_KNOTS ( 'NONE', 3,
 ( #86566, #7937, #63247, #94171 ),
 .UNSPECIFIED., .F., .F.,
 ( 4, 4 ),
 ( 1.734723475976806902E-18, 0.002763707449907618768 ),
 .UNSPECIFIED. ) ;
#95064 = CARTESIAN_POINT ( 'NONE',  ( -2.499999999999993339, 18.99999999999977618, 0.000000000000000000 ) ) ;
#95065 = CARTESIAN_POINT ( 'NONE',  ( -19.25010300378637851, 5.133817055790010464, 11.49999999999998934 ) ) ;
#95066 = CARTESIAN_POINT ( 'NONE',  ( -100.5388770704638546, -25.19555990040513294, 3.297675640329406743 ) ) ;
#95067 = CARTESIAN_POINT ( 'NONE',  ( 12.34629653512297409, 15.52844579862587437, -1.500000000000002220 ) ) ;
#95068 = VERTEX_POINT ( 'NONE', #53524 ) ;
#95069 = CIRCLE ( 'NONE', #5908, 129.7684398600581517 ) ;
#95070 = CARTESIAN_POINT ( 'NONE',  ( -77.62287095715005592, -29.50248528299804818, 1.056150453629038477 ) ) ;
#95071 = ADVANCED_FACE ( 'NONE', ( #84447 ), #38271, .T. ) ;
#95072 = CARTESIAN_POINT ( 'NONE',  ( -104.6228709571500559, -24.64965695001468404, 8.947790433994178727 ) ) ;
#95073 = DIRECTION ( 'NONE',  ( 0.9685340172660600322, 0.000000000000000000, -0.2488812114211667037 ) ) ;
#95074 = CARTESIAN_POINT ( 'NONE',  ( 20.75994597877129877, -1.272245555857973054, 11.49999999999999645 ) ) ;
#95075 = CARTESIAN_POINT ( 'NONE',  ( -81.56339547467169382, -23.48783264082478084, -1.443836473390067043 ) ) ;
#95076 = ADVANCED_FACE ( 'NONE', ( #45406 ), #87355, .T. ) ;
#95077 = DIRECTION ( 'NONE',  ( -0.000000000000000000, -0.000000000000000000, -1.000000000000000000 ) ) ;
#95078 = CARTESIAN_POINT ( 'NONE',  ( 10.87194125936840194, 20.03610521102953257, 11.49999999999999645 ) ) ;
#95079 = ORIENTED_EDGE ( 'NONE', *, *, #71318, .T. ) ;
#95080 = CARTESIAN_POINT ( 'NONE',  ( -111.9228709571500815, -23.47596703998600631, 11.44779298504227860 ) ) ;
#95081 = FACE_OUTER_BOUND ( 'NONE', #44467, .T. ) ;
#95082 = ORIENTED_EDGE ( 'NONE', *, *, #28695, .T. ) ;
#95083 = CARTESIAN_POINT ( 'NONE',  ( -18.82339984186270598, 7.397194320553815317, 11.49999999999998934 ) ) ;
#95084 = CARTESIAN_POINT ( 'NONE',  ( 7.475222833218381879, -5.876774720514418959, 20.91460388675487891 ) ) ;
#95085 = CARTESIAN_POINT ( 'NONE',  ( -49.58953762381673158, -24.65952944569304606, 1.056160979905694575 ) ) ;
#95086 = AXIS2_PLACEMENT_3D ( 'NONE', #72172, #2663, #66076 ) ;
#95087 = CARTESIAN_POINT ( 'NONE',  ( -106.6228709571500559, -24.64898659630368627, 1.056161002820831474 ) ) ;
#95088 = VERTEX_POINT ( 'NONE', #77815 ) ;
#95089 = CARTESIAN_POINT ( 'NONE',  ( -127.5228709571500900, -24.51283580621365843, 0.6167428607019854736 ) ) ;
#95090 = CARTESIAN_POINT ( 'NONE',  ( -100.6228709571500843, -23.84047902841604483, -0.8780736468305493370 ) ) ;
#95091 = CARTESIAN_POINT ( 'NONE',  ( -12.65591448191638335, 15.52279176289047236, -1.500000000000002220 ) ) ;
#95092 = CARTESIAN_POINT ( 'NONE',  ( -36.62287095715007723, -24.33927499327853639, 9.819080762295818943 ) ) ;
#95093 = CARTESIAN_POINT ( 'NONE',  ( -18.84683179826791743, -9.195131953753229226, 11.49999999999999645 ) ) ;
#95094 = VECTOR ( 'NONE', #72830, 1000.000000000000000 ) ;
#95095 = CARTESIAN_POINT ( 'NONE',  ( 8.573524122111766843, 5.965225279485574461, -28.10203366675327175 ) ) ;
#95096 = CYLINDRICAL_SURFACE ( 'NONE', #87010, 2.500000000000000444 ) ;
#95097 = CARTESIAN_POINT ( 'NONE',  ( 13.08019894233326319, 17.74467248152726384, -1.500000000000002220 ) ) ;
#95098 = LINE ( 'NONE', #25583, #33345 ) ;
#95099 = ORIENTED_EDGE ( 'NONE', *, *, #54719, .T. ) ;
#95100 = LINE ( 'NONE', #56558, #84086 ) ;
#95101 = FACE_OUTER_BOUND ( 'NONE', #12984, .T. ) ;
#95102 = CARTESIAN_POINT ( 'NONE',  ( -72.49564566603571336, -24.65952944569304250, 1.056160979905695463 ) ) ;
#95103 = VERTEX_POINT ( 'NONE', #39270 ) ;
#95104 = CARTESIAN_POINT ( 'NONE',  ( 2.628295812946869425, -6.376774720514411854, 19.40849182188139110 ) ) ;
#95105 = ORIENTED_EDGE ( 'NONE', *, *, #62977, .T. ) ;
#95106 = ORIENTED_EDGE ( 'NONE', *, *, #32029, .F. ) ;
#95107 = PLANE ( 'NONE',  #19470 ) ;
#95108 = CARTESIAN_POINT ( 'NONE',  ( -100.5578068411443837, -25.10935802950346130, 2.834635647046928941 ) ) ;
#95109 = CARTESIAN_POINT ( 'NONE',  ( -11.64875734969026233, 5.965225279485572685, 31.02402280011862246 ) ) ;
#95110 = CARTESIAN_POINT ( 'NONE',  ( -10.27258457790969892, -17.75692283049141196, -1.500000000000002220 ) ) ;
#95111 = ORIENTED_EDGE ( 'NONE', *, *, #46604, .T. ) ;
#95112 = LINE ( 'NONE', #64698, #44521 ) ;
#95113 = CARTESIAN_POINT ( 'NONE',  ( 7.087697398486194622, -5.876774720514418959, 20.45710073441444621 ) ) ;
#95114 = CARTESIAN_POINT ( 'NONE',  ( -41.52287095715006870, -24.64965694238406613, 8.947790433994205372 ) ) ;
#95115 = CARTESIAN_POINT ( 'NONE',  ( -18.01732314745861530, 13.19606014829601826, 11.49999999999998934 ) ) ;
#95116 = VECTOR ( 'NONE', #44498, 1000.000000000000000 ) ;
#95117 = B_SPLINE_CURVE_WITH_KNOTS ( 'NONE', 3,
 ( #87968, #73246, #65159, #96080 ),
 .UNSPECIFIED., .F., .F.,
 ( 4, 4 ),
 ( 0.2899930013815662511, 0.2989994326536817293 ),
 .UNSPECIFIED. ) ;
#95118 = DIRECTION ( 'NONE',  ( -0.3133898629642186684, 4.164321980682960499E-15, 0.9496245541219267006 ) ) ;
#95119 = CARTESIAN_POINT ( 'NONE',  ( -2.070328576748420524, -5.876774720514410966, 19.46575348430201657 ) ) ;
#95120 = VERTEX_POINT ( 'NONE', #31158 ) ;
#95121 = CARTESIAN_POINT ( 'NONE',  ( -42.62287095715004881, -23.47593901973091235, -1.443836447539011525 ) ) ;
#95122 = CARTESIAN_POINT ( 'NONE',  ( 19.75748517575715368, 0.3587747205144265483, 28.87153971905864580 ) ) ;
#95123 = CARTESIAN_POINT ( 'NONE',  ( 20.57277012135545036, 3.371850554975475145, 11.49999999999998934 ) ) ;
#95124 = ORIENTED_EDGE ( 'NONE', *, *, #62565, .F. ) ;
#95126 = ORIENTED_EDGE ( 'NONE', *, *, #16359, .T. ) ;
#95125 = CARTESIAN_POINT ( 'NONE',  ( -79.52287095715009002, -24.51387760970724372, 9.387446482453409402 ) ) ;
#95127 = ORIENTED_EDGE ( 'NONE', *, *, #16553, .F. ) ;
#95128 = EDGE_CURVE ( 'NONE', #10120, #17101, #95806, .T. ) ;
#95129 = CARTESIAN_POINT ( 'NONE',  ( -33.55620429048339304, -23.47593901973091235, -1.443836447539013301 ) ) ;
#95130 = CARTESIAN_POINT ( 'NONE',  ( -5.931750313267273533, -20.21149935180699231, -1.500000000000002220 ) ) ;
#95131 = EDGE_LOOP ( 'NONE', ( #47834, #21068, #21653, #36648 ) ) ;
#95132 = VECTOR ( 'NONE', #49463, 1000.000000000000000 ) ;
#95133 = CARTESIAN_POINT ( 'NONE',  ( -93.62287095715005592, -23.48786465467241769, 11.44779295918254114 ) ) ;
#95135 = EDGE_CURVE ( 'NONE', #28096, #51004, #72822, .T. ) ;
#95134 = DIRECTION ( 'NONE',  ( 0.000000000000000000, 1.000000000000000000, 0.000000000000000000 ) ) ;
#95136 = CARTESIAN_POINT ( 'NONE',  ( -120.5880710595450722, -24.92592662359561118, 8.075495903017998245 ) ) ;
#95137 = VECTOR ( 'NONE', #27632, 1000.000000000000114 ) ;
#95138 = CARTESIAN_POINT ( 'NONE',  ( 30.58729439590577570, 4.540774720514427543, 26.14186284044645703 ) ) ;
#95139 = CARTESIAN_POINT ( 'NONE',  ( -110.3139465455115271, -25.12049752546738191, 2.832404795212222659 ) ) ;
#95140 = CARTESIAN_POINT ( 'NONE',  ( -5.395268184683536639, 21.00466093859614958, -1.500000000000002220 ) ) ;
#95141 = CARTESIAN_POINT ( 'NONE',  ( -57.52287095715004739, -23.96127896941631974, -0.6493128931038052443 ) ) ;
#95143 = ORIENTED_EDGE ( 'NONE', *, *, #51643, .T. ) ;
#95142 = CARTESIAN_POINT ( 'NONE',  ( 7.688942331755139747, 20.87172568467934752, 11.49999999999999645 ) ) ;
#95144 = CARTESIAN_POINT ( 'NONE',  ( -51.34258402508250185, -25.24728821302171156, 5.647563055808960009 ) ) ;
#95145 = CARTESIAN_POINT ( 'NONE',  ( -70.93618602633573289, -25.29670723202037408, 5.474567338846606290 ) ) ;
#95146 = ORIENTED_EDGE ( 'NONE', *, *, #41073, .F. ) ;
#95147 = EDGE_CURVE ( 'NONE', #5623, #47484, #16425, .T. ) ;
#95148 = EDGE_CURVE ( 'NONE', #10079, #31190, #50958, .T. ) ;
#95150 = ORIENTED_EDGE ( 'NONE', *, *, #85406, .F. ) ;
#95149 = DIRECTION ( 'NONE',  ( 0.000000000000000000, 0.000000000000000000, 1.000000000000000000 ) ) ;
#95151 = ADVANCED_FACE ( 'NONE', ( #18932 ), #78324, .T. ) ;
#95152 = ORIENTED_EDGE ( 'NONE', *, *, #44173, .T. ) ;
#95153 = ADVANCED_FACE ( 'NONE', ( #65144 ), #35552, .T. ) ;
#95154 = CARTESIAN_POINT ( 'NONE',  ( 31.73616390345410920, -3.909076239803030539, -3.851095480477756627 ) ) ;
#95155 = CARTESIAN_POINT ( 'NONE',  ( -1.972954090310384379, -20.06304030521763337, 11.49999999999998934 ) ) ;
#95156 = DIRECTION ( 'NONE',  ( 0.000000000000000000, 0.000000000000000000, -1.000000000000000000 ) ) ;
#95157 = ORIENTED_EDGE ( 'NONE', *, *, #26986, .F. ) ;
#95158 = CARTESIAN_POINT ( 'NONE',  ( -130.5728709571500588, -24.78459947536195429, 1.143784119390943266 ) ) ;
#95159 = CARTESIAN_POINT ( 'NONE',  ( -1.986123035288760885, 22.30159847666916662, -1.500000000000002220 ) ) ;
#95160 = VERTEX_POINT ( 'NONE', #56018 ) ;
#95161 = ORIENTED_EDGE ( 'NONE', *, *, #41567, .T. ) ;
#95162 = CARTESIAN_POINT ( 'NONE',  ( -112.5540285387501171, -24.15620529776628445, 10.23563542870659404 ) ) ;
#95163 = CARTESIAN_POINT ( 'NONE',  ( -101.5550256582385344, -23.96169478059713853, 10.65365249895717881 ) ) ;
#95164 = CARTESIAN_POINT ( 'NONE',  ( -61.52287095715006160, -24.64965694238407323, 8.947790433994201820 ) ) ;
#95165 = AXIS2_PLACEMENT_3D ( 'NONE', #80271, #96995, #43223 ) ;
#95166 = CARTESIAN_POINT ( 'NONE',  ( -41.52287095715006870, -24.65952944569304606, 1.056160979905691910 ) ) ;
#95167 = CARTESIAN_POINT ( 'NONE',  ( -63.90635886673450017, -25.30559561715417871, 6.147794833475641596 ) ) ;
#95168 = CARTESIAN_POINT ( 'NONE',  ( -6.365771329251782795, -18.49506561991874065, -1.500000000000002220 ) ) ;
#95169 = B_SPLINE_SURFACE_WITH_KNOTS ( 'NONE', 3, 3, ( 
 ( #84885, #6761, #7256, #46837 ),
 ( #69166, #99103, #45837, #29600 ),
 ( #47337, #68675, #53956, #8772 ),
 ( #99595, #39709, #83887, #91496 ),
 ( #60579, #31097, #46330, #21974 ),
 ( #30098, #52956, #77261, #91999 ),
 ( #154, #53460, #14369, #76756 ) ),
 .UNSPECIFIED., .F., .F., .F.,
 ( 4, 3, 4 ),
 ( 4, 4 ),
 ( 0.7945040050992241421, 0.8970133687736498995, 0.9995227324480755460 ),
 ( 0.2095472461047292734, 0.2106567115738801899 ),
 .UNSPECIFIED. ) ;
#95170 = CARTESIAN_POINT ( 'NONE',  ( -50.38822539166535108, -25.31267346029541088, 4.736250531364077254 ) ) ;
#95171 = ORIENTED_EDGE ( 'NONE', *, *, #45430, .F. ) ;
#95172 = CARTESIAN_POINT ( 'NONE',  ( -17.55493245422511350, -12.44833567967518029, -1.500000000000002220 ) ) ;
#95173 = AXIS2_PLACEMENT_3D ( 'NONE', #90541, #82428, #12912 ) ;
#95174 = CARTESIAN_POINT ( 'NONE',  ( -129.5895376238167387, -24.64965694238408034, 8.947790433994645909 ) ) ;
#95175 = DIRECTION ( 'NONE',  ( -0.9890158633619159367, -0.1478094111296165691, -0.000000000000000000 ) ) ;
#95176 = LINE ( 'NONE', #48513, #81433 ) ;
#95177 = LINE ( 'NONE', #89067, #29337 ) ;
#95178 = CARTESIAN_POINT ( 'NONE',  ( 5.768980952343642166, -22.17701263744951490, -1.500000000000002220 ) ) ;
#95179 = COORDINATED_UNIVERSAL_TIME_OFFSET ( 0, 0, .AHEAD. ) ;
#95180 = CARTESIAN_POINT ( 'NONE',  ( 22.02124265030973760, -6.143225279485574397, 16.20402280011862217 ) ) ;
#95181 = CARTESIAN_POINT ( 'NONE',  ( -53.56762332262419335, -23.48783264082476663, -1.443836473390096353 ) ) ;
#95182 = CARTESIAN_POINT ( 'NONE',  ( -14.83682921977595548, 13.52632505182701017, 11.49999999999999645 ) ) ;
#95183 = CARTESIAN_POINT ( 'NONE',  ( -127.6228709571500559, -29.50250243563736774, 8.947779886222132717 ) ) ;
#95184 = CARTESIAN_POINT ( 'NONE',  ( -32.62928502708932399, -24.51419770103159834, 9.386484678747182286 ) ) ;
#95185 = PRODUCT_DEFINITION_SHAPE ( 'NONE', 'NONE',  #30849 ) ;
#95186 = CARTESIAN_POINT ( 'NONE',  ( -121.6228709571499991, -23.95044443724992078, 10.65354141964649237 ) ) ;
#95187 = CARTESIAN_POINT ( 'NONE',  ( 8.160000000000000142, -10.15233964170348457, 1.310587897985993955 ) ) ;
#95188 = CARTESIAN_POINT ( 'NONE',  ( -50.62287095715005592, -23.48786465467241058, 11.44779295918255180 ) ) ;
#95189 = CARTESIAN_POINT ( 'NONE',  ( 19.75055111929153639, -1.948201398878238066, 11.49999999999998934 ) ) ;
#95190 = CARTESIAN_POINT ( 'NONE',  ( -94.52287095715004739, -24.50321055353806088, 9.387540953477534700 ) ) ;
#95191 = CARTESIAN_POINT ( 'NONE',  ( 19.40334540789412188, 3.064012487144803565, -1.500000000000002220 ) ) ;
#95192 = VECTOR ( 'NONE', #50254, 1000.000000000000000 ) ;
#95193 = CARTESIAN_POINT ( 'NONE',  ( -75.62287095715005592, -23.48786465467241058, 11.44779295918254647 ) ) ;
#95194 = CARTESIAN_POINT ( 'NONE',  ( 13.10664265030973930, -5.965225279485574461, -28.18129937516157568 ) ) ;
#95195 = SECURITY_CLASSIFICATION_LEVEL ( 'unclassified' ) ;
#95196 = CARTESIAN_POINT ( 'NONE',  ( 15.97264542221207151, 3.406413700670978262, -27.93485542787877662 ) ) ;
#95197 = CARTESIAN_POINT ( 'NONE',  ( 2.598243466966731585, -5.876774720514414518, 20.31174627870924709 ) ) ;
#95198 = CARTESIAN_POINT ( 'NONE',  ( -11.86786554430972096, -16.85652113839894639, 11.49999999999999645 ) ) ;
#95199 = DIRECTION ( 'NONE',  ( 0.5656310827093757876, -0.8246584009594636333, -1.161164194647627127E-16 ) ) ;
#95200 = ADVANCED_FACE ( 'NONE', ( #87450 ), #17943, .F. ) ;
#95201 = LINE ( 'NONE', #25684, #96661 ) ;
#95202 = CARTESIAN_POINT ( 'NONE',  ( 22.41689761077644860, -2.907977976681301424, 11.49999999999999645 ) ) ;
#95203 = ORIENTED_EDGE ( 'NONE', *, *, #14542, .T. ) ;
#95204 = EDGE_CURVE ( 'NONE', #85400, #70110, #80337, .T. ) ;
#95205 = CARTESIAN_POINT ( 'NONE',  ( -69.34384048089543739, -25.25639414125907578, 6.239613344031938347 ) ) ;
#95206 = FACE_OUTER_BOUND ( 'NONE', #43584, .T. ) ;
#95207 = CARTESIAN_POINT ( 'NONE',  ( -109.6228709571500559, -24.50321055353806443, 9.387540953477524042 ) ) ;
#95208 = DIRECTION ( 'NONE',  ( 0.000000000000000000, 1.000000000000000000, 0.000000000000000000 ) ) ;
#95209 = VECTOR ( 'NONE', #59597, 1000.000000000000000 ) ;
#95210 = CARTESIAN_POINT ( 'NONE',  ( -110.6228709571500559, -24.99156045073393173, 7.747789690856161648 ) ) ;
#95211 = CARTESIAN_POINT ( 'NONE',  ( 1.305682803664691249, 5.965225279485572685, 29.57950906855421991 ) ) ;
#95212 = B_SPLINE_CURVE_WITH_KNOTS ( 'NONE', 3,
 ( #74136, #36069, #20324, #4629 ),
 .UNSPECIFIED., .F., .F.,
 ( 4, 4 ),
 ( 0.000000000000000000, 9.999999999998897304E-05 ),
 .UNSPECIFIED. ) ;
#95213 = VERTEX_POINT ( 'NONE', #5706 ) ;
#95214 = CARTESIAN_POINT ( 'NONE',  ( -80.39192082756260049, -25.26749876446105958, 4.967919919415041186 ) ) ;
#95215 = CARTESIAN_POINT ( 'NONE',  ( -21.19308438721250099, -8.479022899233653376, 11.49999999999998934 ) ) ;
#95216 = CARTESIAN_POINT ( 'NONE',  ( -98.52287095715006160, -24.64965694238575011, 8.947790433994194714 ) ) ;
#95217 = DIRECTION ( 'NONE',  ( 0.000000000000000000, 0.9999999999976377785, 2.173523156925979975E-06 ) ) ;
#95218 = CARTESIAN_POINT ( 'NONE',  ( -82.64080038552411622, -23.73791477778911840, 11.05961554403170766 ) ) ;
#95219 = CARTESIAN_POINT ( 'NONE',  ( 11.54466316424315231, -19.26756404802103972, 11.49999999999999645 ) ) ;
#95220 = ORIENTED_EDGE ( 'NONE', *, *, #86105, .T. ) ;
#95221 = DIRECTION ( 'NONE',  ( -3.773278334453080206E-23, 0.9999999999976377785, 2.173523156925979975E-06 ) ) ;
#95222 = CARTESIAN_POINT ( 'NONE',  ( 16.22650188657148362, -14.79325693486936188, -1.500000000000002220 ) ) ;
#95223 = CARTESIAN_POINT ( 'NONE',  ( -124.4728709570020015, -25.40556190190858388, 4.804048521347549006 ) ) ;
#95224 = CARTESIAN_POINT ( 'NONE',  ( -34.50428818987079893, -23.96169478059712077, 10.65365249895718769 ) ) ;
#95225 = CARTESIAN_POINT ( 'NONE',  ( -66.62287095715005592, -29.50248528299804818, 1.056150453629036701 ) ) ;
#95226 = EDGE_LOOP ( 'NONE', ( #28452, #45716, #55572, #93587 ) ) ;
#95227 = DIRECTION ( 'NONE',  ( -3.773278334453079030E-23, 0.9999999999976377785, 2.173523156925979128E-06 ) ) ;
#95228 = CARTESIAN_POINT ( 'NONE',  ( -36.62287095715005592, -29.50248528299804818, 1.056150453629031594 ) ) ;
#95229 = ORIENTED_EDGE ( 'NONE', *, *, #65178, .F. ) ;
#95230 = CARTESIAN_POINT ( 'NONE',  ( -17.09319154528168383, -11.34935287704045948, -1.500000000000002220 ) ) ;
#95231 = ORIENTED_EDGE ( 'NONE', *, *, #61451, .F. ) ;
#95232 = ORIENTED_EDGE ( 'NONE', *, *, #14721, .T. ) ;
#95233 = VERTEX_POINT ( 'NONE', #60016 ) ;
#95234 = ORIENTED_EDGE ( 'NONE', *, *, #66535, .T. ) ;
#95235 = DIRECTION ( 'NONE',  ( 0.000000000000000000, 0.000000000000000000, -1.000000000000000000 ) ) ;
#95236 = CARTESIAN_POINT ( 'NONE',  ( 1.767912858038628965, -23.04938964843747584, 11.49999999999998934 ) ) ;
#95237 = CARTESIAN_POINT ( 'NONE',  ( 14.67302116299745052, 4.477500275188335266, -27.99481486150953558 ) ) ;
#95238 = CARTESIAN_POINT ( 'NONE',  ( -18.18203184671642703, 9.085611141607108365, -1.500000000000002220 ) ) ;
#95239 = VERTEX_POINT ( 'NONE', #80845 ) ;
#95240 = DIRECTION ( 'NONE',  ( 1.000000000000000000, 3.773278334444167608E-23, 8.201307833595939069E-29 ) ) ;
#95241 = CARTESIAN_POINT ( 'NONE',  ( -29.62953203690532433, -24.43865590823392253, 9.386484716961753350 ) ) ;
#95242 = CARTESIAN_POINT ( 'NONE',  ( -114.6228709571500417, -23.48786465467241769, 11.44779295918253936 ) ) ;
#95243 = CARTESIAN_POINT ( 'NONE',  ( 4.281720980632043094, -5.876774720514409189, 18.71132571341777151 ) ) ;
#95245 = ORIENTED_EDGE ( 'NONE', *, *, #25325, .F. ) ;
#95244 = CARTESIAN_POINT ( 'NONE',  ( 2.436486579176012413, 21.40072447632485364, 11.49999999999999645 ) ) ;
#95246 = CARTESIAN_POINT ( 'NONE',  ( -29.24616400714660003, -24.76881415122372232, 4.855717898223424811 ) ) ;
#95247 = CARTESIAN_POINT ( 'NONE',  ( 32.16024265030974050, 5.965225279485572685, 14.03360796525321774 ) ) ;
#95248 = ORIENTED_EDGE ( 'NONE', *, *, #34767, .T. ) ;
#95249 = CARTESIAN_POINT ( 'NONE',  ( -15.76495264167062160, -13.51897010167481739, 11.49999999999998934 ) ) ;
#95250 = ORIENTED_EDGE ( 'NONE', *, *, #92847, .T. ) ;
#95252 = VERTEX_POINT ( 'NONE', #20923 ) ;
#95251 = DIRECTION ( 'NONE',  ( -3.773278334453080206E-23, 0.9999999999976377785, 2.173523156925979975E-06 ) ) ;
#95253 = B_SPLINE_SURFACE_WITH_KNOTS ( 'NONE', 3, 3, ( 
 ( #21083, #6862, #68272, #100179 ),
 ( #83480, #44944, #84484, #60671 ),
 ( #14966, #45937, #99201, #29207 ),
 ( #92094, #29701, #36324, #28712 ),
 ( #59673, #61173, #91594, #7351 ),
 ( #75866, #37814, #68769, #90602 ),
 ( #52049, #82979, #30697, #53055 ),
 ( #6368, #99686, #37328, #23064 ),
 ( #83984, #13470, #14463, #61669 ),
 ( #84979, #44441, #45445, #5865 ) ),
 .UNSPECIFIED., .F., .F., .F.,
 ( 4, 3, 3, 4 ),
 ( 4, 4 ),
 ( 0.7022005934544808259, 0.7765311282028795059, 0.8508616629512781859, 0.9995227324480756570 ),
 ( 0.2495241106790039021, 0.2506855486834824731 ),
 .UNSPECIFIED. ) ;
#95254 = CARTESIAN_POINT ( 'NONE',  ( -110.9909297185884327, -29.50249817218807635, 6.986241424688308221 ) ) ;
#95255 = PLANE ( 'NONE',  #48702 ) ;
#95256 = ORIENTED_EDGE ( 'NONE', *, *, #9570, .T. ) ;
#95257 = EDGE_LOOP ( 'NONE', ( #2291, #40117, #26350, #73785, #24134, #60659, #89367, #70793, #17725, #61070 ) ) ;
#95258 = DIRECTION ( 'NONE',  ( -3.773278334453079618E-23, 0.9999999999976377785, 2.173523156925979975E-06 ) ) ;
#95259 = EDGE_CURVE ( 'NONE', #60428, #55518, #17692, .T. ) ;
#95260 = CARTESIAN_POINT ( 'NONE',  ( 29.73860345376319358, -3.356774720514427379, 1.647607965253213180 ) ) ;
#95261 = DIRECTION ( 'NONE',  ( -3.773278334453079618E-23, 0.9999999999976377785, 2.173523156925979975E-06 ) ) ;
#95263 = ORIENTED_EDGE ( 'NONE', *, *, #33994, .F. ) ;
#95262 = CARTESIAN_POINT ( 'NONE',  ( 9.413913215453616701, -19.89622248225912315, 11.49999999999999645 ) ) ;
#95264 = CARTESIAN_POINT ( 'NONE',  ( -103.5098641677505213, -24.65952944569305316, 1.056160979905703234 ) ) ;
#95265 = EDGE_CURVE ( 'NONE', #84023, #14758, #70282, .T. ) ;
#95266 = CARTESIAN_POINT ( 'NONE',  ( 14.59886444729927923, 17.24780449347180067, 11.49999999999998934 ) ) ;
#95267 = VECTOR ( 'NONE', #94672, 1000.000000000000000 ) ;
#95268 = EDGE_CURVE ( 'NONE', #54952, #5853, #90446, .T. ) ;
#95270 = ORIENTED_EDGE ( 'NONE', *, *, #95022, .T. ) ;
#95269 = CARTESIAN_POINT ( 'NONE',  ( -62.52287095715006160, -23.47593901973090169, -1.443836447538997092 ) ) ;
#95271 = EDGE_CURVE ( 'NONE', #47459, #20866, #100029, .T. ) ;
#95272 = VERTEX_POINT ( 'NONE', #30540 ) ;
#95273 = ADVANCED_FACE ( 'NONE', ( #31539 ), #8214, .T. ) ;
#95274 = CARTESIAN_POINT ( 'NONE',  ( -83.52287095715001897, -24.66019654487199375, 8.947790411086122830 ) ) ;
#95275 = VECTOR ( 'NONE', #89999, 1000.000000000000114 ) ;
#95276 = CARTESIAN_POINT ( 'NONE',  ( -86.62287095715004170, -23.48783264082478794, -1.443836473390063713 ) ) ;
#95277 = VERTEX_POINT ( 'NONE', #31037 ) ;
#95278 = CARTESIAN_POINT ( 'NONE',  ( -16.93204426113827310, 12.72334981527875186, -1.500000000000002220 ) ) ;
#95279 = CARTESIAN_POINT ( 'NONE',  ( -82.62287095715008434, -24.51283580621365132, 0.6167428607019763698 ) ) ;
#95280 = CARTESIAN_POINT ( 'NONE',  ( 30.61317826727886526, -3.861502214243257125, 27.24847364799711613 ) ) ;
#95281 = VECTOR ( 'NONE', #90909, 1000.000000000000114 ) ;
#95282 = CARTESIAN_POINT ( 'NONE',  ( -7.264088518202086675, -6.376774720514411854, 19.78976258633487717 ) ) ;
#95283 = CARTESIAN_POINT ( 'NONE',  ( -40.84407949893366663, -25.29514021929367118, 5.506588697105319952 ) ) ;
#95284 = CARTESIAN_POINT ( 'NONE',  ( -21.61287440533560300, 5.199345243644041936, -1.500000000000002220 ) ) ;
#95285 = CARTESIAN_POINT ( 'NONE',  ( -67.62287095715005592, -29.50250243563736774, 8.947779886222143375 ) ) ;
#95286 = EDGE_CURVE ( 'NONE', #46066, #65965, #61854, .T. ) ;
#95287 = ORIENTED_EDGE ( 'NONE', *, *, #5015, .F. ) ;
#95288 = CARTESIAN_POINT ( 'NONE',  ( 14.43441819135927950, 5.965225279485592225, -28.36222020317712378 ) ) ;
#95289 = DIRECTION ( 'NONE',  ( 0.000000000000000000, 0.000000000000000000, -1.000000000000000000 ) ) ;
#95290 = CARTESIAN_POINT ( 'NONE',  ( -15.38109395195050233, 11.78095549196778258, 11.49999999999999645 ) ) ;
#95291 = CARTESIAN_POINT ( 'NONE',  ( -36.65742501572457712, -23.73791477778911130, 11.05961554403171121 ) ) ;
#95292 = DIRECTION ( 'NONE',  ( -5.939352905686045343E-16, 0.000000000000000000, 1.000000000000000000 ) ) ;
#95293 = CARTESIAN_POINT ( 'NONE',  ( 19.19537281719634336, 3.394423509666608663, -1.500000000000002220 ) ) ;
#95294 = CARTESIAN_POINT ( 'NONE',  ( 14.52366289275476419, -15.72616519631134580, -1.500000000000002220 ) ) ;
#95295 = DIRECTION ( 'NONE',  ( -0.4009304992412300317, -0.000000000000000000, -0.9161084732596779245 ) ) ;
#95296 = CARTESIAN_POINT ( 'NONE',  ( -60.60738981642156631, -23.85049219812968602, 10.88485053497088728 ) ) ;
#95297 = FACE_OUTER_BOUND ( 'NONE', #23700, .T. ) ;
#95298 = CARTESIAN_POINT ( 'NONE',  ( -77.62361607832929167, -24.65952944569304606, 1.056160979905701458 ) ) ;
#95299 = CARTESIAN_POINT ( 'NONE',  ( 21.15473741701296362, -8.388382055385795510, -1.500000000000002220 ) ) ;
#95300 = CARTESIAN_POINT ( 'NONE',  ( -6.761595463178257569E-15, -20.60441423650954818, 4.029750837822677845 ) ) ;
#95301 = CARTESIAN_POINT ( 'NONE',  ( -98.51385245561148452, -24.15543982623907482, -0.2315651400026625395 ) ) ;
#95302 = DIRECTION ( 'NONE',  ( 0.000000000000000000, 0.000000000000000000, -1.000000000000000000 ) ) ;
#95303 = CARTESIAN_POINT ( 'NONE',  ( -19.80664267627650688, 2.137978742899185214, 11.49999999999999645 ) ) ;
#95304 = CARTESIAN_POINT ( 'NONE',  ( -123.5911770222576251, -23.73791477778912551, 11.05961554403169878 ) ) ;
#95305 = DIRECTION ( 'NONE',  ( 0.000000000000000000, -1.000000000000000000, -1.020425574104004246E-16 ) ) ;
#95306 = DIRECTION ( 'NONE',  ( -0.8209519386396718632, 0.000000000000000000, -0.5709972981054852736 ) ) ;
#95307 = ORIENTED_EDGE ( 'NONE', *, *, #51044, .F. ) ;
#95308 = LINE ( 'NONE', #32411, #8833 ) ;
#95309 = CARTESIAN_POINT ( 'NONE',  ( -31.23323026593057250, -24.87479601683088148, 8.247789944647561100 ) ) ;
#95310 = CARTESIAN_POINT ( 'NONE',  ( -63.58953762381672448, -23.48786465467241058, 11.44779295918254824 ) ) ;
#95311 = CARTESIAN_POINT ( 'NONE',  ( -12.04083774165243881, -18.01462592983040523, 11.49999999999998934 ) ) ;
#95312 = CARTESIAN_POINT ( 'NONE',  ( -51.91099744296860763, -25.23365410514359652, 6.412898804246325746 ) ) ;
#95313 = CARTESIAN_POINT ( 'NONE',  ( -0.2416374764669896869, -19.45557994585427508, -1.500000000000002220 ) ) ;
#95314 = CARTESIAN_POINT ( 'NONE',  ( -58.62287095715004881, -29.50248528299804818, 1.056150453629034924 ) ) ;
#95315 = B_SPLINE_CURVE_WITH_KNOTS ( 'NONE', 3,
 ( #38280, #44921, #68248, #99663 ),
 .UNSPECIFIED., .F., .F.,
 ( 4, 4 ),
 ( 0.04878993775236183800, 0.04979068479312719064 ),
 .UNSPECIFIED. ) ;
#95316 = EDGE_CURVE ( 'NONE', #93197, #28046, #21912, .T. ) ;
#95317 = ORIENTED_EDGE ( 'NONE', *, *, #42191, .T. ) ;
#95318 = CARTESIAN_POINT ( 'NONE',  ( -102.6228709571500559, -29.50250243563736774, 8.947779886222138046 ) ) ;
#95319 = CARTESIAN_POINT ( 'NONE',  ( 11.27307661227339430, 16.98952936956587934, 11.49999999999999645 ) ) ;
#95320 = PLANE ( 'NONE',  #6724 ) ;
#95321 = ADVANCED_FACE ( 'NONE', ( #46776 ), #97921, .T. ) ;
#95322 = CARTESIAN_POINT ( 'NONE',  ( -59.90086478509797985, -25.28839794021433462, 4.072426394371103875 ) ) ;
#95323 = ORIENTED_EDGE ( 'NONE', *, *, #99023, .F. ) ;
#95324 = DIRECTION ( 'NONE',  ( -0.1311553622875919756, 6.845827386180409975E-16, -0.9913618264504692190 ) ) ;
#95325 = CARTESIAN_POINT ( 'NONE',  ( -8.160000000000000142, -10.15233964170348457, 0.003711184059992174607 ) ) ;
#95326 = CARTESIAN_POINT ( 'NONE',  ( 7.402957069319889172, -6.376774720514418959, 20.34212842306459024 ) ) ;
#95327 = CARTESIAN_POINT ( 'NONE',  ( -125.5228709571500616, -23.48786465467241769, 11.44779295918253581 ) ) ;
#95328 = LINE ( 'NONE', #12458, #44623 ) ;
#95329 = LINE ( 'NONE', #49177, #77582 ) ;
#95330 = ORIENTED_EDGE ( 'NONE', *, *, #84709, .F. ) ;
#95331 = CARTESIAN_POINT ( 'NONE',  ( -66.50542857718694734, -24.15620529776628089, 10.23563542870660470 ) ) ;
#95332 = VECTOR ( 'NONE', #30530, 1000.000000000000000 ) ;
#95333 = CARTESIAN_POINT ( 'NONE',  ( -21.95939045666098366, -6.591442671832903777, 11.49999999999999645 ) ) ;
#95334 = CARTESIAN_POINT ( 'NONE',  ( -12.51292883401962541, 18.98408452820241266, -1.500000000000002220 ) ) ;
#95335 = CARTESIAN_POINT ( 'NONE',  ( 4.885870204371583370, -6.376774720514420736, 20.85936027411790405 ) ) ;
#95336 = CARTESIAN_POINT ( 'NONE',  ( -68.52287095715006160, -24.64965694238407323, 8.947790433994200043 ) ) ;
#95337 = CARTESIAN_POINT ( 'NONE',  ( -7.160000000000000142, -6.754662360505033547, 7.925641719537454222 ) ) ;
#95338 = CARTESIAN_POINT ( 'NONE',  ( -69.90276568578059369, -25.14717367798247594, 7.019980506270512066 ) ) ;
#95339 = CARTESIAN_POINT ( 'NONE',  ( -19.20277006422315225, 10.48866939257135833, 11.49999999999998934 ) ) ;
#95340 = PRODUCT_DEFINITION ( 'UNKNOWN', '', #57026, #6334 ) ;
#95341 = CARTESIAN_POINT ( 'NONE',  ( -69.53738162378759569, -24.66019654487199375, 8.947790411086119278 ) ) ;
#95342 = CARTESIAN_POINT ( 'NONE',  ( -26.26995961867267937, -24.88333753901390466, 3.525190991172063804 ) ) ;
#95343 = LINE ( 'NONE', #22426, #95484 ) ;
#95344 = CARTESIAN_POINT ( 'NONE',  ( -58.60466252300279422, -23.73766607897669800, -1.055555164236457344 ) ) ;
#95345 = ORIENTED_EDGE ( 'NONE', *, *, #21469, .T. ) ;
#95346 = B_SPLINE_CURVE_WITH_KNOTS ( 'NONE', 3,
 ( #50787, #81228, #65533, #26452 ),
 .UNSPECIFIED., .F., .F.,
 ( 4, 4 ),
 ( 0.5992008101734043191, 0.6002015572141699007 ),
 .UNSPECIFIED. ) ;
#95347 = AXIS2_PLACEMENT_3D ( 'NONE', #35559, #5594, #59388 ) ;
#95348 = CARTESIAN_POINT ( 'NONE',  ( -20.22731604866883970, -2.807383831903240257, 11.49999999999998934 ) ) ;
#95349 = VERTEX_POINT ( 'NONE', #78696 ) ;
#95350 = VERTEX_POINT ( 'NONE', #78204 ) ;
#95351 = CARTESIAN_POINT ( 'NONE',  ( 8.869223403490039459, -21.23658630136709391, 11.49999999999998934 ) ) ;
#95352 = CARTESIAN_POINT ( 'NONE',  ( -80.52287095714999055, -24.92579138211018730, 1.929029949965667567 ) ) ;
#95353 = ORIENTED_EDGE ( 'NONE', *, *, #31388, .T. ) ;
#95354 = DIRECTION ( 'NONE',  ( -3.773278334453079030E-23, 0.9999999999976377785, 2.173523156925979128E-06 ) ) ;
#95355 = CARTESIAN_POINT ( 'NONE',  ( -78.52287095715006160, -23.47596703998600631, 11.44779298504228571 ) ) ;
#95356 = CARTESIAN_POINT ( 'NONE',  ( -19.80875734969026425, -0.3587747205144265483, 31.02402280011862246 ) ) ;
#95357 = CARTESIAN_POINT ( 'NONE',  ( -118.1692254313890231, -25.21288489780929964, 6.500946880900415614 ) ) ;
#95358 = VECTOR ( 'NONE', #44918, 1000.000000000000114 ) ;
#95360 = ORIENTED_EDGE ( 'NONE', *, *, #31016, .F. ) ;
#95359 = CARTESIAN_POINT ( 'NONE',  ( -11.21157863559261791, -18.18922556752850994, 11.49999999999999645 ) ) ;
#95361 = ORIENTED_EDGE ( 'NONE', *, *, #41552, .F. ) ;
#95362 = CARTESIAN_POINT ( 'NONE',  ( -8.951960448472247478, 20.35530821588910300, -1.500000000000002220 ) ) ;
#95363 = CARTESIAN_POINT ( 'NONE',  ( 18.09409571311175569, -9.955296453752364272, -1.500000000000002220 ) ) ;
#95364 = ORIENTED_EDGE ( 'NONE', *, *, #46115, .T. ) ;
#95365 = CARTESIAN_POINT ( 'NONE',  ( -6.128026245051341192, -5.876774720514410077, 19.39236848396478763 ) ) ;
#95366 = CARTESIAN_POINT ( 'NONE',  ( 3.248328688408994580, -5.876774720514406525, 18.75910638930973917 ) ) ;
#95367 = EDGE_LOOP ( 'NONE', ( #100225, #29244, #686, #83865 ) ) ;
#95368 = CARTESIAN_POINT ( 'NONE',  ( -111.6228709571500559, -23.47593901973091235, -1.443836447538999312 ) ) ;
#95369 = B_SPLINE_CURVE_WITH_KNOTS ( 'NONE', 3,
 ( #37051, #67026, #91832, #83219 ),
 .UNSPECIFIED., .F., .F.,
 ( 4, 4 ),
 ( 0.000000000000000000, 9.999999999999591193E-05 ),
 .UNSPECIFIED. ) ;
#95370 = ORIENTED_EDGE ( 'NONE', *, *, #47716, .T. ) ;
#95371 = CARTESIAN_POINT ( 'NONE',  ( 13.80377080874918150, -3.316774720514426900, -27.21172484903264532 ) ) ;
#95372 = CARTESIAN_POINT ( 'NONE',  ( 0.000000000000000000, 4.132774720514426292, 0.000000000000000000 ) ) ;
#95373 = CARTESIAN_POINT ( 'NONE',  ( 16.15719879640481338, -13.26386290209467944, -1.500000000000002220 ) ) ;
#95374 = EDGE_CURVE ( 'NONE', #18993, #70394, #88438, .T. ) ;
#95375 = CARTESIAN_POINT ( 'NONE',  ( 9.643594380127815668, 19.59848315111488759, 11.49999999999999645 ) ) ;
#95376 = CARTESIAN_POINT ( 'NONE',  ( -73.59227796171214209, -24.15620529776628089, 10.23563542870660470 ) ) ;
#95377 = CARTESIAN_POINT ( 'NONE',  ( -37.62287095715007013, -24.34917612406837861, 0.1852690917426592920 ) ) ;
#95378 = CARTESIAN_POINT ( 'NONE',  ( 20.54305097139451064, 9.177977666691313985, 11.49999999999998934 ) ) ;
#95379 = CARTESIAN_POINT ( 'NONE',  ( 12.70736309587848645, -16.60074808024427284, 11.49999999999998934 ) ) ;
#95380 = CARTESIAN_POINT ( 'NONE',  ( -38.53316654600265423, -24.51314013834316086, 0.6176544820404135105 ) ) ;
#95381 = PLANE ( 'NONE',  #82575 ) ;
#95382 = CARTESIAN_POINT ( 'NONE',  ( -9.543201319291914093E-14, -6.376774720514426953, 18.21871304725679508 ) ) ;
#95383 = EDGE_LOOP ( 'NONE', ( #94656, #84870, #75397, #761 ) ) ;
#95384 = EDGE_CURVE ( 'NONE', #61485, #55194, #48285, .T. ) ;
#95385 = ORIENTED_EDGE ( 'NONE', *, *, #23117, .T. ) ;
#95386 = ORIENTED_EDGE ( 'NONE', *, *, #92933, .F. ) ;
#95387 = EDGE_CURVE ( 'NONE', #21581, #24307, #89216, .T. ) ;
#95388 = CARTESIAN_POINT ( 'NONE',  ( -99.29755759592676156, -25.26221118157064538, 6.181036435632247361 ) ) ;
#95389 = ORIENTED_EDGE ( 'NONE', *, *, #23812, .F. ) ;
#95390 = CARTESIAN_POINT ( 'NONE',  ( -11.99125074976391048, 17.70416384622758343, -1.500000000000002220 ) ) ;
#95391 = CARTESIAN_POINT ( 'NONE',  ( -20.95026660567425481, -7.857139728745305973, 11.49999999999999645 ) ) ;
#95392 = VERTEX_POINT ( 'NONE', #47783 ) ;
#95393 = CARTESIAN_POINT ( 'NONE',  ( -26.29209366616924015, -24.89473993083786851, 6.397464118119456700 ) ) ;
#95394 = CARTESIAN_POINT ( 'NONE',  ( 5.245434476726341444, -20.39595507048906242, 11.49999999999998934 ) ) ;
#95395 = CARTESIAN_POINT ( 'NONE',  ( -30.60461477208441750, -24.58290936297911955, 9.174392229302920754 ) ) ;
#95396 = CARTESIAN_POINT ( 'NONE',  ( 19.92730240972663935, 0.8534881809820089593, -1.500000000000002220 ) ) ;
#95398 = CARTESIAN_POINT ( 'NONE',  ( -50.47484537770900204, -25.00182538069147142, 7.747789668545043362 ) ) ;
#95397 = CIRCLE ( 'NONE', #16223, 0.3000000000000016542 ) ;
#95399 = CARTESIAN_POINT ( 'NONE',  ( -101.6251937039718598, -24.51314013834316086, 0.6176544820404198388 ) ) ;
#95400 = CARTESIAN_POINT ( 'NONE',  ( 19.60348439636399931, 10.09110264789753053, -1.500000000000002220 ) ) ;
#95401 = ORIENTED_EDGE ( 'NONE', *, *, #18937, .T. ) ;
#95402 = CARTESIAN_POINT ( 'NONE',  ( -65.61529913176147488, -23.48786465467241058, 11.44779295918254824 ) ) ;
#95403 = EDGE_CURVE ( 'NONE', #52326, #94778, #86335, .T. ) ;
#95404 = B_SPLINE_CURVE_WITH_KNOTS ( 'NONE', 3,
 ( #5203, #75699, #13301, #82818 ),
 .UNSPECIFIED., .F., .F.,
 ( 4, 4 ),
 ( 0.000000000000000000, 9.999999999998897304E-05 ),
 .UNSPECIFIED. ) ;
#95405 = CARTESIAN_POINT ( 'NONE',  ( -109.6228709571500559, -29.50250243563736774, 8.947779886222136270 ) ) ;
#95406 = CARTESIAN_POINT ( 'NONE',  ( -60.57813654160024441, -24.92564183028978420, 1.928384488918252648 ) ) ;
#95407 = VECTOR ( 'NONE', #91735, 1000.000000000000114 ) ;
#95408 = CARTESIAN_POINT ( 'NONE',  ( -62.50953048082695318, -23.96169478059712787, 10.65365249895718414 ) ) ;
#95409 = DIRECTION ( 'NONE',  ( 0.000000000000000000, 0.000000000000000000, -1.000000000000000000 ) ) ;
#95410 = DIRECTION ( 'NONE',  ( -3.773278334453080206E-23, 0.9999999999976377785, 2.173523156925979975E-06 ) ) ;
#95411 = CARTESIAN_POINT ( 'NONE',  ( 3.065528897535349628, -21.08962430476942274, -1.500000000000002220 ) ) ;
#95412 = CARTESIAN_POINT ( 'NONE',  ( -104.5228709571500758, -23.73934037231757443, 11.05740245334328087 ) ) ;
#95413 = CARTESIAN_POINT ( 'NONE',  ( -124.5228709571500332, -23.94994826722565762, -0.6494450866342719175 ) ) ;
#95414 = FACE_OUTER_BOUND ( 'NONE', #36580, .T. ) ;
#95415 = CARTESIAN_POINT ( 'NONE',  ( -114.6228709571500559, -24.64898659630528854, 1.056161002820831474 ) ) ;
#95416 = CARTESIAN_POINT ( 'NONE',  ( 5.419076944403256491, 21.93356404788375258, -1.500000000000002220 ) ) ;
#95417 = DIRECTION ( 'NONE',  ( 0.000000000000000000, -2.173523156925980399E-06, 0.9999999999976378895 ) ) ;
#95418 = ORIENTED_EDGE ( 'NONE', *, *, #51494, .T. ) ;
#95419 = CARTESIAN_POINT ( 'NONE',  ( -1.358974358974357921, -6.376774720514420736, 20.75510817307693046 ) ) ;
#95420 = CARTESIAN_POINT ( 'NONE',  ( -31.62934438217061839, -24.51419770103156637, 9.386484678747187615 ) ) ;
#95421 = CARTESIAN_POINT ( 'NONE',  ( -18.74838588596843181, -5.942601993926947657, 11.49999999999999645 ) ) ;
#95422 = DIRECTION ( 'NONE',  ( 0.000000000000000000, 2.173523156925980399E-06, -0.9999999999976378895 ) ) ;
#95423 = CIRCLE ( 'NONE', #72686, 130.7884398600581335 ) ;
#95424 = FACE_OUTER_BOUND ( 'NONE', #37531, .T. ) ;
#95425 = ADVANCED_FACE ( 'NONE', ( #81602 ), #12072, .F. ) ;
#95426 = VERTEX_POINT ( 'NONE', #63017 ) ;
#95427 = CARTESIAN_POINT ( 'NONE',  ( -42.62287095715004881, -23.47593901973091235, -1.443836447539011525 ) ) ;
#95428 = CARTESIAN_POINT ( 'NONE',  ( -39.62287095715005592, -24.65952944569304606, 1.056160979905692354 ) ) ;
#95429 = CARTESIAN_POINT ( 'NONE',  ( -122.6228709571500417, -24.64898659630368627, 1.056161002820833028 ) ) ;
#95430 = PLANE ( 'NONE',  #72892 ) ;
#95431 = CARTESIAN_POINT ( 'NONE',  ( -76.52287095715007581, -24.66019654487199730, 8.947790411086124607 ) ) ;
#95432 = DIRECTION ( 'NONE',  ( 0.000000000000000000, 0.000000000000000000, -1.000000000000000000 ) ) ;
#95433 = CARTESIAN_POINT ( 'NONE',  ( -16.86558833231006460, 10.32443627698238409, 11.49999999999998934 ) ) ;
#95434 = ORIENTED_EDGE ( 'NONE', *, *, #61931, .F. ) ;
#95435 = CARTESIAN_POINT ( 'NONE',  ( -0.9278407348523283193, 20.21260682001012654, 11.49999999999999645 ) ) ;
#95436 = CARTESIAN_POINT ( 'NONE',  ( -7.635352852713973348, -5.876774720514416295, 20.14409848895066091 ) ) ;
#95437 = VECTOR ( 'NONE', #96190, 1000.000000000000000 ) ;
#95438 = ADVANCED_FACE ( 'NONE', ( #54895 ), #8717, .F. ) ;
#95439 = ORIENTED_EDGE ( 'NONE', *, *, #44620, .T. ) ;
#95440 = DIRECTION ( 'NONE',  ( 7.726610339123061470E-14, 0.000000000000000000, -1.000000000000000000 ) ) ;
#95441 = CARTESIAN_POINT ( 'NONE',  ( -72.62287095715005592, -23.47596703998600631, 11.44779298504227860 ) ) ;
#95442 = CYLINDRICAL_SURFACE ( 'NONE', #28277, 18.50000000000000355 ) ;
#95443 = FACE_OUTER_BOUND ( 'NONE', #45571, .T. ) ;
#95444 = CARTESIAN_POINT ( 'NONE',  ( -39.62287095715005592, -23.96127896941631619, -0.6493128931037891460 ) ) ;
#95445 = DIRECTION ( 'NONE',  ( -3.773278334453079030E-23, 0.9999999999976377785, 2.173523156925979128E-06 ) ) ;
#95446 = CARTESIAN_POINT ( 'NONE',  ( 20.03642891561555928, 0.6179553080306146029, -1.500000000000002220 ) ) ;
#95447 = DIRECTION ( 'NONE',  ( -6.267148949376405333E-16, 1.000000000000000000, 5.583826031377241668E-16 ) ) ;
#95448 = ORIENTED_EDGE ( 'NONE', *, *, #11217, .T. ) ;
#95449 = CARTESIAN_POINT ( 'NONE',  ( -58.52287095715009713, -24.66019654487199730, 8.947790411086121054 ) ) ;
#95450 = PLANE ( 'NONE',  #70438 ) ;
#95451 = DIRECTION ( 'NONE',  ( 0.000000000000000000, 0.000000000000000000, -1.000000000000000000 ) ) ;
#95452 = DIRECTION ( 'NONE',  ( -1.000000000000000000, 0.000000000000000000, -1.226388327005079762E-16 ) ) ;
#95453 = CARTESIAN_POINT ( 'NONE',  ( -101.4436883411118515, -25.18151332244121221, 3.266733668633749588 ) ) ;
#95454 = ADVANCED_FACE ( 'NONE', ( #19189 ), #40164, .F. ) ;
#95455 = DIRECTION ( 'NONE',  ( 0.000000000000000000, 0.000000000000000000, 1.000000000000000000 ) ) ;
#95456 = CARTESIAN_POINT ( 'NONE',  ( -98.87392103467360016, -25.32724633150700200, 4.398074151685131383 ) ) ;
#95457 = ORIENTED_EDGE ( 'NONE', *, *, #3414, .T. ) ;
#95458 = ADVANCED_FACE ( 'NONE', ( #2117 ), #54277, .T. ) ;
#95459 = AXIS2_PLACEMENT_3D ( 'NONE', #44933, #68261, #236 ) ;
#95460 = CARTESIAN_POINT ( 'NONE',  ( -5.305567426876419468, 19.62801697144059787, 11.49999999999998934 ) ) ;
#95461 = VERTEX_POINT ( 'NONE', #44538 ) ;
#95462 = CARTESIAN_POINT ( 'NONE',  ( 31.62500054620340251, 6.365374413700245704, 26.93529845007237711 ) ) ;
#95463 = CARTESIAN_POINT ( 'NONE',  ( -127.5552447816560857, -24.51419770103158768, 9.386484678747160970 ) ) ;
#95465 = ORIENTED_EDGE ( 'NONE', *, *, #25894, .T. ) ;
#95464 = ADVANCED_FACE ( 'NONE', ( #97323, #84085 ), #36917, .T. ) ;
#95466 = VECTOR ( 'NONE', #80658, 1000.000000000000000 ) ;
#95467 = CARTESIAN_POINT ( 'NONE',  ( -88.55620429048337883, -23.48786465467241058, 11.44779295918254647 ) ) ;
#95468 = EDGE_CURVE ( 'NONE', #50118, #3684, #27809, .T. ) ;
#95469 = CARTESIAN_POINT ( 'NONE',  ( -49.94169464672810221, -25.26264163214096570, 7.031227749355628553 ) ) ;
#95470 = AXIS2_PLACEMENT_3D ( 'NONE', #28948, #8618, #96236 ) ;
#95471 = CARTESIAN_POINT ( 'NONE',  ( -30.47287095715007155, -25.11030793521390692, 2.751272914309959017 ) ) ;
#95472 = CARTESIAN_POINT ( 'NONE',  ( -8.144517828999388698, 19.50133175306300970, 11.49999999999999645 ) ) ;
#95473 = EDGE_CURVE ( 'NONE', #62593, #48556, #83582, .T. ) ;
#95474 = VECTOR ( 'NONE', #81235, 999.9999999999998863 ) ;
#95475 = CARTESIAN_POINT ( 'NONE',  ( 8.970247382295582383, 20.24485829007567617, 11.49999999999998934 ) ) ;
#95476 = CARTESIAN_POINT ( 'NONE',  ( -16.28974412851428255, -12.55652860423730388, 11.49999999999998934 ) ) ;
#95477 = EDGE_LOOP ( 'NONE', ( #58321, #7834, #50940, #54706 ) ) ;
#95478 = CARTESIAN_POINT ( 'NONE',  ( -41.63441546978912555, -24.34968618360933590, 0.1864209137778856940 ) ) ;
#95479 = ORIENTED_EDGE ( 'NONE', *, *, #57807, .F. ) ;
#95480 = DIRECTION ( 'NONE',  ( -0.000000000000000000, 2.173523156925979552E-06, -0.9999999999976378895 ) ) ;
#95481 = CARTESIAN_POINT ( 'NONE',  ( -109.5228709571500758, -23.72773821059536914, 11.05748984161097503 ) ) ;
#95482 = VERTEX_POINT ( 'NONE', #36418 ) ;
#95483 = VERTEX_POINT ( 'NONE', #45541 ) ;
#95484 = VECTOR ( 'NONE', #72022, 1000.000000000000000 ) ;
#95485 = ORIENTED_EDGE ( 'NONE', *, *, #21808, .F. ) ;
#95486 = CARTESIAN_POINT ( 'NONE',  ( -100.5228709571500758, -23.47593901973090524, -1.443836447538996648 ) ) ;
#95487 = CARTESIAN_POINT ( 'NONE',  ( 7.165897526731081157, -6.376774720514420736, 20.76279523443833597 ) ) ;
#95488 = CARTESIAN_POINT ( 'NONE',  ( 5.495499487697820484, -5.876774720514418071, 20.18701882043406926 ) ) ;
#95489 = CARTESIAN_POINT ( 'NONE',  ( -17.26476610439243231, 11.37957233835482818, -1.500000000000002220 ) ) ;
#95490 = EDGE_CURVE ( 'NONE', #89124, #71759, #90207, .T. ) ;
#95491 = CARTESIAN_POINT ( 'NONE',  ( 11.52859134480388903, -18.33581920571378632, 11.49999999999999645 ) ) ;
#95492 = ORIENTED_EDGE ( 'NONE', *, *, #11715, .T. ) ;
#95493 = CARTESIAN_POINT ( 'NONE',  ( -60.52287095715003318, -24.83620972995333531, 8.398175272756253307 ) ) ;
#95494 = CARTESIAN_POINT ( 'NONE',  ( 2.589743589743596086, -5.876774720514419847, 20.00140224358974095 ) ) ;
#95495 = CARTESIAN_POINT ( 'NONE',  ( 6.968497804723354783, -21.30229754059623559, -1.500000000000002220 ) ) ;
#95496 = DIRECTION ( 'NONE',  ( -3.773278334453079030E-23, 0.9999999999976377785, 2.173523156925979128E-06 ) ) ;
#95497 = CARTESIAN_POINT ( 'NONE',  ( 29.73860345376319358, 4.772774720514425972, 0.000000000000000000 ) ) ;
#95498 = ORIENTED_EDGE ( 'NONE', *, *, #10044, .F. ) ;
#95499 = B_SPLINE_CURVE_WITH_KNOTS ( 'NONE', 3,
 ( #13919, #50502, #82931, #83430, #60625, #21524, #12429, #75321 ),
 .UNSPECIFIED., .F., .F.,
 ( 4, 2, 2, 4 ),
 ( -0.001240666984356067221, -0.0002401179793396696679, 0.0007604310256767278856, 0.002761529035709522992 ),
 .UNSPECIFIED. ) ;
#95500 = CARTESIAN_POINT ( 'NONE',  ( 11.92750898180832131, -4.915819049120522699, -27.17522536519172860 ) ) ;
#95501 = VERTEX_POINT ( 'NONE', #12580 ) ;
#95502 = EDGE_LOOP ( 'NONE', ( #87626, #88101, #41296, #77413 ) ) ;
#95504 = EDGE_CURVE ( 'NONE', #12744, #78991, #76461, .T. ) ;
#95503 = CYLINDRICAL_SURFACE ( 'NONE', #89548, 0.2499999999997798983 ) ;
#95505 = VERTEX_POINT ( 'NONE', #91691 ) ;
#95506 = DIRECTION ( 'NONE',  ( -3.773278334453080206E-23, 0.9999999999976377785, 2.173523156925979975E-06 ) ) ;
#95507 = CARTESIAN_POINT ( 'NONE',  ( 1.567330217057175901, -21.20382687294985047, -1.500000000000002220 ) ) ;
#95508 = EDGE_CURVE ( 'NONE', #86083, #53725, #90708, .T. ) ;
#95509 = ORIENTED_EDGE ( 'NONE', *, *, #55903, .T. ) ;
#95510 = CARTESIAN_POINT ( 'NONE',  ( -101.1410787236130489, -25.15676149906418857, 6.899366854011507399 ) ) ;
#95511 = CARTESIAN_POINT ( 'NONE',  ( 12.66963027563507005, -17.75133666976559255, 11.49999999999998934 ) ) ;
#95512 = CARTESIAN_POINT ( 'NONE',  ( -103.5195636159563719, -23.73791477778911840, 11.05961554403170410 ) ) ;
#95513 = CARTESIAN_POINT ( 'NONE',  ( -62.52287095715003318, -24.66019654487199730, 8.947790411086124607 ) ) ;
#95514 = DIRECTION ( 'NONE',  ( -0.000000000000000000, 1.000000000000000000, -0.000000000000000000 ) ) ;
#95515 = CARTESIAN_POINT ( 'NONE',  ( 21.14253370195585546, 5.708146584608840612, -1.500000000000002220 ) ) ;
#95516 = DIRECTION ( 'NONE',  ( -0.9822594791677485837, 0.000000000000000000, 0.1875268396392987258 ) ) ;
#95517 = ORIENTED_EDGE ( 'NONE', *, *, #99852, .T. ) ;
#95518 = CARTESIAN_POINT ( 'NONE',  ( 0.000000000000000000, -0.9000000000000000222, 0.000000000000000000 ) ) ;
#95519 = FACE_OUTER_BOUND ( 'NONE', #70771, .T. ) ;
#95520 = EDGE_CURVE ( 'NONE', #59433, #45083, #98810, .T. ) ;
#95521 = ADVANCED_FACE ( 'NONE', ( #6968 ), #22175, .T. ) ;
#95522 = ORIENTED_EDGE ( 'NONE', *, *, #25606, .T. ) ;
#95523 = CARTESIAN_POINT ( 'NONE',  ( -99.62287095715007013, -24.50321055353805022, 9.387540953477524042 ) ) ;
#95524 = EDGE_CURVE ( 'NONE', #52082, #99074, #41173, .T. ) ;
#95525 = VERTEX_POINT ( 'NONE', #5469 ) ;
#95526 = CARTESIAN_POINT ( 'NONE',  ( 13.03371494964462407, 6.475225279485575136, -27.13839018153349869 ) ) ;
#95527 = CARTESIAN_POINT ( 'NONE',  ( -82.62937087436195327, -24.34968618360933945, 0.1864209137778926328 ) ) ;
#95528 = CARTESIAN_POINT ( 'NONE',  ( 21.23515499356076930, 0.7789969333488580006, -1.500000000000002220 ) ) ;
#95529 = DIRECTION ( 'NONE',  ( -3.773278334453080206E-23, 0.9999999999976377785, 2.173523156925979552E-06 ) ) ;
#95530 = CARTESIAN_POINT ( 'NONE',  ( -130.5728709571500588, -24.92410949913934104, 1.600845668900850116 ) ) ;
#95531 = DIRECTION ( 'NONE',  ( 0.000000000000000000, 0.000000000000000000, -1.000000000000000000 ) ) ;
#95532 = CARTESIAN_POINT ( 'NONE',  ( -109.5228709571500616, -23.47596703998600631, 11.44779298504228038 ) ) ;
#95533 = CARTESIAN_POINT ( 'NONE',  ( -13.55963120218723361, -13.89248740512243430, -1.500000000000002220 ) ) ;
#95534 = CARTESIAN_POINT ( 'NONE',  ( -80.55620429048339304, -23.48786465467240703, 11.44779295918254824 ) ) ;
#95535 = ORIENTED_EDGE ( 'NONE', *, *, #52164, .F. ) ;
#95536 = CARTESIAN_POINT ( 'NONE',  ( -19.51626497420292239, -0.3564122556526727048, 11.49999999999999645 ) ) ;
#95537 = DIRECTION ( 'NONE',  ( 0.000000000000000000, 1.000000000000000000, 0.000000000000000000 ) ) ;
#95538 = VECTOR ( 'NONE', #32564, 999.9999999999998863 ) ;
#95539 = B_SPLINE_CURVE_WITH_KNOTS ( 'NONE', 3,
 ( #11755, #97979, #34111, #81275 ),
 .UNSPECIFIED., .F., .F.,
 ( 4, 4 ),
 ( 0.000000000000000000, 9.999999999998897304E-05 ),
 .UNSPECIFIED. ) ;
#95540 = CARTESIAN_POINT ( 'NONE',  ( -80.19178569327479522, -25.12886892462663369, 7.067847742069440109 ) ) ;
#95541 = ORIENTED_EDGE ( 'NONE', *, *, #44159, .F. ) ;
#95542 = CARTESIAN_POINT ( 'NONE',  ( 4.638796026491669444, -5.876774720514423400, 21.40644651702305268 ) ) ;
#95543 = PLANE ( 'NONE',  #96606 ) ;
#95544 = CIRCLE ( 'NONE', #51800, 2.040000000000000036 ) ;
#95545 = DIRECTION ( 'NONE',  ( 3.773278334444167608E-23, -1.000000000000000000, 0.000000000000000000 ) ) ;
#95546 = CARTESIAN_POINT ( 'NONE',  ( -81.67724764284677974, -25.03155920135590762, 6.915644353864915495 ) ) ;
#95547 = CARTESIAN_POINT ( 'NONE',  ( -3.718233408413001762, 19.32670252783854536, 11.49999999999998934 ) ) ;
#95548 = VECTOR ( 'NONE', #7122, 1000.000000000000000 ) ;
#95549 = EDGE_LOOP ( 'NONE', ( #226, #94480, #35571, #984, #23456, #44541 ) ) ;
#95550 = AXIS2_PLACEMENT_3D ( 'NONE', #24073, #70761, #78353 ) ;
#95551 = DIRECTION ( 'NONE',  ( 2.352173255807804438E-16, -2.352173255807796056E-16, -1.000000000000000000 ) ) ;
#95552 = CARTESIAN_POINT ( 'NONE',  ( -18.41700849636773540, 13.91914711744011157, -1.500000000000002220 ) ) ;
#95553 = VECTOR ( 'NONE', #75401, 1000.000000000000000 ) ;
#95554 = DATE_AND_TIME ( #1213, #99146 ) ;
#95555 = VERTEX_POINT ( 'NONE', #98301 ) ;
#95556 = CARTESIAN_POINT ( 'NONE',  ( -63.62287095715004881, -29.50250243563736774, 8.947779886222145151 ) ) ;
#95557 = DIRECTION ( 'NONE',  ( -0.9952638024365005887, -0.000000000000000000, -0.09721092304694053943 ) ) ;
#95558 = CARTESIAN_POINT ( 'NONE',  ( -114.5895376238167245, -24.64898659630528854, 1.056161002820831252 ) ) ;
#95559 = CARTESIAN_POINT ( 'NONE',  ( -97.59370094711790955, -23.96169478059714208, 10.65365249895717703 ) ) ;
#95560 = CARTESIAN_POINT ( 'NONE',  ( -81.90499567650900303, -25.14083923594767356, 2.947789366383930965 ) ) ;
#95561 = CARTESIAN_POINT ( 'NONE',  ( -41.32836283488544638, -2.682774720514426559, 39.26872235229541985 ) ) ;
#95562 = CARTESIAN_POINT ( 'NONE',  ( -73.52287095715006160, -23.72747288104470087, -1.053458166803226570 ) ) ;
#95563 = CARTESIAN_POINT ( 'NONE',  ( -8.676013072486071565, -17.92234406281952275, -1.500000000000002220 ) ) ;
#95564 = CARTESIAN_POINT ( 'NONE',  ( -75.49751960664619332, -24.63419186844611275, 9.035850630976923981 ) ) ;
#95565 = CARTESIAN_POINT ( 'NONE',  ( -15.96263503330635380, 11.84234753045382682, -1.500000000000002220 ) ) ;
#95566 = EDGE_LOOP ( 'NONE', ( #27031, #70645, #18617, #75369 ) ) ;
#95567 = LINE ( 'NONE', #72744, #29703 ) ;
#95568 = CARTESIAN_POINT ( 'NONE',  ( -51.05935189857146383, -25.15701052765065882, 6.962205197853442940 ) ) ;
#95569 = CARTESIAN_POINT ( 'NONE',  ( 32.98733314340959311, -5.965225279485572685, 2.074222136288530027 ) ) ;
#95570 = CARTESIAN_POINT ( 'NONE',  ( 6.310942340984578180, -6.376774720514426953, -25.29254520177807208 ) ) ;
#95571 = CARTESIAN_POINT ( 'NONE',  ( -19.91680486407696904, 5.911688619927280008, 11.49999999999999645 ) ) ;
#95572 = DIRECTION ( 'NONE',  ( -0.9951627101165076983, -0.09824042138329588947, -3.430045979798635096E-16 ) ) ;
#95573 = DIRECTION ( 'NONE',  ( -1.000000000000000000, 0.000000000000000000, 0.000000000000000000 ) ) ;
#95574 = CARTESIAN_POINT ( 'NONE',  ( 7.824713763024562674, 21.46283361357968289, 11.49999999999999645 ) ) ;
#95576 = ADVANCED_FACE ( 'NONE', ( #75463 ), #53158, .T. ) ;
#95575 = VERTEX_POINT ( 'NONE', #51654 ) ;
#95577 = CARTESIAN_POINT ( 'NONE',  ( -108.5562042904834072, -24.64965694238575011, 8.947790433994187609 ) ) ;
#95578 = CARTESIAN_POINT ( 'NONE',  ( -127.5222628909410645, -23.48783264082477373, -1.443836473390084363 ) ) ;
#95579 = ORIENTED_EDGE ( 'NONE', *, *, #26447, .F. ) ;
#95580 = CARTESIAN_POINT ( 'NONE',  ( -16.41926757845921614, -11.79510067912178606, 11.49999999999998934 ) ) ;
#95581 = CARTESIAN_POINT ( 'NONE',  ( 7.403636664866980688, -6.376774720514424288, 21.18544102487025782 ) ) ;
#95582 = CARTESIAN_POINT ( 'NONE',  ( -110.5228709571500616, -25.00182538069145366, 7.747789668545101094 ) ) ;
#95583 = ADVANCED_FACE ( 'NONE', ( #13568 ), #5964, .F. ) ;
#95584 = EDGE_CURVE ( 'NONE', #20835, #47459, #76375, .T. ) ;
#95585 = CARTESIAN_POINT ( 'NONE',  ( -27.13414387080440093, 5.965225279485594001, -10.21530720150730254 ) ) ;
#95586 = EDGE_CURVE ( 'NONE', #73913, #69024, #75119, .T. ) ;
#95587 = ORIENTED_EDGE ( 'NONE', *, *, #14394, .F. ) ;
#95588 = PLANE ( 'NONE',  #9564 ) ;
#95589 = CARTESIAN_POINT ( 'NONE',  ( -100.6228709571500417, -24.62226745350440638, 0.9660975649729649506 ) ) ;
#95590 = CARTESIAN_POINT ( 'NONE',  ( 16.76344175524385705, -10.90933549886441156, -1.500000000000002220 ) ) ;
#95591 = CARTESIAN_POINT ( 'NONE',  ( 12.86141378215833342, 16.59024694808438127, 11.49999999999999645 ) ) ;
#95592 = ADVANCED_FACE ( 'NONE', ( #52646 ), #8084, .T. ) ;
#95593 = DIRECTION ( 'NONE',  ( -0.000000000000000000, 1.000000000000000000, -0.000000000000000000 ) ) ;
#95594 = DIRECTION ( 'NONE',  ( 1.000000000000000000, -0.000000000000000000, 0.000000000000000000 ) ) ;
#95595 = CARTESIAN_POINT ( 'NONE',  ( 18.22792733936863030, -12.41963300964812156, -1.500000000000002220 ) ) ;
#95596 = AXIS2_PLACEMENT_3D ( 'NONE', #106, #31045, #23935 ) ;
#95597 = CARTESIAN_POINT ( 'NONE',  ( -39.93582354980947002, -25.31589308170816821, 4.982375540116844803 ) ) ;
#95598 = VERTEX_POINT ( 'NONE', #100285 ) ;
#95599 = PLANE ( 'NONE',  #77771 ) ;
#95600 = CARTESIAN_POINT ( 'NONE',  ( -118.5228709571500758, -23.48786465467241769, 11.44779295918253759 ) ) ;
#95601 = LINE ( 'NONE', #26089, #93178 ) ;
#95602 = ORIENTED_EDGE ( 'NONE', *, *, #74955, .F. ) ;
#95603 = DIRECTION ( 'NONE',  ( 0.000000000000000000, -2.173523156925979552E-06, 0.9999999999976378895 ) ) ;
#95604 = EDGE_LOOP ( 'NONE', ( #7287, #14107 ) ) ;
#95605 = CIRCLE ( 'NONE', #51869, 3.349999999999998757 ) ;
#95606 = ORIENTED_EDGE ( 'NONE', *, *, #56004, .F. ) ;
#95607 = DIRECTION ( 'NONE',  ( -1.000000000000000000, -3.773278334444167608E-23, -8.201307833595939069E-29 ) ) ;
#95608 = CARTESIAN_POINT ( 'NONE',  ( -72.62287095715004170, -23.48786465467241058, 11.44779295918254647 ) ) ;
#95609 = DIRECTION ( 'NONE',  ( -1.000000000000000000, 0.000000000000000000, 0.000000000000000000 ) ) ;
#95610 = CARTESIAN_POINT ( 'NONE',  ( -7.444040098415714013, -19.11467064512029879, -1.500000000000002220 ) ) ;
#95611 = ADVANCED_FACE ( 'NONE', ( #30805 ), #47540, .F. ) ;
#95612 = ORIENTED_EDGE ( 'NONE', *, *, #10854, .F. ) ;
#95613 = CARTESIAN_POINT ( 'NONE',  ( -66.62287095715005592, -29.50250786944525672, 11.44777988621623699 ) ) ;
#95614 = VECTOR ( 'NONE', #70636, 1000.000000000000114 ) ;
#95615 = CARTESIAN_POINT ( 'NONE',  ( 6.963174204274080736, -5.876774720514416295, 20.29202897614545975 ) ) ;
#95616 = CARTESIAN_POINT ( 'NONE',  ( 9.278253834636469577, -5.876774720514426953, 21.48128695274316158 ) ) ;
#95617 = CARTESIAN_POINT ( 'NONE',  ( 11.81759748825469281, -18.92407201980706333, -1.500000000000002220 ) ) ;
#95618 = CARTESIAN_POINT ( 'NONE',  ( -102.5228709571500758, -23.47596703998600631, 11.44779298504228215 ) ) ;
#95619 = DIRECTION ( 'NONE',  ( -3.773278334453079618E-23, 0.9999999999976377785, 2.173523156925978705E-06 ) ) ;
#95620 = EDGE_CURVE ( 'NONE', #31086, #1896, #54160, .T. ) ;
#95621 = EDGE_LOOP ( 'NONE', ( #20273, #82209, #13132, #83425 ) ) ;
#95622 = CARTESIAN_POINT ( 'NONE',  ( -104.5228709571500758, -24.66019654487200441, 8.947790411086113949 ) ) ;
#95623 = VECTOR ( 'NONE', #73155, 1000.000000000000114 ) ;
#95624 = CARTESIAN_POINT ( 'NONE',  ( 26.25551457520356635, 1.682774720514426114, -10.59759736550661913 ) ) ;
#95625 = VECTOR ( 'NONE', #65172, 1000.000000000000000 ) ;
#95626 = CARTESIAN_POINT ( 'NONE',  ( 19.93353245626563819, -6.116835970281883306, -1.500000000000002220 ) ) ;
#95627 = ORIENTED_EDGE ( 'NONE', *, *, #18090, .F. ) ;
#95630 = ORIENTED_EDGE ( 'NONE', *, *, #80364, .T. ) ;
#95629 = EDGE_CURVE ( 'NONE', #20120, #7838, #53396, .T. ) ;
#95628 = PLANE ( 'NONE',  #89228 ) ;
#95631 = ORIENTED_EDGE ( 'NONE', *, *, #9502, .T. ) ;
#95632 = AXIS2_PLACEMENT_3D ( 'NONE', #69698, #39236, #37252 ) ;
#95633 = CARTESIAN_POINT ( 'NONE',  ( -68.94101663640660149, -25.03149086959048120, 6.247842836060496730 ) ) ;
#95634 = CARTESIAN_POINT ( 'NONE',  ( -16.48755246578841849, -13.11705038010048163, -1.500000000000002220 ) ) ;
#95635 = ORIENTED_EDGE ( 'NONE', *, *, #88733, .T. ) ;
#95636 = DIRECTION ( 'NONE',  ( -3.773278334453079030E-23, 0.9999999999976377785, 2.173523156925978705E-06 ) ) ;
#95637 = PLANE ( 'NONE',  #20689 ) ;
#95638 = CARTESIAN_POINT ( 'NONE',  ( -120.5877765925405640, -25.00182538069146787, 7.747789668545044250 ) ) ;
#95639 = CARTESIAN_POINT ( 'NONE',  ( -100.8646123533485621, -25.25419544284016737, 7.517421368992579289 ) ) ;
#95640 = CARTESIAN_POINT ( 'NONE',  ( -59.62769267835140852, -24.51314013834316441, 0.6176544820404136216 ) ) ;
#95641 = CARTESIAN_POINT ( 'NONE',  ( -1.268225406894735396, -21.67698866206750097, -1.500000000000002220 ) ) ;
#95642 = CARTESIAN_POINT ( 'NONE',  ( -107.6228709571500701, -23.48783264082479150, -1.443836473390060382 ) ) ;
#95644 = VERTEX_POINT ( 'NONE', #351 ) ;
#95643 = CARTESIAN_POINT ( 'NONE',  ( 21.27325221474336914, 6.521069146585026566, 11.49999999999999645 ) ) ;
#95645 = CARTESIAN_POINT ( 'NONE',  ( -57.52287095715005449, -29.50250786944525672, 11.44777988621623876 ) ) ;
#95646 = CARTESIAN_POINT ( 'NONE',  ( 8.809764260727234841, -0.02602732333168140261, -3.697389739420774646 ) ) ;
#95647 = CARTESIAN_POINT ( 'NONE',  ( -71.30457154551152144, -25.24554880456021522, 6.209207408033732278 ) ) ;
#95649 = ORIENTED_EDGE ( 'NONE', *, *, #29372, .F. ) ;
#95648 = ADVANCED_FACE ( 'NONE', ( #94192 ), #4755, .T. ) ;
#95650 = EDGE_CURVE ( 'NONE', #32345, #98224, #10975, .T. ) ;
#95652 = ORIENTED_EDGE ( 'NONE', *, *, #18653, .T. ) ;
#95651 = DIRECTION ( 'NONE',  ( -1.000000000000000000, -0.000000000000000000, -0.000000000000000000 ) ) ;
#95653 = ORIENTED_EDGE ( 'NONE', *, *, #81141, .T. ) ;
#95654 = CARTESIAN_POINT ( 'NONE',  ( 4.712727796232550226, 3.316774720514426456, -25.55789472434992859 ) ) ;
#95655 = EDGE_CURVE ( 'NONE', #65926, #58835, #21914, .T. ) ;
#95656 = B_SPLINE_CURVE_WITH_KNOTS ( 'NONE', 3,
 ( #86161, #56736, #55733, #48114, #25258, #56237 ),
 .UNSPECIFIED., .F., .F.,
 ( 4, 2, 4 ),
 ( 0.000000000000000000, 0.001380901958385385509, 0.002761803916770771018 ),
 .UNSPECIFIED. ) ;
#95657 = CARTESIAN_POINT ( 'NONE',  ( -48.62287095715004881, -24.65952944569303895, 1.056160979905692798 ) ) ;
#95658 = CARTESIAN_POINT ( 'NONE',  ( -51.52287095715009713, -24.33927499327855060, 9.819080762295804732 ) ) ;
#95659 = ORIENTED_EDGE ( 'NONE', *, *, #88194, .F. ) ;
#95660 = B_SPLINE_CURVE_WITH_KNOTS ( 'NONE', 3,
 ( #15485, #55573, #14991, #62688, #70789, #53582, #47452, #38329, #1283, #31723, #69287, #16481, #100203, #38828, #30721, #93604, #8885, #39829, #61690, #23089 ),
 .UNSPECIFIED., .F., .F.,
 ( 4, 2, 2, 2, 2, 2, 2, 2, 2, 4 ),
 ( 0.000000000000000000, 0.0005520169820108884132, 0.001104033964021776826, 0.001656050946032664156, 0.002208067928043551485, 0.002760084910054437946, 0.003312101892065325275, 0.003864118874076212171, 0.004140127365081655401, 0.004416135856087097765 ),
 .UNSPECIFIED. ) ;
#95661 = CARTESIAN_POINT ( 'NONE',  ( -130.5728709571500588, -25.19110101596870877, 2.714942820864931328 ) ) ;
#95662 = CARTESIAN_POINT ( 'NONE',  ( -8.633843874998758494, 20.65557450359631630, -1.500000000000002220 ) ) ;
#95663 = ORIENTED_EDGE ( 'NONE', *, *, #93981, .F. ) ;
#95664 = VERTEX_POINT ( 'NONE', #1863 ) ;
#95665 = CARTESIAN_POINT ( 'NONE',  ( -34.52287095715006160, -23.47596703998600631, 11.44779298504229459 ) ) ;
#95666 = CARTESIAN_POINT ( 'NONE',  ( -128.6228709571500417, -29.50250243563736774, 8.947779886222132717 ) ) ;
#95667 = CARTESIAN_POINT ( 'NONE',  ( -40.17059228844927787, -25.31544866396273363, 5.061091936170584837 ) ) ;
#95668 = CARTESIAN_POINT ( 'NONE',  ( -125.5228709571500616, -23.48783264083375144, -1.443836473376139740 ) ) ;
#95669 = CARTESIAN_POINT ( 'NONE',  ( -97.25031873460709164, -24.47917135695840685, 9.440663514584127114 ) ) ;
#95670 = CARTESIAN_POINT ( 'NONE',  ( -19.52990877098713796, 1.257015143768854815, 11.49999999999998934 ) ) ;
#95671 = CARTESIAN_POINT ( 'NONE',  ( -49.51538943686712457, -25.28145962008399650, 4.090414597456915935 ) ) ;
#95672 = ORIENTED_EDGE ( 'NONE', *, *, #24448, .F. ) ;
#95673 = CARTESIAN_POINT ( 'NONE',  ( 2.436486579176012413, 21.40072447632485364, 11.49999999999998934 ) ) ;
#95674 = CARTESIAN_POINT ( 'NONE',  ( -128.5554938434827932, -24.51314013834317151, 0.6176544820404290537 ) ) ;
#95675 = CARTESIAN_POINT ( 'NONE',  ( -81.01373513877602761, -25.30394778790603638, 5.057100112635003697 ) ) ;
#95676 = CARTESIAN_POINT ( 'NONE',  ( -42.62287095715004881, -29.50250786944525672, 11.44777988621624232 ) ) ;
#95677 = CIRCLE ( 'NONE', #9763, 0.2499999999997798983 ) ;
#95678 = CARTESIAN_POINT ( 'NONE',  ( 29.70220533433691301, 6.376774720514426953, 28.20564067601639735 ) ) ;
#95679 = CARTESIAN_POINT ( 'NONE',  ( -14.98413761715186077, 17.36544542080599740, -1.500000000000002220 ) ) ;
#95680 = APPROVAL_ROLE ( '' ) ;
#95681 = PLANE ( 'NONE',  #62906 ) ;
#95682 = CARTESIAN_POINT ( 'NONE',  ( -53.53251464419344074, -24.65952944569304250, 1.056160979905695463 ) ) ;
#95683 = CARTESIAN_POINT ( 'NONE',  ( -10.05502934987021391, 17.38067806581081598, 11.49999999999999645 ) ) ;
#95684 = DIRECTION ( 'NONE',  ( 0.000000000000000000, -2.173523156925980399E-06, 0.9999999999976378895 ) ) ;
#95685 = CARTESIAN_POINT ( 'NONE',  ( -119.2228709571500644, -23.47593901973090169, -1.443836447538996426 ) ) ;
#95686 = CARTESIAN_POINT ( 'NONE',  ( 1.255616527394258553, 17.95615290467683778, 9.000000000000000000 ) ) ;
#95687 = CARTESIAN_POINT ( 'NONE',  ( -65.62287095715011276, -24.51163499207176244, 0.6490370598554294768 ) ) ;
#95688 = DIRECTION ( 'NONE',  ( -3.773278334453079618E-23, 0.9999999999976377785, 2.173523156925979975E-06 ) ) ;
#95689 = CARTESIAN_POINT ( 'NONE',  ( -3.387584560642538101, 19.54024307811383210, 11.49999999999998934 ) ) ;
#95690 = DIRECTION ( 'NONE',  ( 1.224646799147353207E-16, -1.000000000000000000, 0.000000000000000000 ) ) ;
#95691 = CARTESIAN_POINT ( 'NONE',  ( 15.15379598424239838, -12.58889634127381640, -1.500000000000002220 ) ) ;
#95692 = CARTESIAN_POINT ( 'NONE',  ( 16.15056352287343699, -5.152774720514406326, -27.77856273171769530 ) ) ;
#95693 = AXIS2_PLACEMENT_3D ( 'NONE', #91152, #28262, #91646 ) ;
#95694 = CARTESIAN_POINT ( 'NONE',  ( -54.52287095715006870, -23.48786465467240347, 11.44779295918255002 ) ) ;
#95695 = CIRCLE ( 'NONE', #51951, 1.149999999999998135 ) ;
#95696 = CARTESIAN_POINT ( 'NONE',  ( -115.6228709571499564, -24.51163499207178731, 0.6490370598555471604 ) ) ;
#95697 = DIRECTION ( 'NONE',  ( 0.000000000000000000, -0.9999999999976377785, -2.173523156925979128E-06 ) ) ;
#95698 = CARTESIAN_POINT ( 'NONE',  ( 20.58124611042576646, 0.8182449333618511123, 11.49999999999999645 ) ) ;
#95699 = CARTESIAN_POINT ( 'NONE',  ( -128.5228709571500758, -23.96177878511310055, 10.65340807706329507 ) ) ;
#95700 = AXIS2_PLACEMENT_3D ( 'NONE', #28389, #90296, #74083 ) ;
#95701 = CARTESIAN_POINT ( 'NONE',  ( 20.74359285767136640, 8.971229656761206428, 11.49999999999999645 ) ) ;
#95702 = ORIENTED_EDGE ( 'NONE', *, *, #6185, .T. ) ;
#95703 = LINE ( 'NONE', #33806, #7025 ) ;
#95705 = EDGE_CURVE ( 'NONE', #33400, #61899, #50531, .T. ) ;
#95704 = CARTESIAN_POINT ( 'NONE',  ( -56.52287095715009002, -24.51283580621365132, 0.6167428607019713738 ) ) ;
#95706 = CARTESIAN_POINT ( 'NONE',  ( -39.62287095715005592, -23.72747288104441665, -1.053458166803662888 ) ) ;
#95707 = EDGE_CURVE ( 'NONE', #15171, #41799, #14557, .T. ) ;
#95708 = CARTESIAN_POINT ( 'NONE',  ( -27.26363273317966573, -24.61460103318581716, 8.203483245735846197 ) ) ;
#95709 = ADVANCED_FACE ( 'NONE', ( #72878 ), #19571, .F. ) ;
#95710 = CARTESIAN_POINT ( 'NONE',  ( -97.62287095715005592, -29.50247984919015209, -1.443849546365050029 ) ) ;
#95711 = ADVANCED_FACE ( 'NONE', ( #94700 ), #69223, .F. ) ;
#95712 = ORIENTED_EDGE ( 'NONE', *, *, #80065, .F. ) ;
#95713 = CARTESIAN_POINT ( 'NONE',  ( -79.64180909446726275, -25.26749935932355484, 5.241605752690947639 ) ) ;
#95714 = CARTESIAN_POINT ( 'NONE',  ( 12.51456667378993259, 19.11410217522374921, 11.49999999999998934 ) ) ;
#95715 = CARTESIAN_POINT ( 'NONE',  ( -105.6228709571500417, -24.99132157543166954, 2.256160258750667502 ) ) ;
#95716 = CARTESIAN_POINT ( 'NONE',  ( -36.52287095715006870, -23.48783264082477018, -1.443836473390097019 ) ) ;
#95717 = CARTESIAN_POINT ( 'NONE',  ( -63.58339596546591821, -24.51419770103158058, 9.386484678747173405 ) ) ;
#95718 = CARTESIAN_POINT ( 'NONE',  ( 9.939345090160914609, -20.19931669485651682, 11.49999999999999645 ) ) ;
#95719 = ORIENTED_EDGE ( 'NONE', *, *, #78118, .F. ) ;
#95720 = FACE_OUTER_BOUND ( 'NONE', #98812, .T. ) ;
#95721 = CARTESIAN_POINT ( 'NONE',  ( 7.969717912702302343, -20.46423023992739942, 11.49999999999998934 ) ) ;
#95722 = CARTESIAN_POINT ( 'NONE',  ( 32.04341656622251122, 4.806217029847265287, -4.198923130344409671 ) ) ;
#95723 = CARTESIAN_POINT ( 'NONE',  ( -44.56898981399523763, -23.48786465467240347, 11.44779295918255357 ) ) ;
#95724 = CARTESIAN_POINT ( 'NONE',  ( -29.20082839157102583, -24.79699936332711729, 5.852070492749260389 ) ) ;
#95725 = ORIENTED_EDGE ( 'NONE', *, *, #12968, .T. ) ;
#95726 = EDGE_CURVE ( 'NONE', #2918, #64945, #66276, .T. ) ;
#95727 = DIRECTION ( 'NONE',  ( -0.000000000000000000, 2.173523156925979552E-06, -0.9999999999976378895 ) ) ;
#95728 = CARTESIAN_POINT ( 'NONE',  ( -107.5228709571501184, -23.95044443724992789, 10.65354141964649237 ) ) ;
#95729 = EDGE_LOOP ( 'NONE', ( #59447, #96133, #88262, #68600, #100088, #34216 ) ) ;
#95730 = CARTESIAN_POINT ( 'NONE',  ( -54.60549947881357014, -23.73791477778911130, 11.05961554403171299 ) ) ;
#95731 = CARTESIAN_POINT ( 'NONE',  ( -2.888065500968368227, -20.30684875360264741, -1.500000000000002220 ) ) ;
#95732 = ORIENTED_EDGE ( 'NONE', *, *, #9048, .F. ) ;
#95733 = ORIENTED_EDGE ( 'NONE', *, *, #58390, .F. ) ;
#95734 = VERTEX_POINT ( 'NONE', #22054 ) ;
#95735 = CARTESIAN_POINT ( 'NONE',  ( -50.24400751237210017, -25.31394886661938770, 5.202389599532529552 ) ) ;
#95736 = CARTESIAN_POINT ( 'NONE',  ( 22.28998074345494729, -6.091270044117925053, -1.500000000000002220 ) ) ;
#95737 = CARTESIAN_POINT ( 'NONE',  ( 14.83405752585509596, 4.881907540129173384, -27.54622755360215791 ) ) ;
#95738 = CARTESIAN_POINT ( 'NONE',  ( 18.28078834835902455, 8.925752885971231620, -1.500000000000002220 ) ) ;
#95739 = VERTEX_POINT ( 'NONE', #42931 ) ;
#95740 = DIRECTION ( 'NONE',  ( -3.773278334453079618E-23, 0.9999999999976377785, 2.173523156925979975E-06 ) ) ;
#95741 = CARTESIAN_POINT ( 'NONE',  ( -50.38191529551148307, -25.12049752546737835, 2.832404795212222659 ) ) ;
#95742 = PLANE ( 'NONE',  #27013 ) ;
#95743 = CARTESIAN_POINT ( 'NONE',  ( -57.62287095715004881, -23.48783264082478794, -1.443836473390068820 ) ) ;
#95744 = ORIENTED_EDGE ( 'NONE', *, *, #52988, .F. ) ;
#95745 = CARTESIAN_POINT ( 'NONE',  ( -28.74075323809458737, -24.76880966510508486, 2.791733147577219132 ) ) ;
#95746 = CARTESIAN_POINT ( 'NONE',  ( -49.69311491917191148, -25.26385837989523964, 4.912235144068747061 ) ) ;
#95747 = ORIENTED_EDGE ( 'NONE', *, *, #61451, .T. ) ;
#95748 = CARTESIAN_POINT ( 'NONE',  ( -9.565632364391108311, -18.43008791299702764, -1.500000000000002220 ) ) ;
#95749 = VECTOR ( 'NONE', #62066, 1000.000000000000000 ) ;
#95750 = ORIENTED_EDGE ( 'NONE', *, *, #36047, .T. ) ;
#95752 = VERTEX_POINT ( 'NONE', #21555 ) ;
#95751 = CARTESIAN_POINT ( 'NONE',  ( -125.5903909907711267, -24.15503026093915295, -0.2815557561904348804 ) ) ;
#95753 = CARTESIAN_POINT ( 'NONE',  ( -41.56077783461210373, -23.73791477778911485, 11.05961554403170766 ) ) ;
#95754 = CARTESIAN_POINT ( 'NONE',  ( -28.62287095715004881, -29.50248528299880846, 1.056150804693231082 ) ) ;
#95755 = VERTEX_POINT ( 'NONE', #90089 ) ;
#95756 = ORIENTED_EDGE ( 'NONE', *, *, #63140, .T. ) ;
#95757 = DIRECTION ( 'NONE',  ( 0.000000000000000000, -0.000000000000000000, 1.000000000000000000 ) ) ;
#95758 = CARTESIAN_POINT ( 'NONE',  ( -68.62287095715005592, -23.48786465467241058, 11.44779295918254647 ) ) ;
#95759 = CARTESIAN_POINT ( 'NONE',  ( -27.70544111104076990, -24.61528742064533049, 1.628749860405701799 ) ) ;
#95761 = ORIENTED_EDGE ( 'NONE', *, *, #12155, .T. ) ;
#95760 = CARTESIAN_POINT ( 'NONE',  ( -10.28628152547328511, -19.52461415289770130, 11.49999999999999645 ) ) ;
#95762 = CARTESIAN_POINT ( 'NONE',  ( -103.5151658127220458, -24.15543982623907482, -0.2315651400026619011 ) ) ;
#95763 = CARTESIAN_POINT ( 'NONE',  ( -9.785633969878258398, 20.35780147342342516, -1.500000000000002220 ) ) ;
#95764 = EDGE_CURVE ( 'NONE', #53793, #36016, #35255, .T. ) ;
#95766 = VERTEX_POINT ( 'NONE', #58644 ) ;
#95765 = CARTESIAN_POINT ( 'NONE',  ( -90.62287095715004170, -23.48783264082478794, -1.443836473390063713 ) ) ;
#95767 = VECTOR ( 'NONE', #97649, 1000.000000000000000 ) ;
#95768 = ORIENTED_EDGE ( 'NONE', *, *, #92605, .T. ) ;
#95769 = VECTOR ( 'NONE', #76735, 1000.000000000000227 ) ;
#95770 = CARTESIAN_POINT ( 'NONE',  ( -93.58953762381672448, -23.47593901973091235, -1.443836447539002865 ) ) ;
#95771 = B_SPLINE_CURVE_WITH_KNOTS ( 'NONE', 3,
 ( #66817, #12502, #22094, #52073 ),
 .UNSPECIFIED., .F., .F.,
 ( 4, 4 ),
 ( 0.8010720259253786280, 0.8100784571974942727 ),
 .UNSPECIFIED. ) ;
#95772 = ADVANCED_FACE ( 'NONE', ( #5848 ), #73866, .F. ) ;
#95773 = B_SPLINE_CURVE_WITH_KNOTS ( 'NONE', 3,
 ( #40756, #73217, #94537, #25023 ),
 .UNSPECIFIED., .F., .F.,
 ( 4, 4 ),
 ( 0.000000000000000000, 9.999999999998206125E-05 ),
 .UNSPECIFIED. ) ;
#95774 = PLANE ( 'NONE',  #27926 ) ;
#95775 = ORIENTED_EDGE ( 'NONE', *, *, #56915, .T. ) ;
#95776 = CARTESIAN_POINT ( 'NONE',  ( -1.756177585742932479, 21.11346882147791959, 11.49999999999998934 ) ) ;
#95777 = CARTESIAN_POINT ( 'NONE',  ( 30.63451081005166543, -4.279369518130740069, 28.08236555530620038 ) ) ;
#95778 = CARTESIAN_POINT ( 'NONE',  ( -6.905879715866854340, -6.376774720514411854, 19.48240003225459560 ) ) ;
#95779 = DIRECTION ( 'NONE',  ( 0.000000000000000000, 0.9999999999976377785, 2.173523156925979975E-06 ) ) ;
#95780 = CARTESIAN_POINT ( 'NONE',  ( -9.187330254778467875, -20.22999604658808082, -1.500000000000002220 ) ) ;
#95781 = DIRECTION ( 'NONE',  ( -0.9994733861282923959, 0.000000000000000000, -0.03244919754393515293 ) ) ;
#95782 = VERTEX_POINT ( 'NONE', #35315 ) ;
#95783 = CARTESIAN_POINT ( 'NONE',  ( 13.43165536947796213, 5.965225279485592225, -28.18099828186571187 ) ) ;
#95784 = PLANE ( 'NONE',  #10332 ) ;
#95785 = CARTESIAN_POINT ( 'NONE',  ( -36.59393400239565608, -24.15620529776627379, 10.23563542870660825 ) ) ;
#95786 = CARTESIAN_POINT ( 'NONE',  ( -49.62287095715005592, -24.66019654487199020, 8.947790411086135265 ) ) ;
#95787 = CARTESIAN_POINT ( 'NONE',  ( 10.22484414329051994, 16.58839404647166660, 11.49999999999998934 ) ) ;
#95788 = CARTESIAN_POINT ( 'NONE',  ( 11.41860910855227829, 18.14899599152127152, 11.49999999999998934 ) ) ;
#95789 = CARTESIAN_POINT ( 'NONE',  ( -56.62287095715007013, -24.33832256527049154, 0.1851278514138594566 ) ) ;
#95790 = CARTESIAN_POINT ( 'NONE',  ( -26.59970390766585169, -24.57999573590466014, 1.981117045598722370 ) ) ;
#95791 = DIRECTION ( 'NONE',  ( -1.000000000000000000, -0.000000000000000000, -0.000000000000000000 ) ) ;
#95792 = DIRECTION ( 'NONE',  ( 0.1489078231574191002, -6.845827386180410961E-16, -0.9888510809027407644 ) ) ;
#95793 = CARTESIAN_POINT ( 'NONE',  ( -7.854035805165779927, 21.33931789143995417, -1.500000000000002220 ) ) ;
#95794 = DIRECTION ( 'NONE',  ( -1.000000000000000000, -9.044818380534024011E-19, 3.498155517982143549E-15 ) ) ;
#95795 = CARTESIAN_POINT ( 'NONE',  ( -102.5508244618846163, -24.34968618360934656, 0.1864209137778959358 ) ) ;
#95796 = CARTESIAN_POINT ( 'NONE',  ( -101.5895376238167245, -24.66019654487199375, 8.947790411086133489 ) ) ;
#95797 = CARTESIAN_POINT ( 'NONE',  ( 19.88832268942539017, -0.5522253751840191516, 11.49999999999999645 ) ) ;
#95798 = CARTESIAN_POINT ( 'NONE',  ( -104.5951184837940531, -23.73766607897670866, -1.055555164236450016 ) ) ;
#95799 = DIRECTION ( 'NONE',  ( -3.773278334453079618E-23, 0.9999999999976377785, 2.173523156925979975E-06 ) ) ;
#95800 = CARTESIAN_POINT ( 'NONE',  ( -48.48929744942994802, -24.51314013834315375, 0.6176544820404137326 ) ) ;
#95801 = ORIENTED_EDGE ( 'NONE', *, *, #70981, .F. ) ;
#95802 = LINE ( 'NONE', #3968, #3995 ) ;
#95803 = LINE ( 'NONE', #11073, #37735 ) ;
#95804 = CARTESIAN_POINT ( 'NONE',  ( 18.84366469573077296, 10.75509914293975555, 11.49999999999998934 ) ) ;
#95805 = CARTESIAN_POINT ( 'NONE',  ( -67.55620429048339304, -24.65952944569304961, 1.056160979905695685 ) ) ;
#95806 = B_SPLINE_CURVE_WITH_KNOTS ( 'NONE', 3,
 ( #37782, #68736, #62128, #30666 ),
 .UNSPECIFIED., .F., .F.,
 ( 4, 4 ),
 ( 0.000000000000000000, 0.0001000000000000167422 ),
 .UNSPECIFIED. ) ;
#95807 = CARTESIAN_POINT ( 'NONE',  ( -3.206006181753352724, -19.19236486397402430, -1.500000000000002220 ) ) ;
#95808 = DIRECTION ( 'NONE',  ( -0.000000000000000000, 1.000000000000000000, -0.000000000000000000 ) ) ;
#95809 = VERTEX_POINT ( 'NONE', #68253 ) ;
#95810 = DATE_AND_TIME ( #96317, #52303 ) ;
#95811 = DIRECTION ( 'NONE',  ( 0.9975640502598243087, -0.06975647374412546897, -0.000000000000000000 ) ) ;
#95812 = CARTESIAN_POINT ( 'NONE',  ( -19.05221060042639536, -7.346018566486852031, 11.49999999999999645 ) ) ;
#95813 = DIRECTION ( 'NONE',  ( 1.000000000000000000, -0.000000000000000000, -0.000000000000000000 ) ) ;
#95814 = VECTOR ( 'NONE', #52608, 1000.000000000000114 ) ;
#95815 = CARTESIAN_POINT ( 'NONE',  ( -2.794871794871795156, -5.876774720514418071, 20.36318108974359475 ) ) ;
#95816 = ORIENTED_EDGE ( 'NONE', *, *, #1204, .F. ) ;
#95817 = CARTESIAN_POINT ( 'NONE',  ( -72.52287095715007581, -24.34917612406836795, 0.1852690917426531025 ) ) ;
#95818 = FACE_OUTER_BOUND ( 'NONE', #19569, .T. ) ;
#95819 = CARTESIAN_POINT ( 'NONE',  ( -39.18717306657202215, -25.27985411147982120, 4.881706710394202453 ) ) ;
#95820 = EDGE_CURVE ( 'NONE', #28727, #64178, #24273, .T. ) ;
#95821 = PLANE ( 'NONE',  #27945 ) ;
#95822 = DIRECTION ( 'NONE',  ( 0.000000000000000000, 0.9999999999976377785, 2.173523156925979975E-06 ) ) ;
#95824 = VERTEX_POINT ( 'NONE', #99182 ) ;
#95823 = EDGE_CURVE ( 'NONE', #41575, #56695, #12949, .T. ) ;
#95825 = DIRECTION ( 'NONE',  ( -0.000000000000000000, 1.000000000000000000, -0.000000000000000000 ) ) ;
#95826 = EDGE_CURVE ( 'NONE', #38350, #11878, #65460, .T. ) ;
#95827 = VECTOR ( 'NONE', #8436, 1000.000000000000000 ) ;
#95828 = CARTESIAN_POINT ( 'NONE',  ( -19.06187107478486098, -12.82570580458313003, 11.49999999999999645 ) ) ;
#95829 = CARTESIAN_POINT ( 'NONE',  ( 19.47892149737544187, 11.75266795981601753, 11.49999999999998934 ) ) ;
#95830 = CARTESIAN_POINT ( 'NONE',  ( 4.966987340572156739, -6.376774720514417183, 20.16530235339958210 ) ) ;
#95831 = EDGE_CURVE ( 'NONE', #98210, #42298, #50879, .T. ) ;
#95832 = LINE ( 'NONE', #26327, #39860 ) ;
#95833 = CARTESIAN_POINT ( 'NONE',  ( -90.58449521732619303, -24.83618233451450763, 1.606449574219535492 ) ) ;
#95834 = AXIS2_PLACEMENT_3D ( 'NONE', #95300, #80074, #49639 ) ;
#95835 = CARTESIAN_POINT ( 'NONE',  ( -125.5228709571500616, -23.47593901973090524, -1.443836447538996204 ) ) ;
#95836 = EDGE_CURVE ( 'NONE', #8339, #81218, #100159, .T. ) ;
#95837 = CARTESIAN_POINT ( 'NONE',  ( -70.01777984349551787, -25.14013070378048198, 7.061429261598838991 ) ) ;
#95838 = CARTESIAN_POINT ( 'NONE',  ( -11.18773875818744656, -18.78983145652188469, 11.49999999999998934 ) ) ;
#95839 = DIRECTION ( 'NONE',  ( 0.000000000000000000, 0.000000000000000000, -1.000000000000000000 ) ) ;
#95840 = B_SPLINE_CURVE_WITH_KNOTS ( 'NONE', 3,
 ( #4169, #37103, #58958, #20871, #35120, #68067 ),
 .UNSPECIFIED., .F., .F.,
 ( 4, 2, 4 ),
 ( 0.000000000000000000, 0.001380901958385388545, 0.002761803916770777089 ),
 .UNSPECIFIED. ) ;
#95841 = CARTESIAN_POINT ( 'NONE',  ( -26.42866040157690222, -24.83930146701730735, 3.123068956510520966 ) ) ;
#95842 = DIRECTION ( 'NONE',  ( -0.000000000000000000, -1.000000000000000000, -0.000000000000000000 ) ) ;
#95843 = CARTESIAN_POINT ( 'NONE',  ( -81.58953762381673869, -23.47593901973091235, -1.443836447539004642 ) ) ;
#95844 = ORIENTED_EDGE ( 'NONE', *, *, #52411, .T. ) ;
#95845 = B_SPLINE_CURVE_WITH_KNOTS ( 'NONE', 3,
 ( #12448, #66268, #13940, #97191, #28183, #89583, #29672, #58636 ),
 .UNSPECIFIED., .F., .F.,
 ( 4, 2, 2, 4 ),
 ( -0.001240355328176661687, -0.0002398155169397982525, 0.0007607242942970651820, 0.002761803916770787931 ),
 .UNSPECIFIED. ) ;
#95846 = CARTESIAN_POINT ( 'NONE',  ( -15.55180764702766716, 13.24544322234432414, 11.49999999999998934 ) ) ;
#95847 = VERTEX_POINT ( 'NONE', #92074 ) ;
#95848 = ORIENTED_EDGE ( 'NONE', *, *, #6354, .T. ) ;
#95849 = EDGE_CURVE ( 'NONE', #27638, #23749, #723, .T. ) ;
#95850 = CARTESIAN_POINT ( 'NONE',  ( 8.869223403490039459, -21.23658630136709391, -1.500000000000002220 ) ) ;
#95851 = DIRECTION ( 'NONE',  ( -3.773278334453079618E-23, 0.9999999999976377785, 2.173523156925979975E-06 ) ) ;
#95852 = ORIENTED_EDGE ( 'NONE', *, *, #19224, .F. ) ;
#95853 = CARTESIAN_POINT ( 'NONE',  ( -124.6228709571500701, -24.66019654487200086, 8.947790411086121054 ) ) ;
#95854 = CARTESIAN_POINT ( 'NONE',  ( -101.6228709571500559, -23.48783264082479505, -1.443836473390062380 ) ) ;
#95855 = DIRECTION ( 'NONE',  ( -0.000000000000000000, 0.000000000000000000, -1.000000000000000000 ) ) ;
#95856 = PLANE ( 'NONE',  #39940 ) ;
#95858 = ORIENTED_EDGE ( 'NONE', *, *, #28287, .T. ) ;
#95857 = CARTESIAN_POINT ( 'NONE',  ( 12.64048258313813733, 17.25876517447949610, 11.49999999999999645 ) ) ;
#95859 = ORIENTED_EDGE ( 'NONE', *, *, #88775, .T. ) ;
#95860 = CARTESIAN_POINT ( 'NONE',  ( -21.98633505697190671, -3.258044352128648846, 11.49999999999998934 ) ) ;
#95861 = CARTESIAN_POINT ( 'NONE',  ( 16.58470376584361361, 12.37529123428901556, -1.500000000000002220 ) ) ;
#95862 = VERTEX_POINT ( 'NONE', #22545 ) ;
#95863 = CARTESIAN_POINT ( 'NONE',  ( -115.6228709571500559, -29.50247984919015209, -1.443849546365046699 ) ) ;
#95864 = VECTOR ( 'NONE', #97142, 1000.000000000000000 ) ;
#95865 = CARTESIAN_POINT ( 'NONE',  ( 8.160000000000000142, -9.652339641703484574, -1.621096496867199033 ) ) ;
#95866 = ORIENTED_EDGE ( 'NONE', *, *, #2022, .F. ) ;
#95867 = CARTESIAN_POINT ( 'NONE',  ( -122.6228709571500417, -29.50248528299804818, 1.056150453629045360 ) ) ;
#95868 = ORIENTED_EDGE ( 'NONE', *, *, #2958, .F. ) ;
#95869 = CARTESIAN_POINT ( 'NONE',  ( -50.38191529551148307, -25.10935127036004033, 2.832404819438866017 ) ) ;
#95870 = CARTESIAN_POINT ( 'NONE',  ( 16.20321855003292555, -13.12800272717607619, -1.500000000000002220 ) ) ;
#95872 = EDGE_CURVE ( 'NONE', #33316, #15357, #30678, .T. ) ;
#95871 = CARTESIAN_POINT ( 'NONE',  ( 21.88901064076550185, 0.7357440816682787599, 11.49999999999999645 ) ) ;
#95873 = CARTESIAN_POINT ( 'NONE',  ( -107.6228709571500843, -24.51387760970725083, 9.387446482453409402 ) ) ;
#95874 = CARTESIAN_POINT ( 'NONE',  ( -61.24303308397303880, -25.03284409833926105, 7.563174216509380265 ) ) ;
#95875 = CARTESIAN_POINT ( 'NONE',  ( 16.80569330386292748, 14.95695114220347932, -1.500000000000002220 ) ) ;
#95876 = CARTESIAN_POINT ( 'NONE',  ( 11.32296221242833667, -17.63459971646239310, 11.49999999999998934 ) ) ;
#95877 = CARTESIAN_POINT ( 'NONE',  ( -26.09849696787948403, -24.97066838479807416, 5.165052413643238083 ) ) ;
#95878 = EDGE_CURVE ( 'NONE', #75528, #40241, #84461, .T. ) ;
#95879 = CARTESIAN_POINT ( 'NONE',  ( -53.52287095715006870, -24.64898659630367916, 1.056161002820821038 ) ) ;
#95880 = CARTESIAN_POINT ( 'NONE',  ( -88.62287095715004170, -23.47593901973091235, -1.443836447539002865 ) ) ;
#95881 = VERTEX_POINT ( 'NONE', #1242 ) ;
#95882 = ORIENTED_EDGE ( 'NONE', *, *, #51660, .F. ) ;
#95883 = ORIENTED_EDGE ( 'NONE', *, *, #53489, .T. ) ;
#95884 = VECTOR ( 'NONE', #53018, 1000.000000000000000 ) ;
#95885 = LINE ( 'NONE', #12138, #88723 ) ;
#95886 = ORIENTED_EDGE ( 'NONE', *, *, #2278, .F. ) ;
#95887 = CARTESIAN_POINT ( 'NONE',  ( 2.169945595249806125, 21.32849103866527329, -1.500000000000002220 ) ) ;
#95888 = EDGE_CURVE ( 'NONE', #93691, #78770, #53036, .T. ) ;
#95889 = ORIENTED_EDGE ( 'NONE', *, *, #12141, .T. ) ;
#95890 = DIRECTION ( 'NONE',  ( 0.000000000000000000, -1.000000000000000000, 0.000000000000000000 ) ) ;
#95891 = CARTESIAN_POINT ( 'NONE',  ( 7.532573551308565207, 19.69859070278346991, 11.49999999999998934 ) ) ;
#95892 = CARTESIAN_POINT ( 'NONE',  ( -61.55620429048340014, -23.47593901973091235, -1.443836447539007972 ) ) ;
#95893 = CARTESIAN_POINT ( 'NONE',  ( 2.745953332610513442, -6.376774720514418959, 21.05053573504278575 ) ) ;
#95894 = DIRECTION ( 'NONE',  ( -0.000000000000000000, -1.000000000000000000, 0.000000000000000000 ) ) ;
#95895 = CARTESIAN_POINT ( 'NONE',  ( -117.5228709571500758, -23.48783264082477729, -1.443836473390083697 ) ) ;
#95896 = FACE_OUTER_BOUND ( 'NONE', #40282, .T. ) ;
#95897 = CARTESIAN_POINT ( 'NONE',  ( 9.306852550357104903, -20.00191182576189064, -1.500000000000002220 ) ) ;
#95898 = ORIENTED_EDGE ( 'NONE', *, *, #2962, .T. ) ;
#95899 = CARTESIAN_POINT ( 'NONE',  ( -65.59839509469505003, -24.15602025860896518, 10.28564288303535257 ) ) ;
#95900 = EDGE_CURVE ( 'NONE', #6944, #21327, #63146, .T. ) ;
#95901 = DIRECTION ( 'NONE',  ( 0.000000000000000000, -2.173523156925980399E-06, 0.9999999999976378895 ) ) ;
#95902 = DIRECTION ( 'NONE',  ( 0.000000000000000000, 1.000000000000000000, 0.000000000000000000 ) ) ;
#95904 = B_SPLINE_CURVE_WITH_KNOTS ( 'NONE', 3,
 ( #303, #63220, #31247, #62218, #93138, #23621 ),
 .UNSPECIFIED., .F., .F.,
 ( 4, 2, 4 ),
 ( 1.570887131795413739E-05, 0.001396322306279768229, 0.002776935741241582344 ),
 .UNSPECIFIED. ) ;
#95903 = CARTESIAN_POINT ( 'NONE',  ( -62.49489557338270629, -24.51419770103156281, 9.386484678747184063 ) ) ;
#95905 = VECTOR ( 'NONE', #27040, 1000.000000000000114 ) ;
#95906 = PLANE ( 'NONE',  #94305 ) ;
#95907 = APPROVAL_PERSON_ORGANIZATION ( #63243, #32096, #54129 ) ;
#95908 = CARTESIAN_POINT ( 'NONE',  ( 11.98973536156539943, -2.682774720514426559, -26.26140391504922178 ) ) ;
#95909 = CARTESIAN_POINT ( 'NONE',  ( 20.65877813657638740, 5.380652674160894655, -1.500000000000002220 ) ) ;
#95910 = CARTESIAN_POINT ( 'NONE',  ( -104.5228709571500332, -24.35013146730204525, 9.818937971375099494 ) ) ;
#95911 = DIRECTION ( 'NONE',  ( -3.773278334453079030E-23, 0.9999999999976377785, 2.173523156925979128E-06 ) ) ;
#95912 = CARTESIAN_POINT ( 'NONE',  ( -64.65372345458705183, -23.48786465467241058, 11.44779295918254824 ) ) ;
#95913 = DIRECTION ( 'NONE',  ( -3.773278334453079618E-23, 0.9999999999976377785, 2.173523156925979975E-06 ) ) ;
#95914 = CC_DESIGN_PERSON_AND_ORGANIZATION_ASSIGNMENT ( #58011, #66131, ( #91188 ) ) ;
#95915 = CARTESIAN_POINT ( 'NONE',  ( 20.50669422456317292, -9.396423750077818937, -1.500000000000002220 ) ) ;
#95916 = CARTESIAN_POINT ( 'NONE',  ( -23.59123376470063960, -6.143225279485574397, 23.50402280011862288 ) ) ;
#95917 = ORIENTED_EDGE ( 'NONE', *, *, #1703, .F. ) ;
#95918 = CARTESIAN_POINT ( 'NONE',  ( 5.271800844963591359, 3.316774720514426456, -28.56638892015329745 ) ) ;
#95919 = CARTESIAN_POINT ( 'NONE',  ( -31.57476609544196933, -24.66019654487199020, 8.947790411086133489 ) ) ;
#95920 = CARTESIAN_POINT ( 'NONE',  ( 15.33752688427012778, 12.42672799324400934, 11.49999999999999645 ) ) ;
#95921 = CARTESIAN_POINT ( 'NONE',  ( -40.62287095715005592, -23.47593901973091235, -1.443836447539011525 ) ) ;
#95922 = CARTESIAN_POINT ( 'NONE',  ( -67.55938042207226601, -23.73766607897670511, -1.055555164236457788 ) ) ;
#95923 = B_SPLINE_CURVE_WITH_KNOTS ( 'NONE', 3,
 ( #47309, #24958, #77727, #25461 ),
 .UNSPECIFIED., .F., .F.,
 ( 4, 4 ),
 ( 0.5791858693580937967, 0.5801866163988591563 ),
 .UNSPECIFIED. ) ;
#95924 = VERTEX_POINT ( 'NONE', #24056 ) ;
#95925 = CARTESIAN_POINT ( 'NONE',  ( 9.948453975742596711, -5.965225279485574461, -28.04422933552663366 ) ) ;
#95926 = CARTESIAN_POINT ( 'NONE',  ( -99.62287095715004170, -24.66019654487199730, 8.947790411086122830 ) ) ;
#95927 = CARTESIAN_POINT ( 'NONE',  ( 31.79364159983995464, 2.682774720514426559, -11.59305536555894278 ) ) ;
#95928 = CARTESIAN_POINT ( 'NONE',  ( -20.99440926880444636, 4.982473936180791263, -1.500000000000002220 ) ) ;
#95929 = CARTESIAN_POINT ( 'NONE',  ( -71.52287095715007581, -23.47596703998600631, 11.44779298504228748 ) ) ;
#95930 = DIRECTION ( 'NONE',  ( 1.000000000000000000, -7.960204194457801640E-17, 0.000000000000000000 ) ) ;
#95931 = CARTESIAN_POINT ( 'NONE',  ( -68.62287095715005592, -24.64965695001468404, 8.947790433994184056 ) ) ;
#95932 = CARTESIAN_POINT ( 'NONE',  ( -97.62287095715005592, -29.50248528299804818, 1.056150453629042030 ) ) ;
#95933 = CARTESIAN_POINT ( 'NONE',  ( -19.30086548479123465, -4.275078920326023990, -1.500000000000002220 ) ) ;
#95934 = ORIENTED_EDGE ( 'NONE', *, *, #6030, .T. ) ;
#95935 = CARTESIAN_POINT ( 'NONE',  ( 9.670762957215185196, 17.83519281925787325, 11.49999999999999645 ) ) ;
#95936 = CARTESIAN_POINT ( 'NONE',  ( -7.491187506528125262, -5.876774720514410966, 19.53857357749109980 ) ) ;
#95937 = VECTOR ( 'NONE', #18146, 1000.000000000000114 ) ;
#95938 = VERTEX_POINT ( 'NONE', #61649 ) ;
#95939 = CARTESIAN_POINT ( 'NONE',  ( -46.52287095715006160, -23.47596703998600631, 11.44779298504229104 ) ) ;
#95940 = DIRECTION ( 'NONE',  ( -3.773278334453080206E-23, 0.9999999999976377785, 2.173523156925979975E-06 ) ) ;
#95941 = PLANE ( 'NONE',  #62260 ) ;
#95942 = CARTESIAN_POINT ( 'NONE',  ( -69.86226356453386188, -25.11033435731149055, 2.832404375966413479 ) ) ;
#95943 = DIRECTION ( 'NONE',  ( 0.000000000000000000, 0.9999999999976377785, 2.173523156925979975E-06 ) ) ;
#95944 = CARTESIAN_POINT ( 'NONE',  ( -32.68833172073793492, -25.11010177982458913, 2.831122766525575152 ) ) ;
#95946 = EDGE_CURVE ( 'NONE', #95739, #16907, #17079, .T. ) ;
#95945 = CARTESIAN_POINT ( 'NONE',  ( 15.05167116458888010, 13.23127732593390959, -1.500000000000002220 ) ) ;
#95947 = CYLINDRICAL_SURFACE ( 'NONE', #28859, 130.2784398600581710 ) ;
#95948 = ORIENTED_EDGE ( 'NONE', *, *, #73743, .F. ) ;
#95949 = CARTESIAN_POINT ( 'NONE',  ( -51.52287095715006870, -24.65952944569304606, 1.056160979905693686 ) ) ;
#95950 = VECTOR ( 'NONE', #95305, 1000.000000000000000 ) ;
#95951 = ADVANCED_FACE ( 'NONE', ( #7331 ), #76831, .F. ) ;
#95952 = CARTESIAN_POINT ( 'NONE',  ( -35.57730181162962424, -24.83618233451448987, 1.606449574219547261 ) ) ;
#95953 = CARTESIAN_POINT ( 'NONE',  ( -52.52287095715006870, -24.64898659630367916, 1.056161002820821038 ) ) ;
#95954 = AXIS2_PLACEMENT_3D ( 'NONE', #71114, #45766, #32543 ) ;
#95955 = EDGE_CURVE ( 'NONE', #10587, #77573, #42442, .T. ) ;
#95956 = CARTESIAN_POINT ( 'NONE',  ( -105.5228709571500616, -24.51163499207175178, 0.6490370598554284776 ) ) ;
#95957 = DIRECTION ( 'NONE',  ( 0.000000000000000000, 0.000000000000000000, -1.000000000000000000 ) ) ;
#95958 = B_SPLINE_CURVE_WITH_KNOTS ( 'NONE', 3,
 ( #98629, #4805, #27143, #97639 ),
 .UNSPECIFIED., .F., .F.,
 ( 4, 4 ),
 ( 0.000000000000000000, 9.999999999998897304E-05 ),
 .UNSPECIFIED. ) ;
#95959 = B_SPLINE_CURVE_WITH_KNOTS ( 'NONE', 3,
 ( #25748, #910, #56215, #1920, #64341, #64847, #16622, #24736, #25240, #87144, #10518, #55215, #94251, #17633, #2420 ),
 .UNSPECIFIED., .F., .F.,
 ( 4, 1, 1, 1, 1, 1, 1, 1, 1, 1, 1, 1, 4 ),
 ( 0.000000000000000000, 0.07176606415833990116, 0.1412255357663689537, 0.2091158524974625343, 0.2748396534685271231, 0.3394829303752209260, 0.4024762667353996570, 0.4649418891713271162, 0.5268326406463837985, 0.6474148160608227398, 0.7655615117859490004, 0.8816150870393316685, 1.000000000000000000 ),
 .UNSPECIFIED. ) ;
#95960 = CARTESIAN_POINT ( 'NONE',  ( -0.02075734969026423599, 0.3587747205144213303, -0.08597719988137648983 ) ) ;
#95961 = DIRECTION ( 'NONE',  ( -1.000000000000000000, -3.773278334444166432E-23, -8.201307841325785021E-29 ) ) ;
#95962 = ORIENTED_EDGE ( 'NONE', *, *, #11523, .F. ) ;
#95963 = CARTESIAN_POINT ( 'NONE',  ( -19.79944955726156763, -4.570829099900970860, 11.49999999999998934 ) ) ;
#95964 = EDGE_LOOP ( 'NONE', ( #19214, #24600, #14204, #65601 ) ) ;
#95965 = EDGE_CURVE ( 'NONE', #14117, #74994, #89699, .T. ) ;
#95966 = CARTESIAN_POINT ( 'NONE',  ( 31.61046577166746374, 4.540774708561928108, 26.28065669267635585 ) ) ;
#95967 = CARTESIAN_POINT ( 'NONE',  ( -118.5895376238167387, -23.47596703998600631, 11.44779298504227683 ) ) ;
#95968 = ORIENTED_EDGE ( 'NONE', *, *, #39225, .T. ) ;
#95969 = CARTESIAN_POINT ( 'NONE',  ( -59.58301786718180892, -24.51419770103156281, 9.386484678747184063 ) ) ;
#95970 = CARTESIAN_POINT ( 'NONE',  ( -49.39546678031889826, -25.12215307982809875, 6.587942430398275206 ) ) ;
#95971 = VECTOR ( 'NONE', #36126, 1000.000000000000227 ) ;
#95972 = CARTESIAN_POINT ( 'NONE',  ( -30.47287095715007865, -24.48778984439529793, 0.5888598878604692777 ) ) ;
#95973 = CARTESIAN_POINT ( 'NONE',  ( -10.79823215447539653, -18.26288818932900071, 11.49999999999999645 ) ) ;
#95974 = CC_DESIGN_APPROVAL ( #92807, ( #97564 ) ) ;
#95975 = CARTESIAN_POINT ( 'NONE',  ( -17.14978611337857473, 13.99085498846200437, 11.49999999999998934 ) ) ;
#95976 = CARTESIAN_POINT ( 'NONE',  ( 14.30100545221680441, -14.83292283143518375, -1.500000000000002220 ) ) ;
#95977 = ORIENTED_EDGE ( 'NONE', *, *, #58390, .T. ) ;
#95978 = CARTESIAN_POINT ( 'NONE',  ( -41.50561517559466296, -23.96119346886880663, -0.6495511937831991434 ) ) ;
#95979 = ORIENTED_EDGE ( 'NONE', *, *, #83651, .T. ) ;
#95980 = CARTESIAN_POINT ( 'NONE',  ( -54.65829041126421117, -23.48783264082476308, -1.443836473390098130 ) ) ;
#95981 = DIRECTION ( 'NONE',  ( 0.000000000000000000, -0.9999999999976377785, -2.173523156925979128E-06 ) ) ;
#95982 = ORIENTED_EDGE ( 'NONE', *, *, #71850, .F. ) ;
#95983 = ORIENTED_EDGE ( 'NONE', *, *, #87134, .F. ) ;
#95984 = ORIENTED_EDGE ( 'NONE', *, *, #95268, .F. ) ;
#95985 = AXIS2_PLACEMENT_3D ( 'NONE', #6906, #15508, #46473 ) ;
#95986 = CARTESIAN_POINT ( 'NONE',  ( 8.071512145086531476, -9.528487854913507249, -1.499999999999996891 ) ) ;
#95987 = DIRECTION ( 'NONE',  ( 0.000000000000000000, -2.173523156925979552E-06, 0.9999999999976378895 ) ) ;
#95988 = LINE ( 'NONE', #57450, #1750 ) ;
#95989 = CARTESIAN_POINT ( 'NONE',  ( 2.909938941155331360, -20.50406750007545398, -1.500000000000002220 ) ) ;
#95990 = B_SPLINE_CURVE_WITH_KNOTS ( 'NONE', 3,
 ( #59267, #90213, #19686, #66404, #50166, #89220, #43051, #4490, #35437, #51154, #13073, #90711, #20189, #19194, #97327, #74971, #27814, #82103, #34930 ),
 .UNSPECIFIED., .F., .F.,
 ( 4, 1, 1, 1, 1, 1, 1, 1, 1, 1, 1, 1, 1, 1, 1, 1, 4 ),
 ( 0.000000000000000000, 0.06113791491562318298, 0.1199938438512138800, 0.1782253215076183839, 0.2362564202618999687, 0.2949293769549112820, 0.3547157488097555933, 0.4167296639241647727, 0.4806644084708298625, 0.5458317702108677061, 0.6097581054261674849, 0.6729712284742227490, 0.7360168691676642894, 0.7998393981920319806, 0.8647753566655687063, 0.9310876232725688872, 1.000000000000000000 ),
 .UNSPECIFIED. ) ;
#95991 = CARTESIAN_POINT ( 'NONE',  ( -2.129050106866105185, 21.58297100922832357, 11.49999999999999645 ) ) ;
#95992 = ORIENTED_EDGE ( 'NONE', *, *, #58768, .T. ) ;
#95993 = CARTESIAN_POINT ( 'NONE',  ( -69.86226847989213695, -25.12049686670126292, 2.832401160916445004 ) ) ;
#95994 = CARTESIAN_POINT ( 'NONE',  ( -28.58953762381671737, -23.32893085120693044, 11.44779297967261478 ) ) ;
#95995 = CARTESIAN_POINT ( 'NONE',  ( 12.67250375155129127, 18.46511205475877304, -1.500000000000002220 ) ) ;
#95996 = B_SPLINE_CURVE_WITH_KNOTS ( 'NONE', 3,
 ( #39408, #31800, #62768, #93686, #55149, #86078 ),
 .UNSPECIFIED., .F., .F.,
 ( 4, 2, 4 ),
 ( 1.570887131794952276E-05, 0.001396322306279762808, 0.002776935741241575838 ),
 .UNSPECIFIED. ) ;
#95997 = DIRECTION ( 'NONE',  ( -1.000000000000000000, -0.000000000000000000, -0.000000000000000000 ) ) ;
#95998 = CARTESIAN_POINT ( 'NONE',  ( -71.62287095715005592, -23.48783264082478084, -1.443836473390067487 ) ) ;
#96000 = ORIENTED_EDGE ( 'NONE', *, *, #68012, .T. ) ;
#95999 = EDGE_CURVE ( 'NONE', #97756, #33587, #84826, .T. ) ;
#96001 = CARTESIAN_POINT ( 'NONE',  ( -121.5228709571500616, -23.48786465467241769, 11.44779295918253759 ) ) ;
#96002 = FACE_OUTER_BOUND ( 'NONE', #65319, .T. ) ;
#96003 = B_SPLINE_SURFACE_WITH_KNOTS ( 'NONE', 3, 3, ( 
 ( #95980, #49830, #26966, #10240 ),
 ( #19351, #64562, #73646, #24960 ),
 ( #48316, #25967, #79243, #2150 ),
 ( #65562, #42221, #50317, #17859 ),
 ( #72156, #33083, #73154, #3644 ),
 ( #64062, #48823, #57443, #34590 ),
 ( #3151, #94974, #96477, #88879 ) ),
 .UNSPECIFIED., .F., .F., .F.,
 ( 4, 3, 4 ),
 ( 4, 4 ),
 ( 0.0004766839783814135812, 0.1029713700210890814, 0.2054660560637967537 ),
 ( 0.7596872487054024958, 0.7610504915621147948 ),
 .UNSPECIFIED. ) ;
#96004 = VERTEX_POINT ( 'NONE', #87466 ) ;
#96005 = ORIENTED_EDGE ( 'NONE', *, *, #52866, .F. ) ;
#96006 = DIRECTION ( 'NONE',  ( -1.000000000000000000, 0.000000000000000000, 0.000000000000000000 ) ) ;
#96007 = EDGE_LOOP ( 'NONE', ( #10400, #97968, #14319, #33567 ) ) ;
#96008 = ADVANCED_FACE ( 'NONE', ( #11345 ), #48415, .F. ) ;
#96009 = AXIS2_PLACEMENT_3D ( 'NONE', #1328, #69328, #78928 ) ;
#96010 = CARTESIAN_POINT ( 'NONE',  ( -19.98547761299008130, 7.154247560337752887, -1.500000000000002220 ) ) ;
#96011 = ORIENTED_EDGE ( 'NONE', *, *, #53172, .F. ) ;
#96012 = CARTESIAN_POINT ( 'NONE',  ( -88.50298424756591942, -24.65952944569304606, 1.056160979905701902 ) ) ;
#96013 = CARTESIAN_POINT ( 'NONE',  ( 8.176594470695947692, -20.27425322898990601, 11.49999999999998934 ) ) ;
#96014 = CARTESIAN_POINT ( 'NONE',  ( -103.5929781363113591, -23.96169478059713498, 10.65365249895717881 ) ) ;
#96015 = CARTESIAN_POINT ( 'NONE',  ( -12.65407072091355722, -6.376774720514426953, -26.15404995688569301 ) ) ;
#96016 = FACE_OUTER_BOUND ( 'NONE', #51813, .T. ) ;
#96017 = CARTESIAN_POINT ( 'NONE',  ( 12.52028139621776326, 17.89958603277719718, -1.500000000000002220 ) ) ;
#96018 = CARTESIAN_POINT ( 'NONE',  ( 7.111284305517425075, -6.376774720514422512, 21.05363841023157434 ) ) ;
#96019 = ORIENTED_EDGE ( 'NONE', *, *, #28187, .T. ) ;
#96020 = PLANE ( 'NONE',  #87503 ) ;
#96021 = CARTESIAN_POINT ( 'NONE',  ( -5.366453405989236813, 0.000000000000000000, 0.000000000000000000 ) ) ;
#96022 = ORIENTED_EDGE ( 'NONE', *, *, #57037, .T. ) ;
#96023 = CARTESIAN_POINT ( 'NONE',  ( -30.58316948069863628, -25.14456584033169051, 2.729964928219756004 ) ) ;
#96024 = VERTEX_POINT ( 'NONE', #26066 ) ;
#96025 = VECTOR ( 'NONE', #36779, 1000.000000000000114 ) ;
#96026 = LINE ( 'NONE', #58478, #62151 ) ;
#96027 = CARTESIAN_POINT ( 'NONE',  ( -82.50023227949210991, -24.65952944569304606, 1.056160979905703012 ) ) ;
#96028 = CARTESIAN_POINT ( 'NONE',  ( -1.624102159174229731, 21.17438964843747584, 11.49999999999998934 ) ) ;
#96029 = CARTESIAN_POINT ( 'NONE',  ( 10.46399479596396453, 2.682774720514426559, -27.03001098546561920 ) ) ;
#96030 = CARTESIAN_POINT ( 'NONE',  ( -30.63208233338743725, -23.87624887660336981, 11.01174216661999594 ) ) ;
#96031 = EDGE_CURVE ( 'NONE', #57803, #93401, #96087, .T. ) ;
#96032 = CARTESIAN_POINT ( 'NONE',  ( 29.73860345376319358, 4.772803916115708311, -4.021109907510727943 ) ) ;
#96033 = CARTESIAN_POINT ( 'NONE',  ( -68.65187207870859254, -23.48783264082476308, -1.443836473390094799 ) ) ;
#96034 = EDGE_CURVE ( 'NONE', #89278, #21561, #15814, .T. ) ;
#96035 = CARTESIAN_POINT ( 'NONE',  ( -16.37229413335033001, -10.43475415037859655, 11.49999999999998934 ) ) ;
#96036 = LINE ( 'NONE', #94529, #78170 ) ;
#96037 = ORIENTED_EDGE ( 'NONE', *, *, #69523, .F. ) ;
#96038 = CARTESIAN_POINT ( 'NONE',  ( 14.28107258077893604, -13.35224110012613963, 11.49999999999999645 ) ) ;
#96039 = CARTESIAN_POINT ( 'NONE',  ( -5.576843645946834016, -5.876774720514417183, 20.41272575174755133 ) ) ;
#96040 = DIRECTION ( 'NONE',  ( 0.000000000000000000, -1.084202172485504434E-16, -1.000000000000000000 ) ) ;
#96041 = ORIENTED_EDGE ( 'NONE', *, *, #97731, .F. ) ;
#96042 = CARTESIAN_POINT ( 'NONE',  ( -97.52287095715009002, -23.73907113216990084, -1.053371485793246576 ) ) ;
#96043 = ADVANCED_FACE ( 'NONE', ( #63652 ), #26577, .T. ) ;
#96044 = DIRECTION ( 'NONE',  ( -3.773278334453079618E-23, 0.9999999999976377785, 2.173523156925979975E-06 ) ) ;
#96045 = EDGE_CURVE ( 'NONE', #39879, #79654, #1276, .T. ) ;
#96046 = CARTESIAN_POINT ( 'NONE',  ( 0.000000000000000000, -2.056774720514426669, 0.000000000000000000 ) ) ;
#96047 = VECTOR ( 'NONE', #91304, 1000.000000000000114 ) ;
#96048 = CARTESIAN_POINT ( 'NONE',  ( -81.34205133964172774, -25.24813932869157540, 7.294265035158486121 ) ) ;
#96049 = CARTESIAN_POINT ( 'NONE',  ( -3.718233408413001762, 19.32670252783854536, -1.500000000000002220 ) ) ;
#96050 = ADVANCED_FACE ( 'NONE', ( #79847 ), #10848, .F. ) ;
#96052 = ORIENTED_EDGE ( 'NONE', *, *, #86793, .T. ) ;
#96051 = PRODUCT_DEFINITION_FORMATION_WITH_SPECIFIED_SOURCE ( 'ANY', '', #5326, .NOT_KNOWN. ) ;
#96053 = LINE ( 'NONE', #40763, #42405 ) ;
#96054 = DIRECTION ( 'NONE',  ( 0.000000000000000000, 0.000000000000000000, -1.000000000000000000 ) ) ;
#96055 = B_SPLINE_CURVE_WITH_KNOTS ( 'NONE', 3,
 ( #62555, #9251, #93479, #79260, #23972, #54942, #85883, #47328 ),
 .UNSPECIFIED., .F., .F.,
 ( 4, 2, 2, 4 ),
 ( 0.000000000000000000, 0.002001079623178226262, 0.003001619434767339393, 0.004002159246356452524 ),
 .UNSPECIFIED. ) ;
#96056 = CIRCLE ( 'NONE', #28044, 28.96799999999999287 ) ;
#96057 = CALENDAR_DATE ( 2026, 9, 10 ) ;
#96058 = ORIENTED_EDGE ( 'NONE', *, *, #23875, .F. ) ;
#96059 = CARTESIAN_POINT ( 'NONE',  ( 3.557932825399831689, -5.876774720514428729, 21.44518044978141091 ) ) ;
#96060 = CARTESIAN_POINT ( 'NONE',  ( -59.92287095715006728, -23.47596703998600276, 11.44779298504227860 ) ) ;
#96061 = CARTESIAN_POINT ( 'NONE',  ( -52.62287095715005592, -23.47593901973091235, -1.443836447539009749 ) ) ;
#96062 = CARTESIAN_POINT ( 'NONE',  ( -97.58474207598447947, -24.66019654487199730, 8.947790411086115725 ) ) ;
#96063 = FACE_OUTER_BOUND ( 'NONE', #79600, .T. ) ;
#96064 = CARTESIAN_POINT ( 'NONE',  ( -69.57050707393172218, -25.31201661394681324, 5.639419279061749890 ) ) ;
#96065 = AXIS2_PLACEMENT_3D ( 'NONE', #37493, #28882, #89787 ) ;
#96066 = CARTESIAN_POINT ( 'NONE',  ( -114.5222273195970075, -23.48786465467241413, 11.44779295918253581 ) ) ;
#96068 = EDGE_CURVE ( 'NONE', #98443, #46565, #11174, .T. ) ;
#96067 = CARTESIAN_POINT ( 'NONE',  ( 6.088051586893210576, -19.00464151315268424, 11.49999999999998934 ) ) ;
#96069 = CARTESIAN_POINT ( 'NONE',  ( -75.62366547609374834, -25.00182538069147142, 7.747789668545045139 ) ) ;
#96070 = CARTESIAN_POINT ( 'NONE',  ( -18.24115112668064853, 7.888873183027880209, -1.500000000000002220 ) ) ;
#96071 = ORIENTED_EDGE ( 'NONE', *, *, #61711, .F. ) ;
#96072 = CARTESIAN_POINT ( 'NONE',  ( -28.62287095715006302, -23.33147402473456822, -1.443835808584760683 ) ) ;
#96073 = CARTESIAN_POINT ( 'NONE',  ( -104.6228709571500133, -24.33927499327854704, 9.819080762295815390 ) ) ;
#96074 = FACE_OUTER_BOUND ( 'NONE', #42480, .T. ) ;
#96075 = CARTESIAN_POINT ( 'NONE',  ( 10.16466294932649106, -6.376774720514429617, -24.98589889747637116 ) ) ;
#96076 = CARTESIAN_POINT ( 'NONE',  ( -12.40256906124370673, -16.71776976679197801, 11.49999999999999645 ) ) ;
#96077 = CARTESIAN_POINT ( 'NONE',  ( -35.62287095715005592, -23.47593901973091235, -1.443836447539011525 ) ) ;
#96078 = B_SPLINE_CURVE_WITH_KNOTS ( 'NONE', 3,
 ( #90118, #73407, #81012, #36334, #12492, #89126 ),
 .UNSPECIFIED., .F., .F.,
 ( 4, 2, 4 ),
 ( 0.000000000000000000, 0.001380764517854769302, 0.002761529035709538605 ),
 .UNSPECIFIED. ) ;
#96079 = EDGE_CURVE ( 'NONE', #3121, #86407, #81062, .T. ) ;
#96080 = CARTESIAN_POINT ( 'NONE',  ( -60.52287095715006160, -23.47593901973090169, -1.443836447538996870 ) ) ;
#96081 = CARTESIAN_POINT ( 'NONE',  ( -15.12447472116105729, 17.10960193589383849, 11.49999999999999645 ) ) ;
#96082 = AXIS2_PLACEMENT_3D ( 'NONE', #96176, #73340, #11929 ) ;
#96083 = EDGE_LOOP ( 'NONE', ( #49274, #3807, #97039, #12482 ) ) ;
#96084 = B_SPLINE_SURFACE_WITH_KNOTS ( 'NONE', 3, 1, ( 
 ( #16583, #39437 ),
 ( #70385, #84102 ),
 ( #92214, #22687 ),
 ( #99804, #68880 ),
 ( #54179, #100303 ),
 ( #77973, #30312 ),
 ( #53673, #875 ),
 ( #1386, #69885 ),
 ( #32320, #61787 ),
 ( #7472, #70895 ),
 ( #62286, #76478 ),
 ( #84605, #6984 ),
 ( #15092, #46059 ),
 ( #54670, #38432 ),
 ( #8487, #47059 ) ),
 .UNSPECIFIED., .F., .F., .F.,
 ( 4, 1, 1, 1, 1, 1, 1, 1, 1, 1, 1, 1, 4 ),
 ( 2, 2 ),
 ( 0.000000000000000000, 0.1041667992898066553, 0.1978560952899005576, 0.2832345117281488411, 0.3600126653135328203, 0.4338442080180757721, 0.5095057223304334526, 0.5870428909783838023, 0.6687538545127389433, 0.7511636688534690798, 0.8334676797015410088, 0.9158479811556834438, 1.000000000000000000 ),
 ( 0.000000000000000000, 1.000000000000000000 ),
 .UNSPECIFIED. ) ;
#96085 = CARTESIAN_POINT ( 'NONE',  ( -62.62287095715002039, -23.94994826722515313, -0.6494450866351701990 ) ) ;
#96086 = EDGE_CURVE ( 'NONE', #6944, #72067, #15631, .T. ) ;
#96087 = LINE ( 'NONE', #48918, #20862 ) ;
#96088 = ORIENTED_EDGE ( 'NONE', *, *, #51851, .F. ) ;
#96089 = CARTESIAN_POINT ( 'NONE',  ( 12.15850541088210868, 16.18036119754114566, 11.49999999999998934 ) ) ;
#96090 = CARTESIAN_POINT ( 'NONE',  ( -106.5228709571500332, -24.51387760970726148, 9.387446482453402297 ) ) ;
#96091 = ADVANCED_FACE ( 'NONE', ( #80859 ), #17450, .T. ) ;
#96092 = DIRECTION ( 'NONE',  ( -0.000000000000000000, 2.173523156925979552E-06, -0.9999999999976378895 ) ) ;
#96093 = VECTOR ( 'NONE', #81399, 1000.000000000000000 ) ;
#96094 = EDGE_CURVE ( 'NONE', #5560, #8268, #2244, .T. ) ;
#96095 = CARTESIAN_POINT ( 'NONE',  ( -28.98875734969026396, 5.965225279485572685, 7.870022800118625206 ) ) ;
#96096 = ORIENTED_EDGE ( 'NONE', *, *, #12415, .F. ) ;
#96097 = CARTESIAN_POINT ( 'NONE',  ( -109.6228709571500559, -24.64965695001469115, 8.947790433994176951 ) ) ;
#96098 = DIRECTION ( 'NONE',  ( -0.9951627101165078093, -0.09824042138329590335, 0.000000000000000000 ) ) ;
#96099 = CARTESIAN_POINT ( 'NONE',  ( 19.63333621495807435, 3.783328549194958867, -1.500000000000002220 ) ) ;
#96100 = AXIS2_PLACEMENT_3D ( 'NONE', #10206, #41163, #72117 ) ;
#96101 = CARTESIAN_POINT ( 'NONE',  ( -5.787726610425443674, -20.20099407548119075, 11.49999999999999645 ) ) ;
#96102 = CARTESIAN_POINT ( 'NONE',  ( 7.207151257207165429, 5.965225279485574461, -28.24477140324590252 ) ) ;
#96103 = DIRECTION ( 'NONE',  ( -1.000000000000000000, -0.000000000000000000, 0.000000000000000000 ) ) ;
#96104 = CARTESIAN_POINT ( 'NONE',  ( -0.5447568859041533873, -22.05808898580190558, 11.49999999999998934 ) ) ;
#96105 = CARTESIAN_POINT ( 'NONE',  ( -40.38104457131870362, -25.27806106493511251, 5.081426816473861408 ) ) ;
#96106 = ORIENTED_EDGE ( 'NONE', *, *, #57726, .F. ) ;
#96107 = PLANE ( 'NONE',  #98638 ) ;
#96108 = CARTESIAN_POINT ( 'NONE',  ( 33.12653832968937451, -6.376774720514426953, -7.315055336576590683 ) ) ;
#96109 = CARTESIAN_POINT ( 'NONE',  ( -72.59232901061996301, -24.15543982623907127, -0.2315651400026661755 ) ) ;
#96110 = CARTESIAN_POINT ( 'NONE',  ( 13.91401389203221406, -5.965225279485572685, 27.75920385068456042 ) ) ;
#96111 = EDGE_LOOP ( 'NONE', ( #32953, #42121, #22483, #90141 ) ) ;
#96112 = ORIENTED_EDGE ( 'NONE', *, *, #92591, .F. ) ;
#96113 = CARTESIAN_POINT ( 'NONE',  ( 0.000000000000000000, 1.826774720514426464, 6.000000000000000888 ) ) ;
#96114 = CARTESIAN_POINT ( 'NONE',  ( -100.7878122855614293, -25.10935811319381372, 2.873140115367836867 ) ) ;
#96115 = FACE_OUTER_BOUND ( 'NONE', #82511, .T. ) ;
#96116 = CARTESIAN_POINT ( 'NONE',  ( -4.863915844574979275, 19.94883092034378791, -1.500000000000002220 ) ) ;
#96117 = ORIENTED_EDGE ( 'NONE', *, *, #11760, .F. ) ;
#96118 = CARTESIAN_POINT ( 'NONE',  ( -10.24059822343752479, -6.376774720514426953, -2.394817856121274864E-14 ) ) ;
#96119 = DIRECTION ( 'NONE',  ( 0.000000000000000000, 0.000000000000000000, -1.000000000000000000 ) ) ;
#96120 = LINE ( 'NONE', #17991, #99889 ) ;
#96121 = CARTESIAN_POINT ( 'NONE',  ( 19.83320176327591255, -10.20924650237717835, 11.49999999999998934 ) ) ;
#96123 = CARTESIAN_POINT ( 'NONE',  ( -114.6228709571500559, -29.50250243563736774, 8.947779886222136270 ) ) ;
#96122 = AXIS2_PLACEMENT_3D ( 'NONE', #11695, #88840, #80217 ) ;
#96125 = ADVANCED_FACE ( 'NONE', ( #41295 ), #2745, .T. ) ;
#96124 = CARTESIAN_POINT ( 'NONE',  ( -6.660000000000001030, -9.074990544709798712, -0.7360493640965779516 ) ) ;
#96126 = EDGE_LOOP ( 'NONE', ( #85081, #74991, #22446, #85373 ) ) ;
#96127 = CARTESIAN_POINT ( 'NONE',  ( 33.28704981706498955, -4.441298812401576868, -11.58844794911118647 ) ) ;
#96128 = CARTESIAN_POINT ( 'NONE',  ( -96.62287095715005592, -23.48786465467241413, 11.44779295918254114 ) ) ;
#96129 = SECURITY_CLASSIFICATION ( '', '', #95195 ) ;
#96130 = CARTESIAN_POINT ( 'NONE',  ( 20.80141654084381386, -1.409215765453083469, -1.500000000000002220 ) ) ;
#96131 = EDGE_LOOP ( 'NONE', ( #2013, #14864, #30958, #41885 ) ) ;
#96133 = ORIENTED_EDGE ( 'NONE', *, *, #38917, .T. ) ;
#96132 = CARTESIAN_POINT ( 'NONE',  ( 14.85834502026402681, -2.682774720514426559, -27.37203305628894867 ) ) ;
#96134 = VERTEX_POINT ( 'NONE', #64157 ) ;
#96135 = CIRCLE ( 'NONE', #92918, 1.325999999999943446 ) ;
#96136 = ADVANCED_FACE ( 'NONE', ( #95081 ), #22618, .T. ) ;
#96137 = CARTESIAN_POINT ( 'NONE',  ( -69.21490423241783674, -25.03149257829292651, 7.033986958848029047 ) ) ;
#96138 = CARTESIAN_POINT ( 'NONE',  ( -19.04630365209304799, -9.011775662611203330, -1.500000000000002220 ) ) ;
#96139 = ORIENTED_EDGE ( 'NONE', *, *, #28139, .F. ) ;
#96140 = LINE ( 'NONE', #97129, #91577 ) ;
#96141 = DIRECTION ( 'NONE',  ( -0.000000000000000000, -0.000000000000000000, -1.000000000000000000 ) ) ;
#96142 = DIRECTION ( 'NONE',  ( 0.000000000000000000, -0.9999999999976377785, -2.173523156925979975E-06 ) ) ;
#96143 = AXIS2_PLACEMENT_3D ( 'NONE', #25384, #80175, #96397 ) ;
#96144 = CARTESIAN_POINT ( 'NONE',  ( -101.3347705957103528, -25.03152393472591797, 7.306917963305517461 ) ) ;
#96145 = CARTESIAN_POINT ( 'NONE',  ( -83.92287095715005307, -23.47593901973090169, -1.443836447538996870 ) ) ;
#96146 = CARTESIAN_POINT ( 'NONE',  ( -17.53059066697263546, 12.75712217820542627, -1.500000000000002220 ) ) ;
#96147 = CARTESIAN_POINT ( 'NONE',  ( -80.72310326078591913, -25.24759799559129192, 7.076933208677574250 ) ) ;
#96149 = ORIENTED_EDGE ( 'NONE', *, *, #98707, .T. ) ;
#96148 = CARTESIAN_POINT ( 'NONE',  ( 22.20168578472828358, 1.497490109320031682, 11.49999999999999645 ) ) ;
#96150 = CARTESIAN_POINT ( 'NONE',  ( -50.49683564601712504, -25.24728724001002433, 5.199897385844055364 ) ) ;
#96151 = FACE_OUTER_BOUND ( 'NONE', #75513, .T. ) ;
#96152 = FACE_BOUND ( 'NONE', #2108, .T. ) ;
#96153 = ORIENTED_EDGE ( 'NONE', *, *, #25796, .F. ) ;
#96155 = VERTEX_POINT ( 'NONE', #75228 ) ;
#96154 = CARTESIAN_POINT ( 'NONE',  ( -35.62287095715005592, -23.47596703998600276, 11.44779298504227505 ) ) ;
#96156 = ORIENTED_EDGE ( 'NONE', *, *, #6382, .T. ) ;
#96157 = CARTESIAN_POINT ( 'NONE',  ( 13.91401389203221406, 6.376774720514426953, 158.0376437107427137 ) ) ;
#96158 = ADVANCED_FACE ( 'NONE', ( #83339 ), #82346, .F. ) ;
#96159 = CARTESIAN_POINT ( 'NONE',  ( -87.52287095715006160, -23.72773821059536914, 11.05748984161097503 ) ) ;
#96160 = CARTESIAN_POINT ( 'NONE',  ( -46.52287095715006160, -29.50250243563736774, 8.947779886222146928 ) ) ;
#96161 = VERTEX_POINT ( 'NONE', #81853 ) ;
#96162 = CARTESIAN_POINT ( 'NONE',  ( -130.5728709571500872, -24.71514176503767146, 0.9371183705310238699 ) ) ;
#96163 = CARTESIAN_POINT ( 'NONE',  ( 6.649717926671450563, 21.43536518531312396, -1.500000000000002220 ) ) ;
#96164 = ORIENTED_EDGE ( 'NONE', *, *, #61593, .F. ) ;
#96165 = CARTESIAN_POINT ( 'NONE',  ( -112.5175246721842655, -24.15620529776628445, 10.23563542870659404 ) ) ;
#96167 = FACE_OUTER_BOUND ( 'NONE', #55895, .T. ) ;
#96166 = VECTOR ( 'NONE', #16632, 1000.000000000000000 ) ;
#96168 = CARTESIAN_POINT ( 'NONE',  ( 10.22011794244940752, 3.316774720515020203, -27.02313658111319938 ) ) ;
#96169 = EDGE_CURVE ( 'NONE', #71152, #69536, #35187, .T. ) ;
#96170 = EDGE_CURVE ( 'NONE', #39801, #20337, #37174, .T. ) ;
#96171 = LINE ( 'NONE', #10422, #91893 ) ;
#96172 = EDGE_CURVE ( 'NONE', #84636, #82268, #6216, .T. ) ;
#96173 = CARTESIAN_POINT ( 'NONE',  ( -130.5728709571501156, -25.30557784678704891, 3.856996771331004048 ) ) ;
#96174 = CARTESIAN_POINT ( 'NONE',  ( 3.881049643139886207, -19.21785841795820104, -1.500000000000002220 ) ) ;
#96175 = CIRCLE ( 'NONE', #60541, 2.349999999999999645 ) ;
#96176 = CARTESIAN_POINT ( 'NONE',  ( -29.49875734969026198, -0.3587747205144265483, 10.11402280011862587 ) ) ;
#96178 = ADVANCED_FACE ( 'NONE', ( #27073 ), #27577, .T. ) ;
#96177 = VERTEX_POINT ( 'NONE', #96572 ) ;
#96179 = CARTESIAN_POINT ( 'NONE',  ( 8.792760106793807040, 19.66521392739144858, -1.500000000000002220 ) ) ;
#96180 = LINE ( 'NONE', #57625, #13930 ) ;
#96181 = CARTESIAN_POINT ( 'NONE',  ( -70.94546041667526026, -25.25639558167272725, 6.902322488783775079 ) ) ;
#96182 = LINE ( 'NONE', #95676, #27966 ) ;
#96183 = DIRECTION ( 'NONE',  ( -0.1875268396392987258, -0.000000000000000000, -0.9822594791677485837 ) ) ;
#96184 = CARTESIAN_POINT ( 'NONE',  ( 2.319610639010541764, -22.79860127089448696, -1.500000000000002220 ) ) ;
#96185 = APPROVAL_ROLE ( '' ) ;
#96186 = CARTESIAN_POINT ( 'NONE',  ( -66.52287095715007581, -23.47593901973090524, -1.443836447538997092 ) ) ;
#96187 = CARTESIAN_POINT ( 'NONE',  ( -53.49620482326537285, -24.34968618360933590, 0.1864209137778785885 ) ) ;
#96188 = CARTESIAN_POINT ( 'NONE',  ( -20.04763853020464737, 0.9818187932333496404, 11.49999999999999645 ) ) ;
#96189 = CARTESIAN_POINT ( 'NONE',  ( -40.58953762381671737, -25.00182538069145011, 7.747789668545099317 ) ) ;
#96190 = DIRECTION ( 'NONE',  ( 0.000000000000000000, 0.000000000000000000, -1.000000000000000000 ) ) ;
#96191 = CARTESIAN_POINT ( 'NONE',  ( -0.7395115731254252589, 18.09566585216508727, -8.999999999999998224 ) ) ;
#96192 = CARTESIAN_POINT ( 'NONE',  ( -102.5895376238167103, -24.64898659630368272, 1.056161002820388273 ) ) ;
#96193 = FACE_OUTER_BOUND ( 'NONE', #87647, .T. ) ;
#96194 = ADVANCED_FACE ( 'NONE', ( #19446 ), #19943, .F. ) ;
#96196 = ADVANCED_FACE ( 'NONE', ( #50912 ), #44490, .T. ) ;
#96195 = CARTESIAN_POINT ( 'NONE',  ( 11.68167410197319001, -16.05257874518773065, -1.500000000000002220 ) ) ;
#96197 = CARTESIAN_POINT ( 'NONE',  ( -90.62287095715004170, -24.92604778743018201, 8.074972756849357225 ) ) ;
#96198 = CARTESIAN_POINT ( 'NONE',  ( -5.312243195520525596, -18.98051080891723430, -1.500000000000002220 ) ) ;
#96199 = CARTESIAN_POINT ( 'NONE',  ( -42.52203047475234854, -23.48783264082477373, -1.443836473390076147 ) ) ;
#96200 = B_SPLINE_CURVE_WITH_KNOTS ( 'NONE', 3,
 ( #5876, #75378, #82008, #59683, #90615, #28218 ),
 .UNSPECIFIED., .F., .F.,
 ( 4, 2, 4 ),
 ( 6.384118678617699402E-06, 0.001386860460828380406, 0.002767336802978143193 ),
 .UNSPECIFIED. ) ;
#96201 = VECTOR ( 'NONE', #67877, 1000.000000000000000 ) ;
#96202 = DATE_TIME_ROLE ( 'classification_date' ) ;
#96203 = CARTESIAN_POINT ( 'NONE',  ( -115.6228709571500701, -24.91544648472627088, 1.928969306349434643 ) ) ;
#96204 = CARTESIAN_POINT ( 'NONE',  ( 2.993365552154886089, -6.376774720514413630, 19.24059921568563425 ) ) ;
#96205 = CARTESIAN_POINT ( 'NONE',  ( -3.146292006899429783, -20.37002610441940220, 11.49999999999999645 ) ) ;
#96206 = EDGE_CURVE ( 'NONE', #95483, #79654, #54904, .T. ) ;
#96207 = CARTESIAN_POINT ( 'NONE',  ( -29.62287095715005592, -23.40871900810292772, -1.443836166241315055 ) ) ;
#96208 = TOROIDAL_SURFACE ( 'NONE', #73533, 1.049999999999998934, 0.5999999999999999778 ) ;
#96209 = CARTESIAN_POINT ( 'NONE',  ( 20.84710439121840864, 8.857176948214046774, 11.49999999999999645 ) ) ;
#96210 = EDGE_LOOP ( 'NONE', ( #6836, #26259, #4621, #92859 ) ) ;
#96211 = CARTESIAN_POINT ( 'NONE',  ( -69.63000454671555417, -25.25639544928042568, 6.841411100453155036 ) ) ;
#96212 = CARTESIAN_POINT ( 'NONE',  ( -97.52218086169804678, -23.48783264082477729, -1.443836473390088138 ) ) ;
#96213 = AXIS2_PLACEMENT_3D ( 'NONE', #99006, #90415, #68579 ) ;
#96214 = FACE_OUTER_BOUND ( 'NONE', #35615, .T. ) ;
#96215 = ADVANCED_FACE ( 'NONE', ( #91951 ), #23419, .F. ) ;
#96216 = CARTESIAN_POINT ( 'NONE',  ( -76.62287095715007013, -29.50248528299804818, 1.056150453629038477 ) ) ;
#96217 = EDGE_CURVE ( 'NONE', #58474, #99423, #88249, .T. ) ;
#96218 = EDGE_LOOP ( 'NONE', ( #59425, #17239, #88634, #22251 ) ) ;
#96219 = CARTESIAN_POINT ( 'NONE',  ( -30.54627711375826493, -23.48004750822538611, -1.443836485791523128 ) ) ;
#96220 = CARTESIAN_POINT ( 'NONE',  ( 20.53691900564983186, 10.01969956684014207, -1.500000000000002220 ) ) ;
#96222 = ADVANCED_FACE ( 'NONE', ( #53408 ), #31047, .T. ) ;
#96221 = DIRECTION ( 'NONE',  ( -0.000000000000000000, 2.173523156925979552E-06, -0.9999999999976378895 ) ) ;
#96223 = CARTESIAN_POINT ( 'NONE',  ( -113.6268376558039108, -24.15620529776628800, 10.23563542870659582 ) ) ;
#96224 = CARTESIAN_POINT ( 'NONE',  ( -82.55857454939099682, -23.73791477778912196, 11.05961554403170943 ) ) ;
#96225 = CARTESIAN_POINT ( 'NONE',  ( 8.471766090126642723, -20.80389698432254519, 11.49999999999999645 ) ) ;
#96226 = ORIENTED_EDGE ( 'NONE', *, *, #93926, .T. ) ;
#96227 = CARTESIAN_POINT ( 'NONE',  ( -5.891025641025639636, -6.376774720514420736, 20.75510817307693046 ) ) ;
#96228 = CARTESIAN_POINT ( 'NONE',  ( 15.04091035147580335, -15.99806323810862274, 11.49999999999998934 ) ) ;
#96229 = PLANE ( 'NONE',  #59215 ) ;
#96230 = CARTESIAN_POINT ( 'NONE',  ( -111.6321586287164109, -23.48783264082477729, -1.443836473390087249 ) ) ;
#96231 = CARTESIAN_POINT ( 'NONE',  ( -29.24636659181000198, -25.21724415148663567, 4.940287013585090925 ) ) ;
#96232 = ORIENTED_EDGE ( 'NONE', *, *, #57595, .F. ) ;
#96233 = CARTESIAN_POINT ( 'NONE',  ( -29.49875734969026198, -5.965225279485572685, 0.1180228001186258285 ) ) ;
#96234 = CARTESIAN_POINT ( 'NONE',  ( -78.94303308397306296, -25.26642230834568537, 5.977536689587218177 ) ) ;
#96235 = VERTEX_POINT ( 'NONE', #47292 ) ;
#96236 = DIRECTION ( 'NONE',  ( 0.000000000000000000, -0.9999999999976377785, -2.173523156925978705E-06 ) ) ;
#96237 = CARTESIAN_POINT ( 'NONE',  ( 17.04084431845542369, 11.38269047019995206, -1.500000000000002220 ) ) ;
#96238 = ORIENTED_EDGE ( 'NONE', *, *, #69600, .F. ) ;
#96239 = ORIENTED_EDGE ( 'NONE', *, *, #45417, .F. ) ;
#96240 = ORIENTED_EDGE ( 'NONE', *, *, #79580, .T. ) ;
#96241 = CARTESIAN_POINT ( 'NONE',  ( -81.22842933447068958, -25.18098627503610132, 6.807814688516057977 ) ) ;
#96242 = CARTESIAN_POINT ( 'NONE',  ( 10.19088217375349892, 20.72639945755932800, -1.500000000000002220 ) ) ;
#96243 = CARTESIAN_POINT ( 'NONE',  ( -104.6305895431347466, -23.96169478059713853, 10.65365249895717525 ) ) ;
#96244 = CARTESIAN_POINT ( 'NONE',  ( -16.54958403137900191, 11.88860064210666856, -1.500000000000002220 ) ) ;
#96245 = VERTEX_POINT ( 'NONE', #14817 ) ;
#96246 = CARTESIAN_POINT ( 'NONE',  ( -126.5228709571500616, -29.50250786944525672, 11.44777988621622633 ) ) ;
#96247 = CARTESIAN_POINT ( 'NONE',  ( -51.54509106397593143, -25.21614873127006007, 3.448408489132474664 ) ) ;
#96248 = CARTESIAN_POINT ( 'NONE',  ( -105.5120883362020123, -24.52300882791530512, 0.6510814631126371488 ) ) ;
#96249 = CARTESIAN_POINT ( 'NONE',  ( -71.03336120160147971, -25.25855344096944677, 7.389033197858497104 ) ) ;
#96250 = EDGE_LOOP ( 'NONE', ( #51955, #37637, #96000, #16021 ) ) ;
#96251 = CARTESIAN_POINT ( 'NONE',  ( -29.22054808153496808, -25.21532083643219480, 4.231943384887517645 ) ) ;
#96253 = CIRCLE ( 'NONE', #91314, 1.529999999999998916 ) ;
#96252 = CARTESIAN_POINT ( 'NONE',  ( -49.50841769935764347, -29.50249164770001542, 3.984438540080014413 ) ) ;
#96254 = ORIENTED_EDGE ( 'NONE', *, *, #57243, .T. ) ;
#96255 = CARTESIAN_POINT ( 'NONE',  ( -16.75865769207039335, -12.26659692683164593, -1.500000000000002220 ) ) ;
#96256 = ORIENTED_EDGE ( 'NONE', *, *, #23294, .T. ) ;
#96258 = VERTEX_POINT ( 'NONE', #53905 ) ;
#96257 = CARTESIAN_POINT ( 'NONE',  ( -39.44687923781921057, -25.27828342519987359, 4.188173683033348027 ) ) ;
#96259 = CARTESIAN_POINT ( 'NONE',  ( -86.62287095715004170, -23.48783264082478794, -1.443836473390063713 ) ) ;
#96260 = CARTESIAN_POINT ( 'NONE',  ( -51.49524425620752766, -25.30370764251490812, 5.230807508121633198 ) ) ;
#96261 = VERTEX_POINT ( 'NONE', #99545 ) ;
#96262 = EDGE_LOOP ( 'NONE', ( #61350, #46777, #91408, #41268 ) ) ;
#96263 = CARTESIAN_POINT ( 'NONE',  ( -78.62287095715007013, -23.48783264082478439, -1.443836473390065711 ) ) ;
#96264 = CARTESIAN_POINT ( 'NONE',  ( -57.62287095715004881, -24.64898659630367916, 1.056161002820822592 ) ) ;
#96265 = CARTESIAN_POINT ( 'NONE',  ( -71.26908920811321480, -25.31201727820361214, 5.945032220875477336 ) ) ;
#96267 = ORIENTED_EDGE ( 'NONE', *, *, #31022, .F. ) ;
#96266 = CARTESIAN_POINT ( 'NONE',  ( -3.902479932019291553, -21.71820464621639246, 11.49999999999999645 ) ) ;
#96268 = CARTESIAN_POINT ( 'NONE',  ( -47.62287095715004881, -24.66019654487199020, 8.947790411086133489 ) ) ;
#96269 = CARTESIAN_POINT ( 'NONE',  ( 20.74359285767136640, 8.971229656761206428, -1.500000000000002220 ) ) ;
#96270 = SHAPE_REPRESENTATION ( 'MAS-154', ( #52021, #84451, #11529, #76329, #5080, #26155, #9928, #24482, #50425, #65020, #95834, #32599, #89327, #66673 ), #52097 ) ;
#96272 = ORIENTED_EDGE ( 'NONE', *, *, #57243, .F. ) ;
#96271 = FACE_OUTER_BOUND ( 'NONE', #8853, .T. ) ;
#96273 = ORIENTED_EDGE ( 'NONE', *, *, #33751, .F. ) ;
#96274 = B_SPLINE_CURVE_WITH_KNOTS ( 'NONE', 3,
 ( #81364, #11846, #12341, #43310, #74249, #35693 ),
 .UNSPECIFIED., .F., .F.,
 ( 4, 2, 4 ),
 ( 0.000000000000000000, 0.001380901958385383774, 0.002761803916770767548 ),
 .UNSPECIFIED. ) ;
#96275 = DIRECTION ( 'NONE',  ( -1.000000000000000000, -0.000000000000000000, -0.000000000000000000 ) ) ;
#96276 = CARTESIAN_POINT ( 'NONE',  ( -86.58953762381671027, -23.48783264082478794, -1.443836473390063713 ) ) ;
#96277 = EDGE_LOOP ( 'NONE', ( #16735, #1830, #55556, #1429 ) ) ;
#96278 = CARTESIAN_POINT ( 'NONE',  ( -19.38594737788604405, 8.525550480899875438, -1.500000000000002220 ) ) ;
#96279 = ADVANCED_FACE ( 'NONE', ( #60530 ), #38157, .T. ) ;
#96280 = CARTESIAN_POINT ( 'NONE',  ( -125.6228709571500559, -24.82558206586145033, 1.605769216559438828 ) ) ;
#96281 = PLANE ( 'NONE',  #19487 ) ;
#96282 = CARTESIAN_POINT ( 'NONE',  ( -10.71655374829924767, -19.46388382022006525, -1.500000000000002220 ) ) ;
#96283 = EDGE_CURVE ( 'NONE', #72936, #94029, #7714, .T. ) ;
#96284 = CARTESIAN_POINT ( 'NONE',  ( -114.5892361776109141, -24.34968618360934656, 0.1864209137778972403 ) ) ;
#96285 = EDGE_CURVE ( 'NONE', #25496, #59175, #1083, .T. ) ;
#96286 = VERTEX_POINT ( 'NONE', #61525 ) ;
#96287 = CARTESIAN_POINT ( 'NONE',  ( -112.5228709571501184, -23.96127896942159907, -0.6493128930933955711 ) ) ;
#96288 = CARTESIAN_POINT ( 'NONE',  ( 20.60020833695035236, 0.000000000000000000, 1.249999999999998446 ) ) ;
#96289 = EDGE_CURVE ( 'NONE', #66424, #24715, #108, .T. ) ;
#96290 = ADVANCED_FACE ( 'NONE', ( #37667 ), #45294, .F. ) ;
#96291 = CARTESIAN_POINT ( 'NONE',  ( -41.31495979539203489, -25.15619487155882084, 3.098286890894269785 ) ) ;
#96292 = LINE ( 'NONE', #34392, #77684 ) ;
#96293 = CARTESIAN_POINT ( 'NONE',  ( -15.27948257512286645, 12.15582775940324822, 11.49999999999998934 ) ) ;
#96294 = CARTESIAN_POINT ( 'NONE',  ( -18.57871158907727249, 10.67946855401146777, 11.49999999999998934 ) ) ;
#96295 = CARTESIAN_POINT ( 'NONE',  ( -0.5218785734906133955, -6.376774720514410077, 19.14848118821636547 ) ) ;
#96296 = CARTESIAN_POINT ( 'NONE',  ( -77.62287095715007013, -23.48786465467241413, 11.44779295918254469 ) ) ;
#96297 = CARTESIAN_POINT ( 'NONE',  ( -77.62662168933164253, -24.51314013834315375, 0.6176544820404131775 ) ) ;
#96299 = VECTOR ( 'NONE', #83705, 1000.000000000000114 ) ;
#96298 = CARTESIAN_POINT ( 'NONE',  ( -16.34568771794417685, -15.85656593008108750, -1.500000000000002220 ) ) ;
#96300 = CARTESIAN_POINT ( 'NONE',  ( -102.6269100961048082, -24.34968618360934656, 0.1864209137778959358 ) ) ;
#96301 = LINE ( 'NONE', #49641, #89756 ) ;
#96302 = CARTESIAN_POINT ( 'NONE',  ( -13.91458393394894166, 14.26456941660895339, 11.49999999999999645 ) ) ;
#96303 = DIRECTION ( 'NONE',  ( 0.000000000000000000, 0.000000000000000000, -1.000000000000000000 ) ) ;
#96304 = CARTESIAN_POINT ( 'NONE',  ( -39.57597530520470741, -24.66019654487198665, 8.947790411086131712 ) ) ;
#96305 = CARTESIAN_POINT ( 'NONE',  ( -57.52287095715005449, -23.47596703998600631, 11.44779298504228926 ) ) ;
#96306 = ORIENTED_EDGE ( 'NONE', *, *, #97881, .T. ) ;
#96307 = CARTESIAN_POINT ( 'NONE',  ( -74.52287095715007581, -29.50250243563736774, 8.947779886222143375 ) ) ;
#96308 = EDGE_CURVE ( 'NONE', #88549, #96700, #89498, .T. ) ;
#96309 = CARTESIAN_POINT ( 'NONE',  ( -31.21623173926616701, -25.31516574674648368, 3.894478520810415567 ) ) ;
#96310 = AXIS2_PLACEMENT_3D ( 'NONE', #45188, #7111, #69013 ) ;
#96311 = CARTESIAN_POINT ( 'NONE',  ( 8.489507321284875729, -19.98171680480944445, 11.49999999999998934 ) ) ;
#96312 = CARTESIAN_POINT ( 'NONE',  ( -93.52287095715006160, -24.65952944569304606, 1.056160979905700570 ) ) ;
#96313 = CARTESIAN_POINT ( 'NONE',  ( 15.26536572251939461, -12.21375333317339695, -1.500000000000002220 ) ) ;
#96314 = CARTESIAN_POINT ( 'NONE',  ( -27.68651082257923690, -24.80976250947271211, 7.605672514646787619 ) ) ;
#96315 = EDGE_CURVE ( 'NONE', #14223, #82393, #62927, .T. ) ;
#96316 = ORIENTED_EDGE ( 'NONE', *, *, #9948, .T. ) ;
#96317 = CALENDAR_DATE ( 2026, 9, 10 ) ;
#96318 = CARTESIAN_POINT ( 'NONE',  ( -4.993225604111834137, 0.3587747205143964613, -29.11654937215279304 ) ) ;
#96319 = CARTESIAN_POINT ( 'NONE',  ( 14.97853827808193294, 13.91023239937271860, 11.49999999999999645 ) ) ;
#96320 = PLANE ( 'NONE',  #97495 ) ;
#96321 = DIRECTION ( 'NONE',  ( 0.000000000000000000, 3.740886741919572836E-15, -1.000000000000000000 ) ) ;
#96322 = EDGE_LOOP ( 'NONE', ( #71320, #52857, #37474, #79021 ) ) ;
#96323 = CARTESIAN_POINT ( 'NONE',  ( -46.62287095715004881, -23.47593901973091235, -1.443836447539009749 ) ) ;
#96324 = CARTESIAN_POINT ( 'NONE',  ( -39.44943695351214785, -25.18431046068020152, 4.097885212006306510 ) ) ;
#96325 = DIRECTION ( 'NONE',  ( 3.773278334444167608E-23, -1.000000000000000000, 0.000000000000000000 ) ) ;
#96326 = CARTESIAN_POINT ( 'NONE',  ( -88.62287095715004170, -29.50250786944525672, 11.44777988621623344 ) ) ;
#96327 = ORIENTED_EDGE ( 'NONE', *, *, #77944, .T. ) ;
#96328 = CARTESIAN_POINT ( 'NONE',  ( 13.91401389203221406, -3.316774720514426456, 158.0376437107427137 ) ) ;
#96329 = EDGE_CURVE ( 'NONE', #39981, #61060, #20933, .T. ) ;
#96330 = CARTESIAN_POINT ( 'NONE',  ( -20.38739128398232836, 10.50225141308550292, 11.49999999999999645 ) ) ;
#96331 = CARTESIAN_POINT ( 'NONE',  ( 12.23086119556625206, 19.17791753167082192, 11.49999999999998934 ) ) ;
#96332 = CARTESIAN_POINT ( 'NONE',  ( 3.825380556292953482, -6.376774720514427841, 21.83927723428477208 ) ) ;
#96333 = DIRECTION ( 'NONE',  ( -3.773278334453079030E-23, 0.9999999999976377785, 2.173523156925979128E-06 ) ) ;
#96334 = CARTESIAN_POINT ( 'NONE',  ( -90.62775138037345357, -24.73486907724917572, 1.287355809206966573 ) ) ;
#96335 = VECTOR ( 'NONE', #27791, 1000.000000000000000 ) ;
#96336 = DIRECTION ( 'NONE',  ( -0.000000000000000000, 0.000000000000000000, 1.000000000000000000 ) ) ;
#96337 = PLANE ( 'NONE',  #90273 ) ;
#96338 = EDGE_CURVE ( 'NONE', #76346, #37940, #36310, .T. ) ;
#96339 = CARTESIAN_POINT ( 'NONE',  ( -6.606886629844116676, -20.84447163495035937, 11.49999999999998934 ) ) ;
#96340 = B_SPLINE_CURVE_WITH_KNOTS ( 'NONE', 3,
 ( #71058, #13877, #1548, #61576, #15371, #53960 ),
 .UNSPECIFIED., .F., .F.,
 ( 4, 2, 4 ),
 ( 0.001731663773559744077, 0.004550964303235547140, 0.007370264832911350636 ),
 .UNSPECIFIED. ) ;
#96341 = CARTESIAN_POINT ( 'NONE',  ( -69.63557676323225110, -24.15620529776627734, 10.23563542870660825 ) ) ;
#96342 = DIRECTION ( 'NONE',  ( 1.797640907747986603E-16, -1.000000000000000000, 0.000000000000000000 ) ) ;
#96343 = CARTESIAN_POINT ( 'NONE',  ( -50.38822539166535108, -25.31267346029541088, 4.736250531364077254 ) ) ;
#96344 = CARTESIAN_POINT ( 'NONE',  ( -48.22287095715009286, -23.47593901973090524, -1.443836447538998424 ) ) ;
#96345 = ORIENTED_EDGE ( 'NONE', *, *, #90013, .T. ) ;
#96346 = CARTESIAN_POINT ( 'NONE',  ( -10.01004151551622456, -17.79114453763541093, 11.49999999999998934 ) ) ;
#96347 = ORIENTED_EDGE ( 'NONE', *, *, #14850, .T. ) ;
#96348 = ORIENTED_EDGE ( 'NONE', *, *, #76576, .F. ) ;
#96349 = ORIENTED_EDGE ( 'NONE', *, *, #20791, .T. ) ;
#96350 = ORIENTED_EDGE ( 'NONE', *, *, #78709, .T. ) ;
#96351 = B_SPLINE_CURVE_WITH_KNOTS ( 'NONE', 3,
 ( #13067, #60767, #90204, #53656, #29300, #51652, #84582, #99785, #37424, #13566 ),
 .UNSPECIFIED., .F., .F.,
 ( 4, 2, 2, 2, 4 ),
 ( 1.438708811377697253E-14, 0.0008342332072047298078, 0.001251349810799902386, 0.001459908112597480814, 0.001668466414395059242 ),
 .UNSPECIFIED. ) ;
#96352 = CARTESIAN_POINT ( 'NONE',  ( -18.14924840124409045, -14.16824886576183040, -1.500000000000002220 ) ) ;
#96353 = CARTESIAN_POINT ( 'NONE',  ( 9.749999999999985789, 18.74999999999999645, 2.100000000000000089 ) ) ;
#96354 = CARTESIAN_POINT ( 'NONE',  ( -7.946508460909448956, -18.53024980520100939, -1.500000000000002220 ) ) ;
#96355 = VERTEX_POINT ( 'NONE', #3129 ) ;
#96356 = CARTESIAN_POINT ( 'NONE',  ( -92.62287095715005592, -29.50250243563736774, 8.947779886222139822 ) ) ;
#96357 = CARTESIAN_POINT ( 'NONE',  ( -49.92287095715005307, -23.47593901973090169, -1.443836447538997758 ) ) ;
#96358 = CARTESIAN_POINT ( 'NONE',  ( -28.98875734969026041, -0.3587747205144265483, 17.86602280011862476 ) ) ;
#96359 = CARTESIAN_POINT ( 'NONE',  ( -53.65876936014893062, -23.48786465467240347, 11.44779295918255002 ) ) ;
#96361 = ORIENTED_EDGE ( 'NONE', *, *, #81295, .T. ) ;
#96360 = CARTESIAN_POINT ( 'NONE',  ( 20.50650179695670872, -5.950058665555418180, 11.49999999999999645 ) ) ;
#96362 = CARTESIAN_POINT ( 'NONE',  ( 6.627987042499408510, -5.876774720514424288, 21.45334999081212146 ) ) ;
#96363 = ORIENTED_EDGE ( 'NONE', *, *, #62029, .F. ) ;
#96364 = CARTESIAN_POINT ( 'NONE',  ( 18.07686251855496096, -12.98574554580779861, 11.49999999999998934 ) ) ;
#96365 = CARTESIAN_POINT ( 'NONE',  ( 13.32396043830641830, 15.83023408377254704, 11.49999999999998934 ) ) ;
#96366 = VECTOR ( 'NONE', #27452, 1000.000000000000114 ) ;
#96367 = ORIENTED_EDGE ( 'NONE', *, *, #32641, .F. ) ;
#96368 = CARTESIAN_POINT ( 'NONE',  ( -113.5562042904834072, -24.65952944569304961, 1.056160979905704123 ) ) ;
#96369 = EDGE_LOOP ( 'NONE', ( #89357, #29326, #38199, #43916 ) ) ;
#96370 = CARTESIAN_POINT ( 'NONE',  ( -28.49194798280535323, -5.965225279485572685, 28.38521343323375490 ) ) ;
#96371 = ORIENTED_EDGE ( 'NONE', *, *, #37515, .T. ) ;
#96372 = CARTESIAN_POINT ( 'NONE',  ( -50.21186637932700592, -25.27517878598833789, 2.837930930803035601 ) ) ;
#96373 = CARTESIAN_POINT ( 'NONE',  ( -8.674659061502078217, -19.08593140856894621, -1.500000000000002220 ) ) ;
#96374 = CARTESIAN_POINT ( 'NONE',  ( 17.35060923807083810, -13.37414737355047656, 11.49999999999999645 ) ) ;
#96375 = VECTOR ( 'NONE', #94610, 1000.000000000000000 ) ;
#96376 = PLANE ( 'NONE',  #47989 ) ;
#96377 = CARTESIAN_POINT ( 'NONE',  ( -6.869692127560369066, -21.44495933931894527, 11.49999999999998934 ) ) ;
#96378 = CARTESIAN_POINT ( 'NONE',  ( 9.933205088616889000, -18.45388779576350302, -1.500000000000002220 ) ) ;
#96379 = CARTESIAN_POINT ( 'NONE',  ( -38.52794170851076672, -24.65952944569304606, 1.056160979905694131 ) ) ;
#96380 = CARTESIAN_POINT ( 'NONE',  ( 5.817949855437939632, -6.376774720514417183, 20.34349022145623209 ) ) ;
#96381 = CARTESIAN_POINT ( 'NONE',  ( 13.91401389203221406, -5.965225279485572685, 158.0376437107427137 ) ) ;
#96382 = CARTESIAN_POINT ( 'NONE',  ( -70.58953762381673869, -23.47596703998600276, 11.44779298504227505 ) ) ;
#96383 = ORIENTED_EDGE ( 'NONE', *, *, #4338, .F. ) ;
#96384 = VERTEX_POINT ( 'NONE', #32556 ) ;
#96385 = ORIENTED_EDGE ( 'NONE', *, *, #15180, .F. ) ;
#96386 = CARTESIAN_POINT ( 'NONE',  ( -99.29755759592676156, -25.12215475168745016, 6.181036740048140743 ) ) ;
#96387 = ORIENTED_EDGE ( 'NONE', *, *, #96566, .F. ) ;
#96388 = CARTESIAN_POINT ( 'NONE',  ( 14.19067371521932230, 16.14321034643037578, -1.500000000000002220 ) ) ;
#96389 = EDGE_CURVE ( 'NONE', #86483, #59212, #9726, .T. ) ;
#96390 = ORIENTED_EDGE ( 'NONE', *, *, #94921, .F. ) ;
#96391 = CARTESIAN_POINT ( 'NONE',  ( -26.25116965330634855, -24.90568970725252385, 6.270097125102462421 ) ) ;
#96392 = CARTESIAN_POINT ( 'NONE',  ( 1.225302832070333636, 21.05158420706169764, -1.500000000000002220 ) ) ;
#96393 = DIRECTION ( 'NONE',  ( -0.000000000000000000, -1.000000000000000000, -0.000000000000000000 ) ) ;
#96394 = ADVANCED_FACE ( 'NONE', ( #63530 ), #86838, .T. ) ;
#96395 = CARTESIAN_POINT ( 'NONE',  ( -52.62287095715007013, -23.96127896941632685, -0.6493128931037880358 ) ) ;
#96396 = CARTESIAN_POINT ( 'NONE',  ( -50.56030009453918694, -23.85049219812685095, 10.88485053497527133 ) ) ;
#96397 = DIRECTION ( 'NONE',  ( 3.773278334444166432E-23, -1.000000000000000000, 0.000000000000000000 ) ) ;
#96398 = CARTESIAN_POINT ( 'NONE',  ( -100.6228709571500559, -24.99132157543167310, 2.256160258750667502 ) ) ;
#96399 = CARTESIAN_POINT ( 'NONE',  ( 21.95769793831392036, 2.030053023538682222, -1.500000000000002220 ) ) ;
#96400 = ORIENTED_EDGE ( 'NONE', *, *, #41314, .T. ) ;
#96401 = CARTESIAN_POINT ( 'NONE',  ( -65.54245111285530356, -24.52399227489126687, 9.353111116836529959 ) ) ;
#96402 = ADVANCED_FACE ( 'NONE', ( #49305 ), #92314, .T. ) ;
#96403 = FACE_OUTER_BOUND ( 'NONE', #81737, .T. ) ;
#96404 = DIRECTION ( 'NONE',  ( 8.719066383522879804E-15, 0.000000000000000000, -1.000000000000000000 ) ) ;
#96405 = ADVANCED_FACE ( 'NONE', ( #50795 ), #27437, .T. ) ;
#96406 = CARTESIAN_POINT ( 'NONE',  ( -62.49104091010542561, -24.66019654487199730, 8.947790411086124607 ) ) ;
#96407 = EDGE_CURVE ( 'NONE', #65127, #70560, #3624, .T. ) ;
#96408 = CARTESIAN_POINT ( 'NONE',  ( -26.12147836438646209, -24.69295662840814387, 2.461328207429541060 ) ) ;
#96409 = AXIS2_PLACEMENT_3D ( 'NONE', #17434, #25041, #31156 ) ;
#96410 = CARTESIAN_POINT ( 'NONE',  ( 1.949999999999999956, 0.1925000000000007538, -0.1924999999999994493 ) ) ;
#96411 = CARTESIAN_POINT ( 'NONE',  ( 12.49974722350246736, 17.29906535522423638, 11.49999999999998934 ) ) ;
#96412 = CARTESIAN_POINT ( 'NONE',  ( -104.5228709571500616, -23.96177878511309345, 10.65340807706329507 ) ) ;
#96413 = EDGE_CURVE ( 'NONE', #22769, #17742, #11713, .T. ) ;
#96414 = CARTESIAN_POINT ( 'NONE',  ( -49.88485461511636032, -25.32724633150700200, 4.398074151685130495 ) ) ;
#96415 = CARTESIAN_POINT ( 'NONE',  ( -70.58953762381673869, -24.99156044556120548, 7.747789690856344613 ) ) ;
#96416 = CARTESIAN_POINT ( 'NONE',  ( -81.46835002855611663, -25.23073161514107454, 6.350709097867520470 ) ) ;
#96417 = CARTESIAN_POINT ( 'NONE',  ( 22.57354875331468591, -1.174960877787051716, -1.500000000000002220 ) ) ;
#96419 = CARTESIAN_POINT ( 'NONE',  ( -92.62287095715005592, -29.50250786944525672, 11.44777988621623344 ) ) ;
#96418 = B_SPLINE_CURVE_WITH_KNOTS ( 'NONE', 3,
 ( #56374, #86294, #87294, #56872 ),
 .UNSPECIFIED., .F., .F.,
 ( 4, 4 ),
 ( 0.000000000000000000, 0.001749918372064178775 ),
 .UNSPECIFIED. ) ;
#96420 = ORIENTED_EDGE ( 'NONE', *, *, #35464, .T. ) ;
#96421 = CARTESIAN_POINT ( 'NONE',  ( -35.62287095715004170, -24.52323809116982645, 9.355190652339427260 ) ) ;
#96422 = CARTESIAN_POINT ( 'NONE',  ( -42.52287095715005449, -29.50248528299804818, 1.056150453629031594 ) ) ;
#96423 = CARTESIAN_POINT ( 'NONE',  ( -15.39140670439391378, -12.39996395878027791, 11.49999999999999645 ) ) ;
#96424 = DIRECTION ( 'NONE',  ( 0.000000000000000000, 0.000000000000000000, 1.000000000000000000 ) ) ;
#96425 = CARTESIAN_POINT ( 'NONE',  ( -67.49693300450357469, -24.51314013834315375, 0.6176544820404126224 ) ) ;
#96426 = ORIENTED_EDGE ( 'NONE', *, *, #71839, .F. ) ;
#96427 = CARTESIAN_POINT ( 'NONE',  ( 10.86264265030973952, -5.965225279485574461, -28.05717073599341305 ) ) ;
#96428 = DIRECTION ( 'NONE',  ( 3.773278334444167608E-23, -1.000000000000000000, 0.000000000000000000 ) ) ;
#96429 = CARTESIAN_POINT ( 'NONE',  ( -113.6228709571500559, -24.64898659630368627, 1.056161002820831474 ) ) ;
#96430 = CARTESIAN_POINT ( 'NONE',  ( -11.89702471719568244, -18.04982639819725776, -1.500000000000002220 ) ) ;
#96431 = CARTESIAN_POINT ( 'NONE',  ( -86.62287095715004170, -23.48783264082478794, -1.443836473390063713 ) ) ;
#96432 = CARTESIAN_POINT ( 'NONE',  ( -7.246369895950522277, -17.95243785538732340, -1.500000000000002220 ) ) ;
#96433 = CARTESIAN_POINT ( 'NONE',  ( -50.55620429048338593, -23.47593901973091235, -1.443836447539009749 ) ) ;
#96434 = LINE ( 'NONE', #58387, #60432 ) ;
#96435 = CARTESIAN_POINT ( 'NONE',  ( 6.953341435731974940, 18.52374150113109152, 11.49999999999998934 ) ) ;
#96436 = ORIENTED_EDGE ( 'NONE', *, *, #47042, .F. ) ;
#96437 = CARTESIAN_POINT ( 'NONE',  ( -18.13051092187696156, -9.059970205480309957, 11.49999999999999645 ) ) ;
#96438 = CARTESIAN_POINT ( 'NONE',  ( 12.30588647389939538, 3.316774720514762187, -28.11066263608955751 ) ) ;
#96439 = VECTOR ( 'NONE', #68507, 1000.000000000000000 ) ;
#96440 = ORIENTED_EDGE ( 'NONE', *, *, #70156, .F. ) ;
#96441 = CARTESIAN_POINT ( 'NONE',  ( -99.83442573030144729, -25.29641444269049444, 4.527172786151116846 ) ) ;
#96442 = DIRECTION ( 'NONE',  ( -0.000000000000000000, 1.000000000000000000, -0.000000000000000000 ) ) ;
#96443 = CARTESIAN_POINT ( 'NONE',  ( -5.576923076923074873, -6.376774720514427841, 21.75000000000000711 ) ) ;
#96444 = CARTESIAN_POINT ( 'NONE',  ( 22.02124265030973760, -6.143225279485574397, 19.55402280011862004 ) ) ;
#96445 = DIRECTION ( 'NONE',  ( -1.000000000000000000, -3.773278334444166432E-23, -8.201307841325785021E-29 ) ) ;
#96446 = CARTESIAN_POINT ( 'NONE',  ( 19.65109224456760728, -3.968444974485820786, 11.49999999999998934 ) ) ;
#96447 = AXIS2_PLACEMENT_3D ( 'NONE', #75279, #76270, #5772 ) ;
#96448 = PLANE ( 'NONE',  #32104 ) ;
#96449 = EDGE_LOOP ( 'NONE', ( #91740, #93375, #90391, #81123 ) ) ;
#96450 = AXIS2_PLACEMENT_3D ( 'NONE', #19592, #50553, #42954 ) ;
#96451 = CARTESIAN_POINT ( 'NONE',  ( 2.899999999999999467, 31.80000000000000071, 2.100000000000000089 ) ) ;
#96452 = CARTESIAN_POINT ( 'NONE',  ( -35.52842849026595218, -24.73486907724917572, 1.287355809206972346 ) ) ;
#96453 = FACE_OUTER_BOUND ( 'NONE', #31295, .T. ) ;
#96454 = FACE_OUTER_BOUND ( 'NONE', #10488, .T. ) ;
#96456 = EDGE_CURVE ( 'NONE', #58907, #27652, #12208, .T. ) ;
#96455 = CARTESIAN_POINT ( 'NONE',  ( -55.62287095715004170, -25.00182538069145011, 7.747789668545097541 ) ) ;
#96457 = DIRECTION ( 'NONE',  ( 0.000000000000000000, 0.000000000000000000, 1.000000000000000000 ) ) ;
#96458 = EDGE_CURVE ( 'NONE', #18521, #62579, #24062, .T. ) ;
#96459 = CARTESIAN_POINT ( 'NONE',  ( -49.26249145549192576, -25.30419751004783535, 5.186272124421678953 ) ) ;
#96460 = ORIENTED_EDGE ( 'NONE', *, *, #10083, .T. ) ;
#96461 = CARTESIAN_POINT ( 'NONE',  ( 8.409737122318338365, 18.51778827956368190, 11.49999999999998934 ) ) ;
#96462 = VERTEX_POINT ( 'NONE', #57918 ) ;
#96463 = CARTESIAN_POINT ( 'NONE',  ( 5.768980952343642166, -22.17701263744951490, 11.49999999999998934 ) ) ;
#96464 = CARTESIAN_POINT ( 'NONE',  ( 29.65417061107837071, 5.752153662292248448, 28.02209566695815823 ) ) ;
#96465 = ORIENTED_EDGE ( 'NONE', *, *, #81524, .T. ) ;
#96466 = CARTESIAN_POINT ( 'NONE',  ( -37.62287095715004881, -24.50216790748098461, 0.6166512839513558220 ) ) ;
#96467 = CARTESIAN_POINT ( 'NONE',  ( -50.04767967325393840, -25.12215411302513957, 7.063298327921868847 ) ) ;
#96468 = CARTESIAN_POINT ( 'NONE',  ( -108.9545715455115129, -25.27705962214097113, 4.170144839539424275 ) ) ;
#96469 = CARTESIAN_POINT ( 'NONE',  ( 21.17954554857512761, 0.9134790845329443520, 11.49999999999999645 ) ) ;
#96470 = VECTOR ( 'NONE', #31427, 1000.000000000000114 ) ;
#96471 = CARTESIAN_POINT ( 'NONE',  ( -19.05511597014879044, -11.33806725510066826, -1.500000000000002220 ) ) ;
#96473 = CARTESIAN_POINT ( 'NONE',  ( 6.226698476505521995, -19.64469265145860177, 11.49999999999998934 ) ) ;
#96472 = CC_DESIGN_PERSON_AND_ORGANIZATION_ASSIGNMENT ( #37417, #51645, ( #83064 ) ) ;
#96474 = VERTEX_POINT ( 'NONE', #82226 ) ;
#96475 = CARTESIAN_POINT ( 'NONE',  ( -50.52287095715006160, -29.50250243563736774, 8.947779886222146928 ) ) ;
#96476 = VERTEX_POINT ( 'NONE', #67518 ) ;
#96477 = CARTESIAN_POINT ( 'NONE',  ( -54.53281950657227384, -24.65952944569304606, 1.056160979905696573 ) ) ;
#96478 = DIRECTION ( 'NONE',  ( -3.773278334453080206E-23, 0.9999999999976377785, 2.173523156925979975E-06 ) ) ;
#96479 = ORIENTED_EDGE ( 'NONE', *, *, #14418, .F. ) ;
#96480 = ORIENTED_EDGE ( 'NONE', *, *, #36637, .T. ) ;
#96481 =( BOUNDED_SURFACE ( )  B_SPLINE_SURFACE ( 3, 2, ( 
 ( #23102, #69801, #85513 ),
 ( #54091, #15004, #94125 ),
 ( #78892, #92129, #24113 ),
 ( #32226, #32730, #85012 ),
 ( #15997, #55085, #9391 ),
 ( #281, #23604, #70805 ),
 ( #15496, #55588, #31230 ),
 ( #46461, #54577, #24609 ),
 ( #40351, #62703, #45972 ),
 ( #77391, #86018, #46967 ),
 ( #70304, #63202, #86517 ),
 ( #78394, #39343, #784 ) ),
 .UNSPECIFIED., .F., .F., .T. ) 
 B_SPLINE_SURFACE_WITH_KNOTS ( ( 4, 2, 2, 2, 2, 4 ),
 ( 3, 3 ),
 ( -3.428680950268159222E-15, 0.001642567453077259246, 0.003285134906157947173, 0.004106418632698291028, 0.004927702359238635317, 0.006570269812319323027 ),
 ( 0.000000000000000000, 1.000000000000000000 ),
 .UNSPECIFIED. ) 
 GEOMETRIC_REPRESENTATION_ITEM ( )  RATIONAL_B_SPLINE_SURFACE ( (
 ( 1.000000000000000000, 0.7071067811865476838, 1.000000000000000000),
 ( 1.000000000000000000, 0.7071067811865476838, 1.000000000000000000),
 ( 1.000000000000000000, 0.7071067811865476838, 1.000000000000000000),
 ( 1.000000000000000000, 0.7071067811865476838, 1.000000000000000000),
 ( 1.000000000000000000, 0.7071067811865476838, 1.000000000000000000),
 ( 1.000000000000000000, 0.7071067811865476838, 1.000000000000000000),
 ( 1.000000000000000000, 0.7071067811865476838, 1.000000000000000000),
 ( 1.000000000000000000, 0.7071067811865476838, 1.000000000000000000),
 ( 1.000000000000000000, 0.7071067811865476838, 1.000000000000000000),
 ( 1.000000000000000000, 0.7071067811865476838, 1.000000000000000000),
 ( 1.000000000000000000, 0.7071067811865476838, 1.000000000000000000),
 ( 1.000000000000000000, 0.7071067811865476838, 1.000000000000000000) ) ) 
 REPRESENTATION_ITEM ( '' )  SURFACE ( )  );
#96482 = ORIENTED_EDGE ( 'NONE', *, *, #81083, .T. ) ;
#96483 = DIRECTION ( 'NONE',  ( 0.5473879298848784991, 0.000000000000000000, -0.8368789961615403783 ) ) ;
#96484 = CARTESIAN_POINT ( 'NONE',  ( 33.69795529655567634, 0.6647747205144264315, 20.86760796525322093 ) ) ;
#96485 = CARTESIAN_POINT ( 'NONE',  ( 5.327901167172695907, -6.376774720514418959, 20.73192761314082233 ) ) ;
#96486 = CARTESIAN_POINT ( 'NONE',  ( -19.11632921840048738, -8.121837694355717119, -1.500000000000002220 ) ) ;
#96487 = CARTESIAN_POINT ( 'NONE',  ( 21.69746526873944958, -0.4026533170205861545, 11.49999999999999645 ) ) ;
#96488 = ORIENTED_EDGE ( 'NONE', *, *, #72127, .F. ) ;
#96489 = CARTESIAN_POINT ( 'NONE',  ( 4.878909776184770742E-15, -5.876774720514426953, 22.50000000000000355 ) ) ;
#96490 = CARTESIAN_POINT ( 'NONE',  ( -115.6302137719211203, -23.85016227208580730, -0.8807180028928280890 ) ) ;
#96491 = CARTESIAN_POINT ( 'NONE',  ( 16.55124408090292576, 15.08944307983326638, 11.49999999999998934 ) ) ;
#96492 = DIRECTION ( 'NONE',  ( -0.9890158633619158257, -0.1478094111296165414, -0.000000000000000000 ) ) ;
#96493 = CARTESIAN_POINT ( 'NONE',  ( 6.660000000000001030, 7.578413286920094194, 5.288828319098143105 ) ) ;
#96494 = VERTEX_POINT ( 'NONE', #42692 ) ;
#96495 = CARTESIAN_POINT ( 'NONE',  ( -31.62287095715003105, -23.96177878511307568, 10.65340807706330928 ) ) ;
#96496 = CARTESIAN_POINT ( 'NONE',  ( -77.52287095715006160, -23.47596703998600631, 11.44779298504228571 ) ) ;
#96497 = VERTEX_POINT ( 'NONE', #27948 ) ;
#96498 = ORIENTED_EDGE ( 'NONE', *, *, #6352, .F. ) ;
#96499 = AXIS2_PLACEMENT_3D ( 'NONE', #68729, #37774, #76317 ) ;
#96500 = CARTESIAN_POINT ( 'NONE',  ( -46.54682791464076530, -24.15620529776627379, 10.23563542870660825 ) ) ;
#96501 = ORIENTED_EDGE ( 'NONE', *, *, #57807, .T. ) ;
#96502 = CIRCLE ( 'NONE', #60881, 2.499999999999963141 ) ;
#96503 = CARTESIAN_POINT ( 'NONE',  ( 21.10678091372558640, -2.468637549841573797, -1.500000000000002220 ) ) ;
#96504 = ORIENTED_EDGE ( 'NONE', *, *, #29130, .F. ) ;
#96505 = CARTESIAN_POINT ( 'NONE',  ( -100.9670406769712656, -25.14006151055734861, 7.002054040855493433 ) ) ;
#96506 = CARTESIAN_POINT ( 'NONE',  ( -1.743439162979827595, 21.76861016152796324, 11.49999999999998934 ) ) ;
#96507 = CARTESIAN_POINT ( 'NONE',  ( -128.6228709571500417, -29.50250786944525672, 11.44777988621622633 ) ) ;
#96508 = CARTESIAN_POINT ( 'NONE',  ( -22.35490716430079061, -3.811827842488555440, -1.500000000000002220 ) ) ;
#96509 = PLANE ( 'NONE',  #33997 ) ;
#96510 = AXIS2_PLACEMENT_3D ( 'NONE', #37506, #99397, #53243 ) ;
#96511 = DIRECTION ( 'NONE',  ( 0.000000000000000000, 0.000000000000000000, 1.000000000000000000 ) ) ;
#96512 = CARTESIAN_POINT ( 'NONE',  ( -1.678574117887026373, -21.80011532881206548, -1.500000000000002220 ) ) ;
#96513 = CARTESIAN_POINT ( 'NONE',  ( -23.59123376470063960, 6.143225279485574397, 23.50402280011862288 ) ) ;
#96514 = ORIENTED_EDGE ( 'NONE', *, *, #88072, .F. ) ;
#96515 = CARTESIAN_POINT ( 'NONE',  ( -69.62287095715005592, -23.48783264082478084, -1.443836473390067265 ) ) ;
#96516 = CARTESIAN_POINT ( 'NONE',  ( 31.02038118199824268, 5.152774720514427642, -4.893189986691015569 ) ) ;
#96517 = VECTOR ( 'NONE', #63556, 1000.000000000000000 ) ;
#96518 = ORIENTED_EDGE ( 'NONE', *, *, #91919, .T. ) ;
#96519 = CARTESIAN_POINT ( 'NONE',  ( -30.57703644430498713, -25.30359631330190950, 3.841990343063858671 ) ) ;
#96520 = ORIENTED_EDGE ( 'NONE', *, *, #52291, .F. ) ;
#96521 = EDGE_CURVE ( 'NONE', #62694, #40793, #85773, .T. ) ;
#96522 = CARTESIAN_POINT ( 'NONE',  ( -3.749999999999999112, 25.69999999999999574, 2.100000000000000089 ) ) ;
#96523 = CARTESIAN_POINT ( 'NONE',  ( -10.31630223030989058, -21.90544972156718018, -1.443836447538997314 ) ) ;
#96524 = CARTESIAN_POINT ( 'NONE',  ( -9.505907188867841029, -19.02311915605711690, 11.49999999999998934 ) ) ;
#96525 = PLANE ( 'NONE',  #67698 ) ;
#96526 = EDGE_CURVE ( 'NONE', #48086, #84956, #70089, .T. ) ;
#96527 = CARTESIAN_POINT ( 'NONE',  ( -26.25750150876569933, -24.75186252390866670, 3.573366613333743391 ) ) ;
#96528 = CARTESIAN_POINT ( 'NONE',  ( -114.5228709571500758, -23.96127896942140367, -0.6493128930937851484 ) ) ;
#96529 = CARTESIAN_POINT ( 'NONE',  ( -38.62287095715005592, -24.64965695001467694, 8.947790433994187609 ) ) ;
#96530 = B_SPLINE_CURVE_WITH_KNOTS ( 'NONE', 3,
 ( #12742, #97975, #83758, #44711 ),
 .UNSPECIFIED., .F., .F.,
 ( 4, 4 ),
 ( 1.788112030672749005E-18, 0.0002127494369525745788 ),
 .UNSPECIFIED. ) ;
#96531 = CARTESIAN_POINT ( 'NONE',  ( -44.62287095715004881, -23.47596703998600631, 11.44779298504227505 ) ) ;
#96532 = ORIENTED_EDGE ( 'NONE', *, *, #97905, .F. ) ;
#96533 = CARTESIAN_POINT ( 'NONE',  ( 17.37147561666312257, 8.948746033654231269, 11.49999999999999645 ) ) ;
#96534 = CARTESIAN_POINT ( 'NONE',  ( -5.514838905578028694, -6.376774720514410077, 19.81240905262003338 ) ) ;
#96535 = DIRECTION ( 'NONE',  ( -3.773278334453079030E-23, 0.9999999999976377785, 2.173523156925979128E-06 ) ) ;
#96536 = EDGE_CURVE ( 'NONE', #53704, #59029, #98439, .T. ) ;
#96537 = EDGE_LOOP ( 'NONE', ( #99464, #30740, #67792, #17446 ) ) ;
#96538 = CARTESIAN_POINT ( 'NONE',  ( -112.6228709571500559, -29.50248528299804818, 1.056150453629043584 ) ) ;
#96539 = CARTESIAN_POINT ( 'NONE',  ( -99.64934318012689118, -25.31535474791540707, 4.927356294767410105 ) ) ;
#96540 = FACE_OUTER_BOUND ( 'NONE', #11190, .T. ) ;
#96541 = CARTESIAN_POINT ( 'NONE',  ( 13.96165483782453087, -2.682774720514426114, -27.24025806393558824 ) ) ;
#96542 = CARTESIAN_POINT ( 'NONE',  ( -16.08770303010339831, 11.32657509950784736, -1.500000000000002220 ) ) ;
#96543 = VERTEX_POINT ( 'NONE', #13202 ) ;
#96544 = AXIS2_PLACEMENT_3D ( 'NONE', #77209, #23936, #78706 ) ;
#96545 = CARTESIAN_POINT ( 'NONE',  ( 8.071512145086503054, -1.028487854913507915, -6.500000000000000000 ) ) ;
#96546 = DIRECTION ( 'NONE',  ( 1.000000000000000000, 3.773278334444167608E-23, 8.201307833595939069E-29 ) ) ;
#96547 = CALENDAR_DATE ( 2026, 9, 10 ) ;
#96548 = ORIENTED_EDGE ( 'NONE', *, *, #15080, .T. ) ;
#96549 = CARTESIAN_POINT ( 'NONE',  ( -74.52287095715007581, -24.65952944569304606, 1.056160979905697239 ) ) ;
#96550 = FACE_OUTER_BOUND ( 'NONE', #28655, .T. ) ;
#96551 = CARTESIAN_POINT ( 'NONE',  ( -47.48889557811029505, -24.51314013834316086, 0.6176544820404172853 ) ) ;
#96552 = CARTESIAN_POINT ( 'NONE',  ( -76.52287095715004739, -23.96127896941632329, -0.6493128931038015805 ) ) ;
#96553 = CARTESIAN_POINT ( 'NONE',  ( -80.90904671513573021, -25.33009845126374771, 4.495758016894969344 ) ) ;
#96554 = CARTESIAN_POINT ( 'NONE',  ( 9.150000000000000355, -6.376774720514426953, -15.70000000000000284 ) ) ;
#96555 = CARTESIAN_POINT ( 'NONE',  ( -73.52287095715007581, -24.50216790748204687, 0.6166512839542513946 ) ) ;
#96556 = CARTESIAN_POINT ( 'NONE',  ( 18.73470368118781693, 6.836574088118649861, -1.500000000000002220 ) ) ;
#96557 = CARTESIAN_POINT ( 'NONE',  ( -0.01697405093676656110, -22.83025757171792947, 7.289440679219588048 ) ) ;
#96558 = CARTESIAN_POINT ( 'NONE',  ( 11.60740158406642664, -16.16820694497113564, -1.500000000000002220 ) ) ;
#96559 = ORIENTED_EDGE ( 'NONE', *, *, #78773, .T. ) ;
#96560 = CARTESIAN_POINT ( 'NONE',  ( -120.5562042904834072, -23.48783264082479150, -1.443836473390058384 ) ) ;
#96561 = ADVANCED_FACE ( 'NONE', ( #27457 ), #28942, .F. ) ;
#96562 = CARTESIAN_POINT ( 'NONE',  ( -93.55620429048339304, -24.66019654487199375, 8.947790411086128159 ) ) ;
#96563 = CARTESIAN_POINT ( 'NONE',  ( 8.159923944623203695, -3.316774720514428232, -28.14238247154670347 ) ) ;
#96564 = CARTESIAN_POINT ( 'NONE',  ( -12.88759680649768136, 16.30154091734715749, 11.49999999999999645 ) ) ;
#96565 = CARTESIAN_POINT ( 'NONE',  ( -6.775140224358976226, -6.376774720514408301, 19.14743589743590846 ) ) ;
#96566 = EDGE_CURVE ( 'NONE', #78612, #16787, #100376, .T. ) ;
#96567 = LINE ( 'NONE', #58524, #93925 ) ;
#96568 = CARTESIAN_POINT ( 'NONE',  ( 21.14566350062385780, -8.679158401671109857, 11.49999999999999645 ) ) ;
#96569 = VECTOR ( 'NONE', #11588, 1000.000000000000114 ) ;
#96570 = ORIENTED_EDGE ( 'NONE', *, *, #56534, .T. ) ;
#96571 = CARTESIAN_POINT ( 'NONE',  ( -64.62287095715005592, -24.65952944569304250, 1.056160979905695685 ) ) ;
#96573 = CIRCLE ( 'NONE', #46305, 2.500000000000000444 ) ;
#96572 = CARTESIAN_POINT ( 'NONE',  ( -36.52287095715006870, -23.48786465467240347, 11.44779295918255180 ) ) ;
#96574 = ORIENTED_EDGE ( 'NONE', *, *, #38443, .F. ) ;
#96575 = AXIS2_PLACEMENT_3D ( 'NONE', #84173, #36501, #13653 ) ;
#96576 = CARTESIAN_POINT ( 'NONE',  ( 10.87751022112437482, 17.06716278085755079, -1.500000000000002220 ) ) ;
#96577 = FACE_OUTER_BOUND ( 'NONE', #89860, .T. ) ;
#96578 = VECTOR ( 'NONE', #33525, 1000.000000000000114 ) ;
#96579 = PLANE ( 'NONE',  #84168 ) ;
#96580 = VECTOR ( 'NONE', #64793, 1000.000000000000000 ) ;
#96581 = DIRECTION ( 'NONE',  ( -3.773278334453079618E-23, 0.9999999999976377785, 2.173523156925979975E-06 ) ) ;
#96582 = VERTEX_POINT ( 'NONE', #90344 ) ;
#96583 = CARTESIAN_POINT ( 'NONE',  ( -79.71038897795425271, -25.31035002353226915, 4.643805851083846470 ) ) ;
#96584 = CARTESIAN_POINT ( 'NONE',  ( -58.62287095715004881, -29.50248528299804818, 1.056150453629034924 ) ) ;
#96585 = CARTESIAN_POINT ( 'NONE',  ( -20.04763853020464737, 0.9818187932333496404, -1.500000000000002220 ) ) ;
#96586 = CARTESIAN_POINT ( 'NONE',  ( -20.81348254183067681, -2.960215062046979373, 11.49999999999999645 ) ) ;
#96587 = CARTESIAN_POINT ( 'NONE',  ( -54.62287095715004170, -23.96177878511307924, 10.65340807706331105 ) ) ;
#96588 = CARTESIAN_POINT ( 'NONE',  ( 8.160000000000000142, -10.15233964170348457, 0.003711184059992174607 ) ) ;
#96589 = CARTESIAN_POINT ( 'NONE',  ( 18.76863814860013235, 11.56883167669432133, 11.49999999999998934 ) ) ;
#96590 = CC_DESIGN_DATE_AND_TIME_ASSIGNMENT ( #39886, #38384, ( #14113 ) ) ;
#96591 = CARTESIAN_POINT ( 'NONE',  ( -40.02212956655154130, -25.31589315899555359, 5.017934114441384708 ) ) ;
#96592 = CARTESIAN_POINT ( 'NONE',  ( 2.000000000000000000, 0.000000000000000000, 0.000000000000000000 ) ) ;
#96593 = LINE ( 'NONE', #74260, #29809 ) ;
#96594 = CARTESIAN_POINT ( 'NONE',  ( -72.65003826940696285, -23.48783264082477018, -1.443836473390095021 ) ) ;
#96595 = CARTESIAN_POINT ( 'NONE',  ( -86.62287095715004170, -24.65952944569304606, 1.056160979905700348 ) ) ;
#96596 = VERTEX_POINT ( 'NONE', #20817 ) ;
#96597 = ORIENTED_EDGE ( 'NONE', *, *, #67766, .T. ) ;
#96598 = DIRECTION ( 'NONE',  ( 0.000000000000000000, 0.000000000000000000, -1.000000000000000000 ) ) ;
#96599 = PLANE ( 'NONE',  #55121 ) ;
#96600 = DIRECTION ( 'NONE',  ( 0.000000000000000000, -1.000000000000000000, 0.000000000000000000 ) ) ;
#96601 = CARTESIAN_POINT ( 'NONE',  ( 15.21836549854886123, 13.79734045396011943, -1.500000000000002220 ) ) ;
#96602 = ORIENTED_EDGE ( 'NONE', *, *, #76504, .F. ) ;
#96603 = CARTESIAN_POINT ( 'NONE',  ( 8.160000000000000142, 1.020006686409831046E-16, 5.788828319098143105 ) ) ;
#96604 = EDGE_CURVE ( 'NONE', #76106, #88628, #51791, .T. ) ;
#96605 = LINE ( 'NONE', #48451, #15869 ) ;
#96606 = AXIS2_PLACEMENT_3D ( 'NONE', #32639, #11307, #41777 ) ;
#96607 = DIRECTION ( 'NONE',  ( 0.000000000000000000, 0.000000000000000000, 1.000000000000000000 ) ) ;
#96608 = CARTESIAN_POINT ( 'NONE',  ( -21.16112330106665240, 7.131417522999676351, -1.500000000000002220 ) ) ;
#96609 = CARTESIAN_POINT ( 'NONE',  ( -19.80875734969026425, -0.3587747205144265483, 31.02402280011862246 ) ) ;
#96610 = CARTESIAN_POINT ( 'NONE',  ( -19.80875734969026425, 0.3587747205144265483, 30.51402280011862089 ) ) ;
#96611 = EDGE_LOOP ( 'NONE', ( #19316, #50479, #94041, #95361 ) ) ;
#96612 = DIRECTION ( 'NONE',  ( 0.000000000000000000, -1.000000000000000000, 0.000000000000000000 ) ) ;
#96613 = CARTESIAN_POINT ( 'NONE',  ( -51.61954071829940460, -25.29021791842099987, 4.383826557230434240 ) ) ;
#96614 = CARTESIAN_POINT ( 'NONE',  ( 18.58881047053902691, 9.431966241625852732, 11.49999999999998934 ) ) ;
#96615 = ORIENTED_EDGE ( 'NONE', *, *, #43718, .F. ) ;
#96617 = EDGE_LOOP ( 'NONE', ( #79788, #46412 ) ) ;
#96616 = CARTESIAN_POINT ( 'NONE',  ( -64.62287095715005592, -29.50250243563736774, 8.947779886222145151 ) ) ;
#96618 = ORIENTED_EDGE ( 'NONE', *, *, #71139, .T. ) ;
#96619 = CARTESIAN_POINT ( 'NONE',  ( -41.32836283488544638, 4.132774720514426292, 39.26872235229541985 ) ) ;
#96620 = CARTESIAN_POINT ( 'NONE',  ( 0.4554788648648982474, -21.05657754196055009, -1.500000000000002220 ) ) ;
#96621 = VERTEX_POINT ( 'NONE', #75110 ) ;
#96622 = PLANE ( 'NONE',  #47854 ) ;
#96623 = CARTESIAN_POINT ( 'NONE',  ( -54.52287095715005449, -24.66019654487198665, 8.947790411086121054 ) ) ;
#96624 = DIRECTION ( 'NONE',  ( -3.773278334453079030E-23, 0.9999999999976377785, 2.173523156925979128E-06 ) ) ;
#96625 = B_SPLINE_CURVE_WITH_KNOTS ( 'NONE', 3,
 ( #13080, #90224, #99320, #75474 ),
 .UNSPECIFIED., .F., .F.,
 ( 4, 4 ),
 ( 0.2606861495984522659, 0.2696925808705678551 ),
 .UNSPECIFIED. ) ;
#96626 = CARTESIAN_POINT ( 'NONE',  ( -76.53951690088622684, -24.66019654487199375, 8.947790411086119278 ) ) ;
#96627 = CARTESIAN_POINT ( 'NONE',  ( 7.190659024148910561, -5.876774720514413630, 19.91543959911579620 ) ) ;
#96628 = CARTESIAN_POINT ( 'NONE',  ( 20.80172415560569021, 6.174449132348904357, -1.500000000000002220 ) ) ;
#96629 = CARTESIAN_POINT ( 'NONE',  ( -80.83723253079826065, -25.12224380035756610, 7.046395587628459189 ) ) ;
#96630 = EDGE_CURVE ( 'NONE', #31511, #91517, #19344, .T. ) ;
#96632 = ORIENTED_EDGE ( 'NONE', *, *, #27449, .T. ) ;
#96631 = CARTESIAN_POINT ( 'NONE',  ( -20.55991158545366204, 8.586518200734140294, 11.49999999999999645 ) ) ;
#96633 = CARTESIAN_POINT ( 'NONE',  ( -72.62287095715002749, -24.51387760970723662, 9.387446482453421837 ) ) ;
#96634 = LINE ( 'NONE', #62080, #548 ) ;
#96635 = CARTESIAN_POINT ( 'NONE',  ( -65.05438548721848235, 3.316774720514426456, 27.45402280011862572 ) ) ;
#96636 = ORIENTED_EDGE ( 'NONE', *, *, #76342, .F. ) ;
#96637 = VECTOR ( 'NONE', #66511, 1000.000000000000000 ) ;
#96639 = ORIENTED_EDGE ( 'NONE', *, *, #55698, .T. ) ;
#96638 = CARTESIAN_POINT ( 'NONE',  ( 0.6000000000000007550, 0.000000000000000000, 0.000000000000000000 ) ) ;
#96640 = VERTEX_POINT ( 'NONE', #62404 ) ;
#96641 = ADVANCED_FACE ( 'NONE', ( #8108 ), #75598, .T. ) ;
#96642 = CARTESIAN_POINT ( 'NONE',  ( 28.30015606816038698, -2.682774720514426559, -13.13501953239208930 ) ) ;
#96643 = B_SPLINE_CURVE_WITH_KNOTS ( 'NONE', 3,
 ( #97537, #29020, #58993, #52368, #82312, #20396 ),
 .UNSPECIFIED., .F., .F.,
 ( 4, 2, 4 ),
 ( 0.000000000000000000, 0.001380764517853247733, 0.002761529035706495466 ),
 .UNSPECIFIED. ) ;
#96644 = EDGE_CURVE ( 'NONE', #85772, #12600, #33921, .T. ) ;
#96645 = CARTESIAN_POINT ( 'NONE',  ( -49.34350806497818098, -25.31059326740647109, 4.644625854372842255 ) ) ;
#96646 = AXIS2_PLACEMENT_3D ( 'NONE', #70590, #1590, #40651 ) ;
#96647 = CARTESIAN_POINT ( 'NONE',  ( -87.52287095715007581, -24.50321055353806088, 9.387540953477520489 ) ) ;
#96648 = CARTESIAN_POINT ( 'NONE',  ( -51.52287095715009002, -23.72773821059536559, 11.05748984161097326 ) ) ;
#96649 = VERTEX_POINT ( 'NONE', #38051 ) ;
#96650 = VECTOR ( 'NONE', #50082, 1000.000000000000000 ) ;
#96651 = CARTESIAN_POINT ( 'NONE',  ( -130.5728709571501156, -25.00463211122487550, 1.879953029323152780 ) ) ;
#96652 = CARTESIAN_POINT ( 'NONE',  ( -22.32441756149717094, -2.617931739244098388, -1.500000000000002220 ) ) ;
#96653 = AXIS2_PLACEMENT_3D ( 'NONE', #17488, #78870, #72789 ) ;
#96654 = EDGE_CURVE ( 'NONE', #43726, #75014, #30442, .T. ) ;
#96655 = VERTEX_POINT ( 'NONE', #23823 ) ;
#96656 = DIRECTION ( 'NONE',  ( 0.000000000000000000, -1.000000000000000000, 0.000000000000000000 ) ) ;
#96657 = DIRECTION ( 'NONE',  ( -3.773278334453079618E-23, 0.9999999999976377785, 2.173523156925979975E-06 ) ) ;
#96658 = CARTESIAN_POINT ( 'NONE',  ( 2.598318274922708060, -6.376774720514413630, 19.68966562063331693 ) ) ;
#96659 = B_SPLINE_CURVE_WITH_KNOTS ( 'NONE', 3,
 ( #16540, #86567, #47516, #78441 ),
 .UNSPECIFIED., .F., .F.,
 ( 4, 4 ),
 ( 0.000000000000000000, 0.0001000000000000028644 ),
 .UNSPECIFIED. ) ;
#96660 = CARTESIAN_POINT ( 'NONE',  ( -125.5228709571500332, -24.52232992886592555, 0.6492154411970870731 ) ) ;
#96661 = VECTOR ( 'NONE', #56655, 1000.000000000000000 ) ;
#96662 = CARTESIAN_POINT ( 'NONE',  ( -63.91870386941572946, -24.82935162629096837, 1.633150109380538950 ) ) ;
#96663 = CARTESIAN_POINT ( 'NONE',  ( 16.12930680145378304, -11.13525102954884893, -1.500000000000002220 ) ) ;
#96664 = CARTESIAN_POINT ( 'NONE',  ( 33.10875634548599322, -6.475225279485573360, -11.42349945801155719 ) ) ;
#96665 = VERTEX_POINT ( 'NONE', #45180 ) ;
#96666 = CARTESIAN_POINT ( 'NONE',  ( -11.62584540149672385, -18.10649092712023389, -1.500000000000002220 ) ) ;
#96667 = CARTESIAN_POINT ( 'NONE',  ( -129.5562042904833788, -24.64965694238575722, 8.947790433994185832 ) ) ;
#96668 = CARTESIAN_POINT ( 'NONE',  ( -80.53911428444936860, -25.31572646508323743, 4.969307509984924209 ) ) ;
#96669 = CARTESIAN_POINT ( 'NONE',  ( -101.2008648890725198, -25.15877266524084988, 3.052372009152386934 ) ) ;
#96670 = CARTESIAN_POINT ( 'NONE',  ( 3.509873074917118085, -5.965225279485572685, 29.15869884040363758 ) ) ;
#96671 = CARTESIAN_POINT ( 'NONE',  ( 12.10309942457327992, -19.51426552955538085, -1.500000000000002220 ) ) ;
#96672 = PERSON_AND_ORGANIZATION ( #70597, #27821 ) ;
#96673 = DIRECTION ( 'NONE',  ( -3.773278334453079618E-23, 0.9999999999976377785, 2.173523156925979975E-06 ) ) ;
#96674 = CARTESIAN_POINT ( 'NONE',  ( -49.63955062369517890, -24.15543982623906771, -0.2315651400026657036 ) ) ;
#96675 = CARTESIAN_POINT ( 'NONE',  ( 10.48293302797296356, 17.13603372422173976, 11.49999999999999645 ) ) ;
#96676 = DIRECTION ( 'NONE',  ( 0.000000000000000000, 0.000000000000000000, 1.000000000000000000 ) ) ;
#96677 = LINE ( 'NONE', #19550, #95437 ) ;
#96678 = FACE_OUTER_BOUND ( 'NONE', #65983, .T. ) ;
#96679 = CARTESIAN_POINT ( 'NONE',  ( 15.32643653063178668, 2.682774720514426559, -27.14485409495428314 ) ) ;
#96680 = CARTESIAN_POINT ( 'NONE',  ( -16.82575997001036328, 10.57904039763333159, 11.49999999999998934 ) ) ;
#96681 = CARTESIAN_POINT ( 'NONE',  ( -19.37210865224160017, -0.3587747205143967943, -21.60955166348796297 ) ) ;
#96682 = B_SPLINE_CURVE_WITH_KNOTS ( 'NONE', 3,
 ( #48931, #26080, #50426, #96587, #27086, #56048 ),
 .UNSPECIFIED., .F., .F.,
 ( 4, 2, 4 ),
 ( 1.570887131794638196E-05, 0.001396322306279763458, 0.002776935741241580609 ),
 .UNSPECIFIED. ) ;
#96683 = CARTESIAN_POINT ( 'NONE',  ( -13.01991350253972080, 14.82018230214031895, -1.500000000000002220 ) ) ;
#96684 = VECTOR ( 'NONE', #36845, 1000.000000000000000 ) ;
#96685 = CARTESIAN_POINT ( 'NONE',  ( 15.63775912259811918, -4.567193422985928564, -28.22903731538494299 ) ) ;
#96686 = PERSON_AND_ORGANIZATION_ROLE ( 'classification_officer' ) ;
#96687 = B_SPLINE_CURVE_WITH_KNOTS ( 'NONE', 3,
 ( #83231, #13712, #99447, #22317 ),
 .UNSPECIFIED., .F., .F.,
 ( 4, 4 ),
 ( 0.000000000000000000, 0.0001000000000000028644 ),
 .UNSPECIFIED. ) ;
#96688 = CARTESIAN_POINT ( 'NONE',  ( -60.52287095715006160, -24.99156044556119838, 7.747789690856173195 ) ) ;
#96689 = FACE_OUTER_BOUND ( 'NONE', #17479, .T. ) ;
#96690 = CARTESIAN_POINT ( 'NONE',  ( -18.09956831669839872, 9.893135806712603397, 11.49999999999999645 ) ) ;
#96691 = VECTOR ( 'NONE', #69575, 1000.000000000000114 ) ;
#96692 = CARTESIAN_POINT ( 'NONE',  ( -33.55620429048339304, -23.47596703998600276, 11.44779298504227505 ) ) ;
#96694 = ADVANCED_FACE ( 'NONE', ( #83223 ), #68509, .F. ) ;
#96693 = CARTESIAN_POINT ( 'NONE',  ( 17.19246737676917292, 14.74310579602587090, 11.49999999999999645 ) ) ;
#96695 = VERTEX_POINT ( 'NONE', #44678 ) ;
#96696 = CARTESIAN_POINT ( 'NONE',  ( -31.24388727629348494, -24.86181185134534388, 1.747789972853592610 ) ) ;
#96697 = CARTESIAN_POINT ( 'NONE',  ( -56.52287095715009002, -23.96127896941632329, -0.6493128931038024687 ) ) ;
#96698 = CARTESIAN_POINT ( 'NONE',  ( -110.6228709571501128, -24.91570333823101180, 8.075032458375558164 ) ) ;
#96699 = CARTESIAN_POINT ( 'NONE',  ( -128.6228709571500417, -24.65952944569305316, 1.056160979905707897 ) ) ;
#96700 = VERTEX_POINT ( 'NONE', #53792 ) ;
#96701 = VECTOR ( 'NONE', #59619, 1000.000000000000114 ) ;
#96702 = ORIENTED_EDGE ( 'NONE', *, *, #80012, .T. ) ;
#96703 = CARTESIAN_POINT ( 'NONE',  ( -98.55620429048339304, -23.47596703998600631, 11.44779298504227683 ) ) ;
#96704 = CARTESIAN_POINT ( 'NONE',  ( -18.82434810282327220, -12.99595988342530362, 11.49999999999998934 ) ) ;
#96705 = CARTESIAN_POINT ( 'NONE',  ( -29.49875734969026198, -0.3587747205144265483, 2.362022800118626531 ) ) ;
#96706 = CARTESIAN_POINT ( 'NONE',  ( 11.83326311654409935, 18.06170320929925310, -1.500000000000002220 ) ) ;
#96707 = CARTESIAN_POINT ( 'NONE',  ( -113.5177876307711529, -24.15620529776628800, 10.23563542870659582 ) ) ;
#96708 = DIRECTION ( 'NONE',  ( -1.000000000000000000, -0.000000000000000000, -0.000000000000000000 ) ) ;
#96709 = CARTESIAN_POINT ( 'NONE',  ( 3.368619518803146029, -22.26131067175759881, 11.49999999999999645 ) ) ;
#96710 = ORIENTED_EDGE ( 'NONE', *, *, #33412, .T. ) ;
#96711 = CARTESIAN_POINT ( 'NONE',  ( -36.55620429048340014, -23.47596703998600276, 11.44779298504227505 ) ) ;
#96712 = CARTESIAN_POINT ( 'NONE',  ( 12.42595048307055983, -18.10569578304522764, 11.49999999999998934 ) ) ;
#96713 = CIRCLE ( 'NONE', #52981, 1.306876713926001354 ) ;
#96714 = EDGE_CURVE ( 'NONE', #96746, #66619, #69003, .T. ) ;
#96715 = DIRECTION ( 'NONE',  ( 1.000000000000000000, 3.773278334444167608E-23, 8.201307833595939069E-29 ) ) ;
#96716 = CARTESIAN_POINT ( 'NONE',  ( -29.10172430483776651, -24.79700049711173193, 6.373704971587772050 ) ) ;
#96717 = ORIENTED_EDGE ( 'NONE', *, *, #49799, .T. ) ;
#96718 = CARTESIAN_POINT ( 'NONE',  ( -110.5228709571500616, -29.50247984919015209, -1.443849546365048253 ) ) ;
#96719 = DIRECTION ( 'NONE',  ( 0.000000000000000000, 0.000000000000000000, -1.000000000000000000 ) ) ;
#96720 = ORIENTED_EDGE ( 'NONE', *, *, #88684, .T. ) ;
#96721 = VECTOR ( 'NONE', #77249, 1000.000000000000000 ) ;
#96722 = CARTESIAN_POINT ( 'NONE',  ( -20.27875734969026311, -6.376774720514428729, 27.00402280011862288 ) ) ;
#96723 = CARTESIAN_POINT ( 'NONE',  ( 6.429960413904108663, -19.47341730443774921, -1.500000000000002220 ) ) ;
#96724 = EDGE_CURVE ( 'NONE', #9882, #67600, #68017, .T. ) ;
#96725 = VERTEX_POINT ( 'NONE', #60414 ) ;
#96726 = CIRCLE ( 'NONE', #88626, 130.2784398600581710 ) ;
#96727 = EDGE_LOOP ( 'NONE', ( #51960, #35952, #95465, #3399 ) ) ;
#96728 = ORIENTED_EDGE ( 'NONE', *, *, #79470, .F. ) ;
#96729 = DIRECTION ( 'NONE',  ( 0.000000000000000000, 0.000000000000000000, -1.000000000000000000 ) ) ;
#96730 = DIRECTION ( 'NONE',  ( -3.773278334453079030E-23, 0.9999999999976377785, 2.173523156925979128E-06 ) ) ;
#96731 = CARTESIAN_POINT ( 'NONE',  ( -104.5196637104627087, -23.73791477778912196, 11.05961554403170410 ) ) ;
#96732 = B_SPLINE_CURVE_WITH_KNOTS ( 'NONE', 3,
 ( #24019, #17418, #31633, #70206 ),
 .UNSPECIFIED., .F., .F.,
 ( 4, 4 ),
 ( 0.7292979254729236027, 0.7302986725136889623 ),
 .UNSPECIFIED. ) ;
#96733 = CARTESIAN_POINT ( 'NONE',  ( -3.780122020211411193, 19.97858748211865532, -1.500000000000002220 ) ) ;
#96734 = ORIENTED_EDGE ( 'NONE', *, *, #64265, .F. ) ;
#96735 = CARTESIAN_POINT ( 'NONE',  ( -71.63981544056943562, -25.19546925735422960, 6.637203831572652035 ) ) ;
#96736 = ADVANCED_FACE ( 'NONE', ( #38555 ), #77102, .T. ) ;
#96737 = CARTESIAN_POINT ( 'NONE',  ( -29.52199316675947216, -23.40095854392973607, 11.44779303447556806 ) ) ;
#96738 = AXIS2_PLACEMENT_3D ( 'NONE', #60972, #99502, #69578 ) ;
#96739 = EDGE_CURVE ( 'NONE', #79117, #44715, #69512, .T. ) ;
#96740 = CARTESIAN_POINT ( 'NONE',  ( -105.5864570552434714, -24.83618233451450408, 1.606449574219534826 ) ) ;
#96741 = CARTESIAN_POINT ( 'NONE',  ( -70.87191485471986141, -25.25855360924004245, 7.466451555984895627 ) ) ;
#96742 = ORIENTED_EDGE ( 'NONE', *, *, #9109, .F. ) ;
#96743 = CARTESIAN_POINT ( 'NONE',  ( -28.57654128002459260, -25.21531733429936750, 2.620673301919582254 ) ) ;
#96744 = LINE ( 'NONE', #20609, #49109 ) ;
#96745 = EDGE_CURVE ( 'NONE', #66223, #8977, #87433, .T. ) ;
#96746 = VERTEX_POINT ( 'NONE', #99930 ) ;
#96747 = CARTESIAN_POINT ( 'NONE',  ( -18.43438512255917772, -9.567967903218889347, 11.49999999999998934 ) ) ;
#96748 = VERTEX_POINT ( 'NONE', #83724 ) ;
#96750 = ORIENTED_EDGE ( 'NONE', *, *, #21019, .F. ) ;
#96749 = DIRECTION ( 'NONE',  ( 0.000000000000000000, 0.000000000000000000, 1.000000000000000000 ) ) ;
#96751 = CARTESIAN_POINT ( 'NONE',  ( -120.5228709571501184, -23.48783264082477373, -1.443836473390081698 ) ) ;
#96752 = CARTESIAN_POINT ( 'NONE',  ( 13.91401389203221406, 3.316774720514426456, 158.0376437107427137 ) ) ;
#96753 = ORIENTED_EDGE ( 'NONE', *, *, #20331, .T. ) ;
#96754 = VERTEX_POINT ( 'NONE', #91835 ) ;
#96755 = CARTESIAN_POINT ( 'NONE',  ( -112.5895376238167245, -23.48783264082479150, -1.443836473390060160 ) ) ;
#96756 = DIRECTION ( 'NONE',  ( 0.3133898629642195011, -5.365801633547218220E-16, -0.9496245541219264785 ) ) ;
#96757 = CARTESIAN_POINT ( 'NONE',  ( -52.62287095715002749, -24.51387760970724372, 9.387446482453430718 ) ) ;
#96758 = CARTESIAN_POINT ( 'NONE',  ( -70.82359880940848029, -25.31201612284975155, 5.413474107398605462 ) ) ;
#96759 = EDGE_CURVE ( 'NONE', #24715, #5012, #67774, .T. ) ;
#96761 = ORIENTED_EDGE ( 'NONE', *, *, #40753, .T. ) ;
#96760 = CARTESIAN_POINT ( 'NONE',  ( 21.80885565983754404, 3.581153529568561478, 11.49999999999999645 ) ) ;
#96762 = CARTESIAN_POINT ( 'NONE',  ( -103.5510089839001466, -24.34968618360933945, 0.1864209137778842229 ) ) ;
#96763 = CARTESIAN_POINT ( 'NONE',  ( -17.13258802378025791, -14.77425600068537115, 11.49999999999998934 ) ) ;
#96764 = AXIS2_PLACEMENT_3D ( 'NONE', #87531, #26632, #27634 ) ;
#96766 = ORIENTED_EDGE ( 'NONE', *, *, #35260, .T. ) ;
#96765 = CARTESIAN_POINT ( 'NONE',  ( -115.6250716495462569, -24.73531770709096023, 8.716586749053508498 ) ) ;
#96767 = VERTEX_POINT ( 'NONE', #42546 ) ;
#96768 = CIRCLE ( 'NONE', #53029, 1.699999999999999289 ) ;
#96769 = FACE_OUTER_BOUND ( 'NONE', #86371, .T. ) ;
#96770 = ADVANCED_FACE ( 'NONE', ( #61906 ), #92831, .F. ) ;
#96771 = EDGE_CURVE ( 'NONE', #57524, #33368, #54298, .T. ) ;
#96772 = DIRECTION ( 'NONE',  ( 0.000000000000000000, 0.000000000000000000, 1.000000000000000000 ) ) ;
#96773 = ORIENTED_EDGE ( 'NONE', *, *, #58245, .F. ) ;
#96774 = CARTESIAN_POINT ( 'NONE',  ( -13.58512445790048417, 16.25115196636789250, 11.49999999999998934 ) ) ;
#96775 = CARTESIAN_POINT ( 'NONE',  ( -7.326695514711824231, -5.876774720514417183, 20.26757654895259719 ) ) ;
#96776 = CARTESIAN_POINT ( 'NONE',  ( -41.52600572741248897, -25.30531391451519596, 5.104681448486787509 ) ) ;
#96777 = CARTESIAN_POINT ( 'NONE',  ( 18.07686251855496096, -12.98574554580779861, -1.500000000000002220 ) ) ;
#96778 = DIRECTION ( 'NONE',  ( 3.773278334444167608E-23, -1.000000000000000000, 0.000000000000000000 ) ) ;
#96779 = EDGE_CURVE ( 'NONE', #35328, #75907, #6605, .T. ) ;
#96780 = ORIENTED_EDGE ( 'NONE', *, *, #57979, .T. ) ;
#96781 = LINE ( 'NONE', #91157, #33553 ) ;
#96782 = DIRECTION ( 'NONE',  ( -3.773278334453079030E-23, 0.9999999999976377785, 2.173523156925979128E-06 ) ) ;
#96783 = AXIS2_PLACEMENT_3D ( 'NONE', #9670, #95901, #65986 ) ;
#96784 = EDGE_CURVE ( 'NONE', #1643, #16488, #38633, .T. ) ;
#96785 = CARTESIAN_POINT ( 'NONE',  ( -36.57019847237913979, -23.48786465467240347, 11.44779295918255180 ) ) ;
#96786 = DIRECTION ( 'NONE',  ( 0.000000000000000000, 0.000000000000000000, 1.000000000000000000 ) ) ;
#96787 = EDGE_CURVE ( 'NONE', #26613, #39625, #80926, .T. ) ;
#96788 = CARTESIAN_POINT ( 'NONE',  ( -19.51626497420292239, -0.3564122556526727048, -1.500000000000002220 ) ) ;
#96789 = CARTESIAN_POINT ( 'NONE',  ( -16.73372362409233105, 13.38858591273363174, 11.49999999999998934 ) ) ;
#96790 = CARTESIAN_POINT ( 'NONE',  ( -26.25707451207771470, -24.92774811677663038, 2.297366685435383360 ) ) ;
#96791 = CARTESIAN_POINT ( 'NONE',  ( 0.000000000000000000, 0.000000000000000000, 0.000000000000000000 ) ) ;
#96792 = CARTESIAN_POINT ( 'NONE',  ( -77.58809874021086728, -24.34968618360934300, 0.1864209137778811143 ) ) ;
#96793 = CARTESIAN_POINT ( 'NONE',  ( 16.42120958226126604, -15.83219868413775622, -1.500000000000002220 ) ) ;
#96794 = CIRCLE ( 'NONE', #15798, 130.2784398600581710 ) ;
#96795 = B_SPLINE_CURVE_WITH_KNOTS ( 'NONE', 3,
 ( #14549, #98279, #28786, #99284, #89690, #60748 ),
 .UNSPECIFIED., .F., .F.,
 ( 4, 2, 4 ),
 ( 0.000000000000000000, 0.001380764517853253154, 0.002761529035706506308 ),
 .UNSPECIFIED. ) ;
#96796 = DIRECTION ( 'NONE',  ( -3.498155634913392171E-15, 0.0002585596332610844150, -0.9999999665734575771 ) ) ;
#96797 = CARTESIAN_POINT ( 'NONE',  ( -98.50757086102233018, -24.65952944569305316, 1.056160979905702124 ) ) ;
#96798 = DIRECTION ( 'NONE',  ( -0.000000000000000000, 0.9513357669802769978, -0.3081562241202472907 ) ) ;
#96799 = CARTESIAN_POINT ( 'NONE',  ( 18.73470368118781693, 6.836574088118649861, 11.49999999999999645 ) ) ;
#96800 = CARTESIAN_POINT ( 'NONE',  ( -78.52287095715006160, -24.64898659630367916, 1.056161002820826145 ) ) ;
#96801 = CIRCLE ( 'NONE', #44952, 3.500000000000000000 ) ;
#96802 = CARTESIAN_POINT ( 'NONE',  ( 17.47419131657910540, -5.965225279485572685, 28.31804950686278843 ) ) ;
#96803 = B_SPLINE_CURVE_WITH_KNOTS ( 'NONE', 3,
 ( #19370, #10770, #89388, #58455 ),
 .UNSPECIFIED., .F., .F.,
 ( 4, 4 ),
 ( 2.775557561562891043E-17, 0.0001000000000000167422 ),
 .UNSPECIFIED. ) ;
#96804 = CARTESIAN_POINT ( 'NONE',  ( -98.55620429048340725, -23.47593901973091235, -1.443836447539001089 ) ) ;
#96805 = ORIENTED_EDGE ( 'NONE', *, *, #80131, .F. ) ;
#96806 = CARTESIAN_POINT ( 'NONE',  ( -65.52287095715006160, -24.99156044556202616, 7.747789690856173195 ) ) ;
#96807 = CARTESIAN_POINT ( 'NONE',  ( 9.940598223437573822, -5.876774720514426953, 21.78128695274315874 ) ) ;
#96808 = CARTESIAN_POINT ( 'NONE',  ( -17.03913561245058261, -13.47071831616118942, -1.500000000000002220 ) ) ;
#96809 = CARTESIAN_POINT ( 'NONE',  ( -51.16651589987333182, -25.07168895645787643, 7.427142928140856526 ) ) ;
#96810 = CARTESIAN_POINT ( 'NONE',  ( -10.28394983263804185, -16.58134856480417341, -1.500000000000002220 ) ) ;
#96811 = CARTESIAN_POINT ( 'NONE',  ( 22.81105451610979173, -1.477225279485574028, -18.46691820600746681 ) ) ;
#96812 = DATE_AND_TIME ( #93927, #49058 ) ;
#96813 = CARTESIAN_POINT ( 'NONE',  ( -51.62287095715005592, -24.66019654487199020, 8.947790411086135265 ) ) ;
#96814 = CARTESIAN_POINT ( 'NONE',  ( -19.37329759448073574, 6.469241145865432863, 11.49999999999999645 ) ) ;
#96815 = LINE ( 'NONE', #28800, #73240 ) ;
#96816 = CARTESIAN_POINT ( 'NONE',  ( -89.52287095715009002, -23.72747288104470087, -1.053458166803225682 ) ) ;
#96817 = ORIENTED_EDGE ( 'NONE', *, *, #18978, .F. ) ;
#96818 = CARTESIAN_POINT ( 'NONE',  ( 2.000000000000000000, 0.000000000000000000, 6.099999999999999645 ) ) ;
#96819 = DIRECTION ( 'NONE',  ( 1.000000000000000000, 0.000000000000000000, 0.000000000000000000 ) ) ;
#96820 = CARTESIAN_POINT ( 'NONE',  ( -116.5903533738907498, -24.15620529776629155, 10.23563542870659759 ) ) ;
#96821 = CARTESIAN_POINT ( 'NONE',  ( -63.62287095715007723, -23.47596703998600631, 11.44779298504227683 ) ) ;
#96822 = ORIENTED_EDGE ( 'NONE', *, *, #71839, .T. ) ;
#96823 = DIRECTION ( 'NONE',  ( 0.000000000000000000, 0.000000000000000000, 1.000000000000000000 ) ) ;
#96824 = VECTOR ( 'NONE', #99859, 1000.000000000000000 ) ;
#96825 = CARTESIAN_POINT ( 'NONE',  ( -1.485350438481424895, -22.96994831426971828, 11.49999999999999645 ) ) ;
#96826 = CARTESIAN_POINT ( 'NONE',  ( -20.37646751746074969, -10.17465561509698979, 11.49999999999998934 ) ) ;
#96827 = CARTESIAN_POINT ( 'NONE',  ( -110.5493961576417519, -24.83644354573579349, 8.397322867130096569 ) ) ;
#96828 = B_SPLINE_SURFACE_WITH_KNOTS ( 'NONE', 3, 3, ( 
 ( #57428, #18344, #11719, #56925 ),
 ( #42699, #18834, #27464, #49309 ),
 ( #73633, #57926, #87856, #35074 ),
 ( #66552, #88867, #20320, #80240 ),
 ( #10734, #96964, #34076, #26465 ),
 ( #58423, #35574, #97463, #27953 ),
 ( #89850, #51293, #60419, #7109 ) ),
 .UNSPECIFIED., .F., .F., .F.,
 ( 4, 3, 4 ),
 ( 4, 4 ),
 ( 0.0004766839783834262941, 0.1029713700210900945, 0.2054660560637967537 ),
 ( 0.9797432271868353748, 0.9812080034676798901 ),
 .UNSPECIFIED. ) ;
#96829 = CARTESIAN_POINT ( 'NONE',  ( 30.53060340732036337, 5.329285123471892760, 3.289350009555732868 ) ) ;
#96830 = CARTESIAN_POINT ( 'NONE',  ( -120.5228709571500616, -23.47596703998600631, 11.44779298504227860 ) ) ;
#96831 = CIRCLE ( 'NONE', #27165, 0.8159999999999469900 ) ;
#96832 = CARTESIAN_POINT ( 'NONE',  ( -54.52287095715008292, -24.51283580621365132, 0.6167428607019751485 ) ) ;
#96833 = DIRECTION ( 'NONE',  ( 0.000000000000000000, -1.000000000000000000, 0.000000000000000000 ) ) ;
#96834 = CARTESIAN_POINT ( 'NONE',  ( -3.281320334969873631, 21.64054093270537393, -1.500000000000002220 ) ) ;
#96835 = CARTESIAN_POINT ( 'NONE',  ( -69.59707406421517817, -23.96169478059712787, 10.65365249895718414 ) ) ;
#96836 = ADVANCED_FACE ( 'NONE', ( #64928 ), #18223, .T. ) ;
#96837 = LINE ( 'NONE', #28828, #10406 ) ;
#96838 = CARTESIAN_POINT ( 'NONE',  ( 6.573941812937369455, -0.2639660507643297183, -9.295380466955404257E-16 ) ) ;
#96839 = CARTESIAN_POINT ( 'NONE',  ( -96.52287095715009002, -23.72773821059536914, 11.05748984161097681 ) ) ;
#96840 = EDGE_LOOP ( 'NONE', ( #24207, #21832, #17502, #84858 ) ) ;
#96841 = EDGE_CURVE ( 'NONE', #33323, #76880, #94338, .T. ) ;
#96842 = PRODUCT_DEFINITION_SHAPE ( 'NONE', 'NONE',  #34522 ) ;
#96843 = CARTESIAN_POINT ( 'NONE',  ( 9.511415417357532931, -18.05363124325620205, 11.49999999999998934 ) ) ;
#96844 = ORIENTED_EDGE ( 'NONE', *, *, #78757, .F. ) ;
#96845 = ORIENTED_EDGE ( 'NONE', *, *, #76677, .T. ) ;
#96846 = ORIENTED_EDGE ( 'NONE', *, *, #51977, .T. ) ;
#96847 = EDGE_LOOP ( 'NONE', ( #31598, #80784, #58319, #19707 ) ) ;
#96848 = CARTESIAN_POINT ( 'NONE',  ( -1.485350438481424895, -22.96994831426971828, -1.500000000000002220 ) ) ;
#96849 = DIRECTION ( 'NONE',  ( -3.773278334453079618E-23, 0.9999999999976377785, 2.173523156925979975E-06 ) ) ;
#96850 = CARTESIAN_POINT ( 'NONE',  ( 12.43249465596513126, -15.92577207200969092, -1.500000000000002220 ) ) ;
#96851 = ORIENTED_EDGE ( 'NONE', *, *, #54041, .T. ) ;
#96852 = CARTESIAN_POINT ( 'NONE',  ( -67.62287095715002749, -23.96177878511307568, 10.65340807706330395 ) ) ;
#96853 = EDGE_CURVE ( 'NONE', #95824, #33348, #55802, .T. ) ;
#96854 = AXIS2_PLACEMENT_3D ( 'NONE', #2089, #86801, #77672 ) ;
#96855 = LINE ( 'NONE', #80130, #49880 ) ;
#96856 = EDGE_CURVE ( 'NONE', #41756, #96886, #35059, .T. ) ;
#96857 = DIRECTION ( 'NONE',  ( 0.000000000000000000, 1.478457507934778393E-16, -1.000000000000000000 ) ) ;
#96858 = LINE ( 'NONE', #97845, #86941 ) ;
#96860 = ORIENTED_EDGE ( 'NONE', *, *, #40279, .F. ) ;
#96859 = CARTESIAN_POINT ( 'NONE',  ( 16.79701800048795590, -13.18750964578662455, 11.49999999999999645 ) ) ;
#96861 = CARTESIAN_POINT ( 'NONE',  ( 1.305682803664691249, -0.3587747205144265483, 29.57950906855421991 ) ) ;
#96862 = ADVANCED_FACE ( 'NONE', ( #17724 ), #59048, .T. ) ;
#96863 = ORIENTED_EDGE ( 'NONE', *, *, #55162, .F. ) ;
#96864 = CARTESIAN_POINT ( 'NONE',  ( -17.34812393562427246, -13.96779696820907191, 11.49999999999998934 ) ) ;
#96865 = CARTESIAN_POINT ( 'NONE',  ( 18.27903665858761073, 9.701928907310005457, 11.49999999999998934 ) ) ;
#96866 = VECTOR ( 'NONE', #29464, 1000.000000000000000 ) ;
#96867 = EDGE_LOOP ( 'NONE', ( #100348, #92108, #20252, #78420 ) ) ;
#96868 = CARTESIAN_POINT ( 'NONE',  ( 2.968164339864655332, -5.876774720514408301, 19.33154224050496595 ) ) ;
#96869 = ORIENTED_EDGE ( 'NONE', *, *, #8120, .F. ) ;
#96870 = DIRECTION ( 'NONE',  ( 1.000000000000000000, 0.000000000000000000, 0.000000000000000000 ) ) ;
#96871 = VECTOR ( 'NONE', #51742, 1000.000000000000114 ) ;
#96872 = ORIENTED_EDGE ( 'NONE', *, *, #37751, .T. ) ;
#96873 = CARTESIAN_POINT ( 'NONE',  ( 12.20502328318355545, -3.316774720514426011, -28.10533714397569582 ) ) ;
#96874 = CARTESIAN_POINT ( 'NONE',  ( -18.08314111433443827, -10.61732331186343004, -1.500000000000002220 ) ) ;
#96875 = EDGE_CURVE ( 'NONE', #27980, #90388, #94346, .T. ) ;
#96876 = CARTESIAN_POINT ( 'NONE',  ( 21.48171311866277122, -4.276277801222842179, 11.49999999999999645 ) ) ;
#96877 = CARTESIAN_POINT ( 'NONE',  ( -26.80323004365396145, -24.89279929861774221, 7.264870854583937110 ) ) ;
#96878 = CARTESIAN_POINT ( 'NONE',  ( -22.36795837939145670, 2.692536522722862813, -1.500000000000002220 ) ) ;
#96879 = CARTESIAN_POINT ( 'NONE',  ( 7.117523389609132778, 19.69228268689324324, -1.500000000000002220 ) ) ;
#96880 = CARTESIAN_POINT ( 'NONE',  ( -110.5228709571500190, -24.91544648472626378, 1.928969306349433532 ) ) ;
#96881 = CARTESIAN_POINT ( 'NONE',  ( 6.059061188053544988, -6.376774720514417183, 20.16803580207560742 ) ) ;
#96882 = CARTESIAN_POINT ( 'NONE',  ( -29.62287095715003460, -24.43778075029778307, 9.387565086202728892 ) ) ;
#96883 = DIRECTION ( 'NONE',  ( -0.000000000000000000, 1.000000000000000000, -0.000000000000000000 ) ) ;
#96885 = ORIENTED_EDGE ( 'NONE', *, *, #38762, .F. ) ;
#96884 = EDGE_CURVE ( 'NONE', #11920, #98613, #999, .T. ) ;
#96886 = VERTEX_POINT ( 'NONE', #40569 ) ;
#96887 = ORIENTED_EDGE ( 'NONE', *, *, #45422, .T. ) ;
#96888 = CYLINDRICAL_SURFACE ( 'NONE', #62813, 21.89999999999999858 ) ;
#96889 = EDGE_LOOP ( 'NONE', ( #62941, #61205, #2824, #52302 ) ) ;
#96890 = ADVANCED_FACE ( 'NONE', ( #10107 ), #69649, .T. ) ;
#96891 = CARTESIAN_POINT ( 'NONE',  ( -21.47443924280258187, -0.1944818460393343829, -1.500000000000002220 ) ) ;
#96892 = DIRECTION ( 'NONE',  ( 0.000000000000000000, -0.000000000000000000, -1.000000000000000000 ) ) ;
#96893 = ORIENTED_EDGE ( 'NONE', *, *, #31078, .F. ) ;
#96894 = CARTESIAN_POINT ( 'NONE',  ( 18.35617536642501690, 10.39506492455470088, 11.49999999999998934 ) ) ;
#96895 = CARTESIAN_POINT ( 'NONE',  ( 8.971512145086528278, -9.528487854913501920, 6.500000000000001776 ) ) ;
#96896 = CARTESIAN_POINT ( 'NONE',  ( 2.708118538500707828, -6.376774720514424288, 20.94830092343283212 ) ) ;
#96897 = CARTESIAN_POINT ( 'NONE',  ( -43.52287095715007581, -24.66019654487199375, 8.947790411086128159 ) ) ;
#96898 = CARTESIAN_POINT ( 'NONE',  ( -41.62287095715006302, -29.50248528299804818, 1.056150453629031594 ) ) ;
#96899 = CARTESIAN_POINT ( 'NONE',  ( -129.5559602451679666, -23.96169478059714208, 10.65365249895717348 ) ) ;
#96900 = CARTESIAN_POINT ( 'NONE',  ( -21.04927197579530329, -6.814310187297170529, -1.500000000000002220 ) ) ;
#96901 = ORIENTED_EDGE ( 'NONE', *, *, #39610, .T. ) ;
#96902 = CARTESIAN_POINT ( 'NONE',  ( -81.54693475870598718, -24.35071581493543036, 9.817618358456037697 ) ) ;
#96903 = CARTESIAN_POINT ( 'NONE',  ( -78.52287095715006160, -23.47593901973090169, -1.443836447538996648 ) ) ;
#96904 = CARTESIAN_POINT ( 'NONE',  ( -41.77207742203299290, -25.27955894647979918, 4.730364241316486584 ) ) ;
#96905 = EDGE_CURVE ( 'NONE', #40078, #52247, #93071, .T. ) ;
#96906 = CARTESIAN_POINT ( 'NONE',  ( -62.58762325277358940, -24.35071581493542325, 9.817618358456032368 ) ) ;
#96907 = CARTESIAN_POINT ( 'NONE',  ( 33.74607884027702909, -0.3587747205144265483, -4.999864028243830916 ) ) ;
#96908 = CARTESIAN_POINT ( 'NONE',  ( -13.85510387911049079, -16.26762222697724880, 11.49999999999998934 ) ) ;
#96909 = CARTESIAN_POINT ( 'NONE',  ( -26.33488822642538452, -24.89212854592702584, 6.524121854850513991 ) ) ;
#96910 = CARTESIAN_POINT ( 'NONE',  ( -50.92286199449029738, -25.11539320716599377, 2.804431449967496714 ) ) ;
#96911 = EDGE_CURVE ( 'NONE', #40199, #63330, #54998, .T. ) ;
#96912 = CARTESIAN_POINT ( 'NONE',  ( -64.59268078241893818, -24.15620529776628445, 10.23563542870660115 ) ) ;
#96913 = DIRECTION ( 'NONE',  ( -0.2164396139380965756, 0.9762960071199346945, 0.000000000000000000 ) ) ;
#96914 = CARTESIAN_POINT ( 'NONE',  ( -21.70561270324154179, 6.225854807558039994, -1.500000000000002220 ) ) ;
#96915 = B_SPLINE_CURVE_WITH_KNOTS ( 'NONE', 3,
 ( #54728, #23248, #76035, #8033 ),
 .UNSPECIFIED., .F., .F.,
 ( 4, 4 ),
 ( 1.387778780781445521E-17, 9.999999999998898659E-05 ),
 .UNSPECIFIED. ) ;
#96916 = B_SPLINE_SURFACE_WITH_KNOTS ( 'NONE', 3, 1, ( 
 ( #50762, #49773 ),
 ( #4589, #81203 ),
 ( #42165, #26918 ),
 ( #74096, #35037 ),
 ( #67482, #90310 ),
 ( #97423, #97908 ),
 ( #28401, #35539 ),
 ( #20781, #59367 ),
 ( #13171, #11193 ),
 ( #66996, #44142 ),
 ( #58872, #80704 ) ),
 .UNSPECIFIED., .F., .F., .F.,
 ( 4, 1, 1, 1, 1, 1, 1, 1, 4 ),
 ( 2, 2 ),
 ( 0.000000000000000000, 0.1182713048357273283, 0.2361775330837587172, 0.3556629329485013757, 0.4759041646706790307, 0.6001273417110856156, 0.7286081161551152263, 0.8613134756739386777, 1.000000000000000000 ),
 ( 0.000000000000000000, 1.000000000000000000 ),
 .UNSPECIFIED. ) ;
#96917 = DIRECTION ( 'NONE',  ( -0.03244919754393515293, 0.000000000000000000, 0.9994733861282923959 ) ) ;
#96918 = ORIENTED_EDGE ( 'NONE', *, *, #32810, .F. ) ;
#96919 = CARTESIAN_POINT ( 'NONE',  ( 4.653494883475234545, -5.876774720514415407, 20.13747874360300116 ) ) ;
#96920 = CARTESIAN_POINT ( 'NONE',  ( -79.62650269055158958, -24.51314013834315375, 0.6176544820404122893 ) ) ;
#96921 = CARTESIAN_POINT ( 'NONE',  ( -13.01991350253972080, 14.82018230214031895, 11.49999999999999645 ) ) ;
#96922 = CARTESIAN_POINT ( 'NONE',  ( -32.52287095715003318, -24.66019654487198665, 8.947790411086131712 ) ) ;
#96923 = CARTESIAN_POINT ( 'NONE',  ( -67.64620999989506345, -23.73766607897670511, -1.055555164236457788 ) ) ;
#96924 = ORIENTED_EDGE ( 'NONE', *, *, #99121, .T. ) ;
#96925 = B_SPLINE_CURVE_WITH_KNOTS ( 'NONE', 3,
 ( #32535, #33040, #88836, #41161, #72611, #71609 ),
 .UNSPECIFIED., .F., .F.,
 ( 4, 2, 4 ),
 ( 1.570887131794952276E-05, 0.001396322306279766060, 0.002776935741241582344 ),
 .UNSPECIFIED. ) ;
#96926 = CARTESIAN_POINT ( 'NONE',  ( 9.032095062437601740, -5.965225279485574461, -28.07116626896318579 ) ) ;
#96927 = CARTESIAN_POINT ( 'NONE',  ( -70.52287095715006160, -24.63345952396257488, 9.038047939301513622 ) ) ;
#96928 = FACE_OUTER_BOUND ( 'NONE', #64857, .T. ) ;
#96929 = CARTESIAN_POINT ( 'NONE',  ( -14.23256820581467785, 16.29125061305494526, 11.49999999999998934 ) ) ;
#96930 = DIRECTION ( 'NONE',  ( -1.000000000000000000, -3.773278334444166432E-23, -8.201307841325785021E-29 ) ) ;
#96931 = AXIS2_PLACEMENT_3D ( 'NONE', #86563, #75822, #42904 ) ;
#96932 = CARTESIAN_POINT ( 'NONE',  ( 0.06232057257353295493, 19.38168652127415825, -1.500000000000002220 ) ) ;
#96933 = DIRECTION ( 'NONE',  ( 3.639962309748244178E-15, -1.000000000000000000, -2.135627652102599075E-15 ) ) ;
#96934 = CARTESIAN_POINT ( 'NONE',  ( -118.5895376238167245, -24.64965694238575367, 8.947790433994191162 ) ) ;
#96935 = CARTESIAN_POINT ( 'NONE',  ( -19.69265041987409859, 1.759638296948408787, -1.500000000000002220 ) ) ;
#96936 = ORIENTED_EDGE ( 'NONE', *, *, #60456, .F. ) ;
#96937 = CARTESIAN_POINT ( 'NONE',  ( -18.19507518397214341, 8.946258903265221107, 11.49999999999999645 ) ) ;
#96938 = FACE_OUTER_BOUND ( 'NONE', #30115, .T. ) ;
#96939 = AXIS2_PLACEMENT_3D ( 'NONE', #100286, #39420, #47041 ) ;
#96940 = CARTESIAN_POINT ( 'NONE',  ( 5.864225667603142789, -6.376774720514424288, 21.27837265517432996 ) ) ;
#96941 = VERTEX_POINT ( 'NONE', #82116 ) ;
#96942 = CARTESIAN_POINT ( 'NONE',  ( 8.071512145086531476, -9.528487854913507249, -4.499999999999994671 ) ) ;
#96943 = DIRECTION ( 'NONE',  ( 0.000000000000000000, -1.000000000000000000, 0.000000000000000000 ) ) ;
#96944 = VECTOR ( 'NONE', #52275, 1000.000000000000000 ) ;
#96945 = FACE_OUTER_BOUND ( 'NONE', #51087, .T. ) ;
#96946 = DIRECTION ( 'NONE',  ( 0.000000000000000000, 0.000000000000000000, 1.000000000000000000 ) ) ;
#96947 = CARTESIAN_POINT ( 'NONE',  ( 7.608091486120485136, 18.53616061196756704, 11.49999999999998934 ) ) ;
#96948 = PLANE ( 'NONE',  #17558 ) ;
#96949 = ORIENTED_EDGE ( 'NONE', *, *, #43351, .T. ) ;
#96950 = AXIS2_PLACEMENT_3D ( 'NONE', #50279, #81221, #11697 ) ;
#96951 = DIRECTION ( 'NONE',  ( 0.000000000000000000, 0.000000000000000000, 1.000000000000000000 ) ) ;
#96952 = CARTESIAN_POINT ( 'NONE',  ( -86.62287095715004170, -23.47593901973091235, -1.443836447539002865 ) ) ;
#96953 = CARTESIAN_POINT ( 'NONE',  ( -79.34849387871311421, -25.27322973831870101, 5.891565427895725016 ) ) ;
#96954 = DIRECTION ( 'NONE',  ( 0.000000000000000000, -1.000000000000000000, 0.000000000000000000 ) ) ;
#96955 = CARTESIAN_POINT ( 'NONE',  ( -73.58435453540160154, -24.51314013834315375, 0.6176544820404104019 ) ) ;
#96956 = DIRECTION ( 'NONE',  ( 0.000000000000000000, 0.000000000000000000, -1.000000000000000000 ) ) ;
#96957 = CARTESIAN_POINT ( 'NONE',  ( -71.58953762381672448, -24.66019654487198665, 8.947790411086131712 ) ) ;
#96958 = EDGE_LOOP ( 'NONE', ( #83340, #54583, #23066, #94134, #70441 ) ) ;
#96959 = EDGE_CURVE ( 'NONE', #52438, #97248, #82512, .T. ) ;
#96960 = CARTESIAN_POINT ( 'NONE',  ( -15.70679263237263434, -12.88635299011707502, -1.500000000000002220 ) ) ;
#96962 = EDGE_CURVE ( 'NONE', #12764, #96655, #24199, .T. ) ;
#96961 = ORIENTED_EDGE ( 'NONE', *, *, #13587, .F. ) ;
#96963 = CARTESIAN_POINT ( 'NONE',  ( -22.88579126497628025, -1.409509213828211927, -1.500000000000002220 ) ) ;
#96964 = CARTESIAN_POINT ( 'NONE',  ( -32.58671537039989374, -24.34968618360933590, 0.1864209137778856384 ) ) ;
#96965 = EDGE_CURVE ( 'NONE', #26990, #62214, #19209, .T. ) ;
#96966 = ORIENTED_EDGE ( 'NONE', *, *, #36422, .F. ) ;
#96967 = CARTESIAN_POINT ( 'NONE',  ( -109.5228709571500474, -23.48783264082477018, -1.443836473390083253 ) ) ;
#96968 = EDGE_CURVE ( 'NONE', #27856, #40542, #28931, .T. ) ;
#96969 = CARTESIAN_POINT ( 'NONE',  ( -49.66108014839032592, -25.12215372425595206, 6.884432421844342009 ) ) ;
#96970 = B_SPLINE_CURVE_WITH_KNOTS ( 'NONE', 3,
 ( #56879, #33023, #88311, #56379 ),
 .UNSPECIFIED., .F., .F.,
 ( 4, 4 ),
 ( 0.000000000000000000, 9.999999999998897304E-05 ),
 .UNSPECIFIED. ) ;
#96971 = DIRECTION ( 'NONE',  ( -0.000000000000000000, 1.000000000000000000, -0.000000000000000000 ) ) ;
#96972 = CARTESIAN_POINT ( 'NONE',  ( -20.37118330240554087, -5.769015352940915164, 11.49999999999999645 ) ) ;
#96973 = CARTESIAN_POINT ( 'NONE',  ( 4.260453091581613450, -21.75001586557718980, -1.500000000000002220 ) ) ;
#96974 = CARTESIAN_POINT ( 'NONE',  ( 6.154377932377651739, 19.64630176443789367, -1.500000000000002220 ) ) ;
#96975 = ORIENTED_EDGE ( 'NONE', *, *, #6112, .T. ) ;
#96976 = CARTESIAN_POINT ( 'NONE',  ( -41.53956861893506414, -24.34968618360933590, 0.1864209137778857495 ) ) ;
#96977 = ORIENTED_EDGE ( 'NONE', *, *, #36172, .T. ) ;
#96978 = CARTESIAN_POINT ( 'NONE',  ( -126.6228709571500559, -29.50250786944525672, 11.44777988621622633 ) ) ;
#96979 = EDGE_CURVE ( 'NONE', #79051, #43735, #84643, .T. ) ;
#96980 = DIRECTION ( 'NONE',  ( 0.000000000000000000, -2.173523156925980399E-06, 0.9999999999976378895 ) ) ;
#96981 = ORIENTED_EDGE ( 'NONE', *, *, #73318, .T. ) ;
#96982 = ORIENTED_EDGE ( 'NONE', *, *, #20468, .T. ) ;
#96983 = ORIENTED_EDGE ( 'NONE', *, *, #45661, .F. ) ;
#96984 = CARTESIAN_POINT ( 'NONE',  ( -77.52287095715007581, -24.51387760970724727, 9.387446482453412955 ) ) ;
#96986 = DIRECTION ( 'NONE',  ( 0.000000000000000000, 0.9999999999976377785, 2.173523156925979975E-06 ) ) ;
#96985 = B_SPLINE_CURVE_WITH_KNOTS ( 'NONE', 3,
 ( #85629, #47084, #92237, #14613, #54202, #70412, #46577, #77999, #60812, #45584 ),
 .UNSPECIFIED., .F., .F.,
 ( 4, 2, 2, 2, 4 ),
 ( 0.000000000000000000, 0.0004275315936954019597, 0.0008550631873907993657, 0.001282594781086196772, 0.001710126374781594178 ),
 .UNSPECIFIED. ) ;
#96987 = CARTESIAN_POINT ( 'NONE',  ( 14.43441819133144044, -3.316774720514426900, -28.36222020317207182 ) ) ;
#96988 = CARTESIAN_POINT ( 'NONE',  ( -7.357705842588929457, 19.43699106120834230, -1.500000000000002220 ) ) ;
#96989 = CARTESIAN_POINT ( 'NONE',  ( -10.76533847658563126, -18.86179312034942868, 11.49999999999999645 ) ) ;
#96990 = ORIENTED_EDGE ( 'NONE', *, *, #22650, .T. ) ;
#96991 = LINE ( 'NONE', #27490, #96866 ) ;
#96992 = CARTESIAN_POINT ( 'NONE',  ( -96.55620429048337883, -24.65952944569304606, 1.056160979905702790 ) ) ;
#96993 = CARTESIAN_POINT ( 'NONE',  ( -3.561414601982806349, 22.15502443119318343, 11.49999999999998934 ) ) ;
#96994 = CIRCLE ( 'NONE', #32161, 1.836000000000000743 ) ;
#96995 = DIRECTION ( 'NONE',  ( -0.000000000000000000, -0.000000000000000000, -1.000000000000000000 ) ) ;
#96996 = CARTESIAN_POINT ( 'NONE',  ( -102.5228709571501042, -23.96177878511310055, 10.65340807706329507 ) ) ;
#96997 = ORIENTED_EDGE ( 'NONE', *, *, #170, .T. ) ;
#96998 = FACE_OUTER_BOUND ( 'NONE', #99615, .T. ) ;
#96999 = DIRECTION ( 'NONE',  ( -1.000000000000000000, 0.000000000000000000, 0.000000000000000000 ) ) ;
#97000 = ORIENTED_EDGE ( 'NONE', *, *, #94033, .F. ) ;
#97001 = ORIENTED_EDGE ( 'NONE', *, *, #81178, .F. ) ;
#97002 = PLANE ( 'NONE',  #39267 ) ;
#97003 = ORIENTED_EDGE ( 'NONE', *, *, #11961, .F. ) ;
#97004 = CARTESIAN_POINT ( 'NONE',  ( -8.160016139516647726, -19.69179572373923648, -1.500000000000002220 ) ) ;
#97005 = EDGE_LOOP ( 'NONE', ( #81263, #26135, #14501, #58713 ) ) ;
#97006 = CARTESIAN_POINT ( 'NONE',  ( -88.54824115366665183, -24.34968618360933945, 0.1864209137778829184 ) ) ;
#97007 = CARTESIAN_POINT ( 'NONE',  ( 19.92038474643397805, 8.973206291307779026, -1.500000000000002220 ) ) ;
#97008 = DIRECTION ( 'NONE',  ( 0.000000000000000000, -0.9999999999976377785, -2.173523156925979128E-06 ) ) ;
#97009 = CARTESIAN_POINT ( 'NONE',  ( 19.36006514395606004, 11.85157241509795512, 11.49999999999998934 ) ) ;
#97010 = AXIS2_PLACEMENT_3D ( 'NONE', #14448, #74851, #81980 ) ;
#97011 = CARTESIAN_POINT ( 'NONE',  ( -40.45829750704998418, -25.28892422092284420, 3.293942890672450829 ) ) ;
#97012 = B_SPLINE_CURVE_WITH_KNOTS ( 'NONE', 3,
 ( #41057, #47675, #42066, #10098, #64420, #49185 ),
 .UNSPECIFIED., .F., .F.,
 ( 4, 2, 4 ),
 ( -8.872634692045293004E-06, 0.0009000329399760627434, 0.001808938514644170764 ),
 .UNSPECIFIED. ) ;
#97013 = LINE ( 'NONE', #41747, #43307 ) ;
#97014 = CARTESIAN_POINT ( 'NONE',  ( -19.93956527825925917, 9.129326121205059152, -1.500000000000002220 ) ) ;
#97015 = CARTESIAN_POINT ( 'NONE',  ( -66.62287095715005592, -23.48783264082478439, -1.443836473390067487 ) ) ;
#97016 = ORIENTED_EDGE ( 'NONE', *, *, #10912, .F. ) ;
#97017 = CARTESIAN_POINT ( 'NONE',  ( -69.62287095715009855, -24.51283580621364422, 0.6167428607019820319 ) ) ;
#97018 = DIRECTION ( 'NONE',  ( 0.000000000000000000, 0.000000000000000000, 1.000000000000000000 ) ) ;
#97019 = ADVANCED_FACE ( 'NONE', ( #58784 ), #34451, .F. ) ;
#97020 = ORIENTED_EDGE ( 'NONE', *, *, #76772, .F. ) ;
#97021 = CARTESIAN_POINT ( 'NONE',  ( -90.62287095715004170, -23.85196035786901447, -0.8779234886475009159 ) ) ;
#97022 = VERTEX_POINT ( 'NONE', #27333 ) ;
#97023 = CARTESIAN_POINT ( 'NONE',  ( -39.56136241089613037, -25.29384247623274362, 5.536731341526268224 ) ) ;
#97024 = CARTESIAN_POINT ( 'NONE',  ( -30.62052902806165733, -24.26770976782746558, 0.04347934593173557322 ) ) ;
#97025 = CARTESIAN_POINT ( 'NONE',  ( 10.81949470224598997, -18.29866561848832518, -1.500000000000002220 ) ) ;
#97026 = LINE ( 'NONE', #28021, #15807 ) ;
#97027 = CARTESIAN_POINT ( 'NONE',  ( -27.27594984642231069, -24.75185983820420788, 2.337720939227504680 ) ) ;
#97028 = EDGE_CURVE ( 'NONE', #33873, #99331, #89734, .T. ) ;
#97029 = CARTESIAN_POINT ( 'NONE',  ( -80.64675904551151575, -29.50249039766296022, 3.409318347773680369 ) ) ;
#97031 = B_SPLINE_CURVE_WITH_KNOTS ( 'NONE', 3,
 ( #87671, #9540, #17654, #33881 ),
 .UNSPECIFIED., .F., .F.,
 ( 4, 4 ),
 ( 0.01876752652939578034, 0.01976827357016127176 ),
 .UNSPECIFIED. ) ;
#97030 = CARTESIAN_POINT ( 'NONE',  ( 32.50838937279095120, -1.682774720514426114, -10.74666623472941218 ) ) ;
#97032 = AXIS2_PLACEMENT_3D ( 'NONE', #78943, #32279, #8444 ) ;
#97033 = EDGE_CURVE ( 'NONE', #41466, #647, #50674, .T. ) ;
#97034 = LINE ( 'NONE', #13772, #15017 ) ;
#97035 = ORIENTED_EDGE ( 'NONE', *, *, #30695, .F. ) ;
#97036 = CARTESIAN_POINT ( 'NONE',  ( 2.510080532074158377, -19.39449211012750496, 11.49999999999999645 ) ) ;
#97037 = CARTESIAN_POINT ( 'NONE',  ( -95.58953762381672448, -23.48783264082479150, -1.443836473390061936 ) ) ;
#97038 = DIRECTION ( 'NONE',  ( -1.000000000000000000, 0.000000000000000000, 0.000000000000000000 ) ) ;
#97039 = ORIENTED_EDGE ( 'NONE', *, *, #18962, .F. ) ;
#97040 = CARTESIAN_POINT ( 'NONE',  ( -97.52287095715007581, -23.96127896941631974, -0.6493128931037969176 ) ) ;
#97041 = CARTESIAN_POINT ( 'NONE',  ( -101.6008575483875092, -25.12800596871544556, 7.076588377906173122 ) ) ;
#97042 = CARTESIAN_POINT ( 'NONE',  ( -90.52287095715013265, -24.63287334234179582, 0.9662140553045340807 ) ) ;
#97043 = CARTESIAN_POINT ( 'NONE',  ( -45.62287095715004881, -23.47593901973091235, -1.443836447539009749 ) ) ;
#97044 = CARTESIAN_POINT ( 'NONE',  ( -13.08164486973500118, 14.69858247433046650, 11.49999999999998934 ) ) ;
#97045 = ORIENTED_EDGE ( 'NONE', *, *, #1798, .F. ) ;
#97046 = CARTESIAN_POINT ( 'NONE',  ( 33.65278273286722310, -3.366611878523314783, -11.65467467704458393 ) ) ;
#97047 = CARTESIAN_POINT ( 'NONE',  ( 2.935461252226840401, -5.876774720514419847, 20.47627681611744777 ) ) ;
#97048 = DATE_TIME_ROLE ( 'creation_date' ) ;
#97049 = ORIENTED_EDGE ( 'NONE', *, *, #42705, .T. ) ;
#97050 = CARTESIAN_POINT ( 'NONE',  ( 8.271845302688323187, -0.3854532800250802249, 3.722136940144805450 ) ) ;
#97051 = CARTESIAN_POINT ( 'NONE',  ( 0.000000000000000000, 0.000000000000000000, 0.000000000000000000 ) ) ;
#97052 = DIRECTION ( 'NONE',  ( -3.773278334444166432E-23, 1.000000000000000000, 0.000000000000000000 ) ) ;
#97053 = CARTESIAN_POINT ( 'NONE',  ( -118.6241822143420563, -24.51314013834317151, 0.6176544820404233915 ) ) ;
#97054 = CARTESIAN_POINT ( 'NONE',  ( -119.5228709571500474, -23.47593901973090524, -1.443836447538996204 ) ) ;
#97055 = CIRCLE ( 'NONE', #53313, 10.80000000000000782 ) ;
#97056 = AXIS2_PLACEMENT_3D ( 'NONE', #81374, #5243, #75735 ) ;
#97057 = LINE ( 'NONE', #26558, #21396 ) ;
#97058 = CARTESIAN_POINT ( 'NONE',  ( -6.914873625533457968, 6.376774720514426953, 29.95171384920748281 ) ) ;
#97059 = CARTESIAN_POINT ( 'NONE',  ( -7.409219584043468920, -18.53548363135739052, -1.500000000000002220 ) ) ;
#97060 = CARTESIAN_POINT ( 'NONE',  ( -0.04830472105987098502, -22.42465742606800561, 8.862518828116197511 ) ) ;
#97061 = CARTESIAN_POINT ( 'NONE',  ( -5.841000908416043913, -19.03464889989004050, -1.500000000000002220 ) ) ;
#97062 = ORIENTED_EDGE ( 'NONE', *, *, #59294, .F. ) ;
#97063 = AXIS2_PLACEMENT_3D ( 'NONE', #47903, #56024, #79835 ) ;
#97064 = CARTESIAN_POINT ( 'NONE',  ( 15.97264540888995299, -3.316774720514426456, -27.93485543958162154 ) ) ;
#97065 = CARTESIAN_POINT ( 'NONE',  ( 3.902919446070569176, -5.876774720514426953, 21.47497695444087284 ) ) ;
#97066 = B_SPLINE_CURVE_WITH_KNOTS ( 'NONE', 3,
 ( #2953, #43008, #19152, #12538 ),
 .UNSPECIFIED., .F., .F.,
 ( 4, 4 ),
 ( 1.387778780781445676E-17, 0.0001000000000000028508 ),
 .UNSPECIFIED. ) ;
#97067 = EDGE_CURVE ( 'NONE', #72334, #5126, #45288, .T. ) ;
#97068 = CARTESIAN_POINT ( 'NONE',  ( 7.460719433876314532, -6.376774720514426953, -25.14146935902945046 ) ) ;
#97069 = CARTESIAN_POINT ( 'NONE',  ( -127.4728709571500360, -25.30558663486607429, 5.000950657679038791 ) ) ;
#97070 = CARTESIAN_POINT ( 'NONE',  ( -7.603582339867426043, -6.376774720514417183, 19.86545874326176175 ) ) ;
#97071 = DIRECTION ( 'NONE',  ( -0.000000000000000000, 1.000000000000000000, -0.000000000000000000 ) ) ;
#97072 = VERTEX_POINT ( 'NONE', #43561 ) ;
#97073 = CARTESIAN_POINT ( 'NONE',  ( -62.62287095715002039, -24.33832256526968507, 0.1851278514119872598 ) ) ;
#97074 = DIRECTION ( 'NONE',  ( 0.000000000000000000, -0.9999999999976377785, -2.173523156925979975E-06 ) ) ;
#97075 = ORIENTED_EDGE ( 'NONE', *, *, #78568, .T. ) ;
#97076 = EDGE_CURVE ( 'NONE', #41986, #59549, #74988, .T. ) ;
#97077 = VECTOR ( 'NONE', #16094, 1000.000000000000000 ) ;
#97078 =( BOUNDED_SURFACE ( )  B_SPLINE_SURFACE ( 3, 1, ( 
 ( #69491, #52768 ),
 ( #91320, #7084 ),
 ( #91815, #61889 ),
 ( #22290, #38035 ) ),
 .UNSPECIFIED., .F., .F., .T. ) 
 B_SPLINE_SURFACE_WITH_KNOTS ( ( 4, 4 ),
 ( 2, 2 ),
 ( 0.000000000000000000, 1.000000000000000000 ),
 ( 0.000000000000000000, 1.000000000000000000 ),
 .UNSPECIFIED. ) 
 GEOMETRIC_REPRESENTATION_ITEM ( )  RATIONAL_B_SPLINE_SURFACE ( (
 ( 1.000000000000000000, 1.000000000000000000),
 ( 0.3333333333333332038, 0.3333333333333332038),
 ( 0.3333333333333332038, 0.3333333333333332038),
 ( 1.000000000000000000, 1.000000000000000000) ) ) 
 REPRESENTATION_ITEM ( '' )  SURFACE ( )  );
#97079 = CARTESIAN_POINT ( 'NONE',  ( 13.55758662847591900, -15.04642845256218031, 11.49999999999998934 ) ) ;
#97080 = CARTESIAN_POINT ( 'NONE',  ( -105.6228709571500417, -24.99156045073393173, 7.747789690856161648 ) ) ;
#97081 = CARTESIAN_POINT ( 'NONE',  ( 9.843544857143434967, 5.965225279485572685, -27.49819965379373343 ) ) ;
#97082 = EDGE_CURVE ( 'NONE', #57950, #90963, #26424, .T. ) ;
#97083 = DIRECTION ( 'NONE',  ( 7.994117400814786717E-16, 0.000000000000000000, -1.000000000000000000 ) ) ;
#97084 = EDGE_CURVE ( 'NONE', #64064, #82023, #35584, .T. ) ;
#97085 = ORIENTED_EDGE ( 'NONE', *, *, #74532, .T. ) ;
#97086 = CARTESIAN_POINT ( 'NONE',  ( -79.20638848209495109, -25.31561901975329576, 5.078358969147119595 ) ) ;
#97087 = CARTESIAN_POINT ( 'NONE',  ( -1.733151984336291695, -6.376774720514408301, 19.29154511076646017 ) ) ;
#97088 = CARTESIAN_POINT ( 'NONE',  ( -18.95788008782500356, -6.583919088883305015, -1.500000000000002220 ) ) ;
#97089 = EDGE_CURVE ( 'NONE', #14852, #69140, #14591, .T. ) ;
#97090 = CARTESIAN_POINT ( 'NONE',  ( -20.98013922110768448, -1.350454208470041273, 11.49999999999999645 ) ) ;
#97091 = CARTESIAN_POINT ( 'NONE',  ( 30.55775998287478856, 1.765878758506263635, 24.49934028559108157 ) ) ;
#97092 = CARTESIAN_POINT ( 'NONE',  ( -70.52205924875542564, -23.48786465467241058, 11.44779295918254824 ) ) ;
#97093 = CARTESIAN_POINT ( 'NONE',  ( -21.77411086464670831, -3.637377321037103872, 11.49999999999998934 ) ) ;
#97094 = ADVANCED_FACE ( 'NONE', ( #78850 ), #14088, .F. ) ;
#97095 = CARTESIAN_POINT ( 'NONE',  ( -42.58953762381672448, -24.64898659630367561, 1.056161002820381833 ) ) ;
#97096 = AXIS2_PLACEMENT_3D ( 'NONE', #22644, #21649, #90680 ) ;
#97097 = CARTESIAN_POINT ( 'NONE',  ( -59.55620429048337883, -24.64898659630528854, 1.056161002820822814 ) ) ;
#97098 = CARTESIAN_POINT ( 'NONE',  ( -50.36897396760109302, -25.27344759737253099, 3.294677657877965071 ) ) ;
#97099 = ORIENTED_EDGE ( 'NONE', *, *, #17957, .T. ) ;
#97100 = LINE ( 'NONE', #80880, #51114 ) ;
#97101 = B_SPLINE_SURFACE_WITH_KNOTS ( 'NONE', 3, 3, ( 
 ( #67579, #5660, #89407, #68565 ),
 ( #28498, #27517, #50854, #83777 ),
 ( #14259, #52346, #81793, #28008 ),
 ( #12266, #51850, #43245, #74183 ),
 ( #35627, #58966, #91390, #20374 ),
 ( #75657, #82289, #28998, #52842 ),
 ( #68073, #45235, #12765, #76158 ) ),
 .UNSPECIFIED., .F., .F., .F.,
 ( 4, 3, 4 ),
 ( 4, 4 ),
 ( 0.7945040050992236980, 0.8970133687736494554, 0.9995227324480753239 ),
 ( 0.07951420290697416848, 0.08056363649449890807 ),
 .UNSPECIFIED. ) ;
#97102 = CARTESIAN_POINT ( 'NONE',  ( -72.52287095715007581, -23.47596703998600631, 11.44779298504228748 ) ) ;
#97103 = EDGE_LOOP ( 'NONE', ( #92878, #8246, #98692, #95231 ) ) ;
#97104 = ORIENTED_EDGE ( 'NONE', *, *, #20468, .F. ) ;
#97105 = CARTESIAN_POINT ( 'NONE',  ( -55.52287095715004028, -24.92579138211018730, 1.929029949965661128 ) ) ;
#97106 = DIRECTION ( 'NONE',  ( -1.000000000000000000, 0.000000000000000000, 0.000000000000000000 ) ) ;
#97108 = EDGE_CURVE ( 'NONE', #69394, #21092, #45819, .T. ) ;
#97107 = CARTESIAN_POINT ( 'NONE',  ( -76.51686571011160254, -23.73766607897670866, -1.055555164236452681 ) ) ;
#97109 = CARTESIAN_POINT ( 'NONE',  ( 16.39479758508079144, -12.47777281027006424, -1.500000000000002220 ) ) ;
#97110 = CARTESIAN_POINT ( 'NONE',  ( 21.55061338234859392, -0.003183148592148328428, 11.49999999999999645 ) ) ;
#97111 = VERTEX_POINT ( 'NONE', #60793 ) ;
#97112 = DIRECTION ( 'NONE',  ( 0.000000000000000000, 0.000000000000000000, -1.000000000000000000 ) ) ;
#97113 = CARTESIAN_POINT ( 'NONE',  ( -116.5228709571499905, -23.48783264083416711, -1.443836473375476270 ) ) ;
#97114 = CARTESIAN_POINT ( 'NONE',  ( -60.62287095715004881, -23.47593901973091235, -1.443836447539007972 ) ) ;
#97115 = CARTESIAN_POINT ( 'NONE',  ( 12.52526618502215250, 18.50471055633022388, -1.500000000000002220 ) ) ;
#97116 = CARTESIAN_POINT ( 'NONE',  ( 29.73612274945269718, -5.099749465620300626, 27.18845636319765191 ) ) ;
#97117 = CARTESIAN_POINT ( 'NONE',  ( -31.55620429048338593, -23.48783264082477729, -1.443836473390074149 ) ) ;
#97118 = ORIENTED_EDGE ( 'NONE', *, *, #41493, .F. ) ;
#97119 = DIRECTION ( 'NONE',  ( -0.6599726524652346216, 0.000000000000000000, 0.7512896232465895441 ) ) ;
#97120 = DIRECTION ( 'NONE',  ( 0.000000000000000000, 0.000000000000000000, 1.000000000000000000 ) ) ;
#97121 = CARTESIAN_POINT ( 'NONE',  ( 7.204507412156021751, -19.57454612608841771, -1.500000000000002220 ) ) ;
#97122 = ORIENTED_EDGE ( 'NONE', *, *, #58853, .F. ) ;
#97124 = ORIENTED_EDGE ( 'NONE', *, *, #41302, .T. ) ;
#97123 = DIRECTION ( 'NONE',  ( -0.000000000000000000, 1.000000000000000000, -0.000000000000000000 ) ) ;
#97125 = ORIENTED_EDGE ( 'NONE', *, *, #37768, .T. ) ;
#97126 = CARTESIAN_POINT ( 'NONE',  ( -51.15183413599653761, -25.29055395653329796, 4.391135634342788308 ) ) ;
#97127 = CARTESIAN_POINT ( 'NONE',  ( -20.79277273739468512, 3.736189789763188607, -1.500000000000002220 ) ) ;
#97128 = ORIENTED_EDGE ( 'NONE', *, *, #9557, .T. ) ;
#97129 = CARTESIAN_POINT ( 'NONE',  ( -20.27875734969026311, 7.743225279485574042, 26.25402280011862288 ) ) ;
#97130 = PLANE ( 'NONE',  #7721 ) ;
#97131 = CARTESIAN_POINT ( 'NONE',  ( -45.52287095715007581, -25.00182538069144655, 7.747789668545101094 ) ) ;
#97132 = CIRCLE ( 'NONE', #11226, 0.3000000000000016542 ) ;
#97133 = DIRECTION ( 'NONE',  ( -3.773278334453079030E-23, 0.9999999999976377785, 2.173523156925979128E-06 ) ) ;
#97134 = CARTESIAN_POINT ( 'NONE',  ( -50.30144419495010766, -25.11080889048738030, 2.835020071207171810 ) ) ;
#97135 = CARTESIAN_POINT ( 'NONE',  ( -21.58526226860004371, 1.989002153404973328, -1.500000000000002220 ) ) ;
#97136 = CARTESIAN_POINT ( 'NONE',  ( -63.52287095715006160, -24.66019654487199375, 8.947790411086122830 ) ) ;
#97138 = ORIENTED_EDGE ( 'NONE', *, *, #86156, .T. ) ;
#97137 = CARTESIAN_POINT ( 'NONE',  ( -22.23078454666273274, -1.437644496696519170, 11.49999999999999645 ) ) ;
#97139 = CARTESIAN_POINT ( 'NONE',  ( 0.1011420733776826480, 1.446399035885977069, -9.000000000000000000 ) ) ;
#97140 = CARTESIAN_POINT ( 'NONE',  ( 15.00349588318476712, 3.443263483566387784, -27.42854228801664007 ) ) ;
#97141 = EDGE_CURVE ( 'NONE', #71376, #27395, #54286, .T. ) ;
#97142 = DIRECTION ( 'NONE',  ( -0.000000000000000000, 1.000000000000000000, -0.000000000000000000 ) ) ;
#97143 = EDGE_LOOP ( 'NONE', ( #83934, #63185, #47702, #5129 ) ) ;
#97144 = VECTOR ( 'NONE', #41611, 1000.000000000000227 ) ;
#97146 = ORIENTED_EDGE ( 'NONE', *, *, #40427, .T. ) ;
#97145 = CARTESIAN_POINT ( 'NONE',  ( -112.5228709571500616, -29.50250243563736774, 8.947779886222136270 ) ) ;
#97147 = EDGE_CURVE ( 'NONE', #10305, #32699, #58340, .T. ) ;
#97148 = VECTOR ( 'NONE', #29440, 1000.000000000000114 ) ;
#97149 = ORIENTED_EDGE ( 'NONE', *, *, #98216, .F. ) ;
#97150 = VECTOR ( 'NONE', #1115, 1000.000000000000114 ) ;
#97151 = CARTESIAN_POINT ( 'NONE',  ( -100.9064891590902420, -25.14618869607998164, 7.025821505394578281 ) ) ;
#97152 = LINE ( 'NONE', #9036, #46535 ) ;
#97153 = CARTESIAN_POINT ( 'NONE',  ( -49.13281699349433040, -25.29228295451561337, 4.248284216210590714 ) ) ;
#97154 = CIRCLE ( 'NONE', #1550, 3.349999999999998757 ) ;
#97155 = CARTESIAN_POINT ( 'NONE',  ( 22.81105451610979173, -1.475225279485572916, -17.31691820600746823 ) ) ;
#97156 = ADVANCED_FACE ( 'NONE', ( #84108 ), #85980, .F. ) ;
#97157 = LINE ( 'NONE', #11916, #27995 ) ;
#97158 = ORIENTED_EDGE ( 'NONE', *, *, #58902, .F. ) ;
#97159 = CARTESIAN_POINT ( 'NONE',  ( -16.26263985875334228, -10.51264992557365829, 11.49999999999999645 ) ) ;
#97160 = CARTESIAN_POINT ( 'NONE',  ( -81.52287095715006160, -23.47596703998600631, 11.44779298504228571 ) ) ;
#97161 = CARTESIAN_POINT ( 'NONE',  ( 11.36419782745769069, 19.35538867594532775, -1.500000000000002220 ) ) ;
#97162 = EDGE_CURVE ( 'NONE', #58574, #41451, #77242, .T. ) ;
#97163 = VERTEX_POINT ( 'NONE', #24570 ) ;
#97164 = CARTESIAN_POINT ( 'NONE',  ( -101.5471428905241140, -24.66019654487200086, 8.947790411086115725 ) ) ;
#97165 = CARTESIAN_POINT ( 'NONE',  ( 5.109298100551870725, 3.316774720514426456, -27.55941679637892250 ) ) ;
#97166 = PLANE ( 'NONE',  #9256 ) ;
#97167 = CARTESIAN_POINT ( 'NONE',  ( -97.23961502710135107, -25.30558673197061381, 5.002395802403323266 ) ) ;
#97168 = CARTESIAN_POINT ( 'NONE',  ( 9.507684299284662188, -17.14340340408069707, 11.49999999999998934 ) ) ;
#97169 = CARTESIAN_POINT ( 'NONE',  ( -119.6228709571500559, -23.47596703998600631, 11.44779298504227860 ) ) ;
#97170 = ORIENTED_EDGE ( 'NONE', *, *, #38420, .T. ) ;
#97171 = CARTESIAN_POINT ( 'NONE',  ( -7.320277434469578459, 20.25297033093062282, -1.500000000000002220 ) ) ;
#97172 = CARTESIAN_POINT ( 'NONE',  ( -2.704906987277317931, -6.376774720514425177, -28.92935364444904778 ) ) ;
#97173 = CARTESIAN_POINT ( 'NONE',  ( 18.72495633783376334, 0.000000000000000000, -1.691563534834430227 ) ) ;
#97174 = DIRECTION ( 'NONE',  ( 0.000000000000000000, -2.173523156925980399E-06, 0.9999999999976378895 ) ) ;
#97175 = DIRECTION ( 'NONE',  ( -1.000000000000000000, 0.000000000000000000, -0.000000000000000000 ) ) ;
#97176 = CARTESIAN_POINT ( 'NONE',  ( 20.04565040668967413, 11.27863464804978477, -1.500000000000002220 ) ) ;
#97177 = CC_DESIGN_DATE_AND_TIME_ASSIGNMENT ( #9815, #88447, ( #65234 ) ) ;
#97178 = PERSON_AND_ORGANIZATION_ROLE ( 'design_owner' ) ;
#97179 = FACE_OUTER_BOUND ( 'NONE', #8153, .T. ) ;
#97180 = CARTESIAN_POINT ( 'NONE',  ( -53.62804967469141104, -24.51314013834315730, 0.6176544820404108460 ) ) ;
#97181 = CARTESIAN_POINT ( 'NONE',  ( -19.29710791919172053, 5.528754708966634901, 11.49999999999999645 ) ) ;
#97182 = CARTESIAN_POINT ( 'NONE',  ( -109.5317876555421037, -25.10927444747738235, 3.055434969720114413 ) ) ;
#97183 = CARTESIAN_POINT ( 'NONE',  ( -31.52287095715007581, -24.51283580621452174, 0.6167428607045826183 ) ) ;
#97184 = CARTESIAN_POINT ( 'NONE',  ( 5.184553252003285984, -6.475225279485573360, -28.06387035751381731 ) ) ;
#97185 = CARTESIAN_POINT ( 'NONE',  ( 11.86515846156731335, 5.152774720514426754, -28.09350142571734921 ) ) ;
#97186 = CARTESIAN_POINT ( 'NONE',  ( 14.61581676223891613, 2.682774720514426559, -27.35847991879931485 ) ) ;
#97187 = CARTESIAN_POINT ( 'NONE',  ( -16.51628311069853083, -11.03946451426814690, 11.49999999999998934 ) ) ;
#97188 = CARTESIAN_POINT ( 'NONE',  ( -113.6255566680633535, -24.34968618360934300, 0.1864209137778879699 ) ) ;
#97189 = CARTESIAN_POINT ( 'NONE',  ( 17.66836560233463516, 8.693963128369697202, -1.500000000000002220 ) ) ;
#97190 = CARTESIAN_POINT ( 'NONE',  ( -126.5206417414244982, -24.51419770103158058, 9.386484678747164523 ) ) ;
#97191 = CARTESIAN_POINT ( 'NONE',  ( -110.5228709571500190, -24.62285846331434769, 9.038163153548369522 ) ) ;
#97192 = CARTESIAN_POINT ( 'NONE',  ( 31.41423154468143153, 2.682774720514426559, -0.3119954678742140053 ) ) ;
#97193 = CARTESIAN_POINT ( 'NONE',  ( 14.30100545221680441, -14.83292283143518375, 11.49999999999999645 ) ) ;
#97194 = VECTOR ( 'NONE', #50483, 1000.000000000000000 ) ;
#97195 = DIRECTION ( 'NONE',  ( 0.000000000000000000, -1.000000000000000000, 0.000000000000000000 ) ) ;
#97196 = CARTESIAN_POINT ( 'NONE',  ( -7.311831771877058905, -21.45741656709679646, 11.49999999999999645 ) ) ;
#97197 = ORIENTED_EDGE ( 'NONE', *, *, #72628, .F. ) ;
#97198 = CARTESIAN_POINT ( 'NONE',  ( -1.877194073982709988, 8.794404527355018431, -9.000000000000000000 ) ) ;
#97199 = CARTESIAN_POINT ( 'NONE',  ( 29.71119274252842501, 4.341971045292455145, 27.93347042254709223 ) ) ;
#97200 = VECTOR ( 'NONE', #88001, 1000.000000000000000 ) ;
#97201 = EDGE_CURVE ( 'NONE', #10079, #63968, #93577, .T. ) ;
#97202 = CARTESIAN_POINT ( 'NONE',  ( -101.5228709571500758, -29.50250243563736774, 8.947779886222138046 ) ) ;
#97203 = CARTESIAN_POINT ( 'NONE',  ( -56.52287095715004028, -23.73934037231755667, 11.05740245334328797 ) ) ;
#97204 = AXIS2_PLACEMENT_3D ( 'NONE', #96381, #20243, #26872 ) ;
#97205 = ORIENTED_EDGE ( 'NONE', *, *, #50882, .F. ) ;
#97206 = EDGE_LOOP ( 'NONE', ( #49268, #90137, #98454, #12097 ) ) ;
#97207 = DIRECTION ( 'NONE',  ( 0.000000000000000000, 1.000000000000000000, 0.000000000000000000 ) ) ;
#97208 = CARTESIAN_POINT ( 'NONE',  ( 10.78062712001149492, -20.16176685268226976, 11.49999999999998934 ) ) ;
#97209 = CARTESIAN_POINT ( 'NONE',  ( 29.77147767949874435, -6.376774720514426953, 26.15915692125051706 ) ) ;
#97210 = AXIS2_PLACEMENT_3D ( 'NONE', #59049, #49950, #26598 ) ;
#97211 = CARTESIAN_POINT ( 'NONE',  ( 21.54666897473465070, 1.519730039111064412, -1.500000000000002220 ) ) ;
#97212 = CARTESIAN_POINT ( 'NONE',  ( -94.62287095715005592, -29.50250786944525672, 11.44777988621623344 ) ) ;
#97213 = CARTESIAN_POINT ( 'NONE',  ( -3.826923076923074429, -5.876774720514426953, 21.75000000000000355 ) ) ;
#97214 = ADVANCED_FACE ( 'NONE', ( #90729 ), #67907, .T. ) ;
#97215 = CARTESIAN_POINT ( 'NONE',  ( 11.64696156460271581, 19.30390316350253244, 11.49999999999999645 ) ) ;
#97216 = ORIENTED_EDGE ( 'NONE', *, *, #81869, .T. ) ;
#97217 = VECTOR ( 'NONE', #99043, 1000.000000000000000 ) ;
#97218 = CARTESIAN_POINT ( 'NONE',  ( -69.75794024142732042, -25.31612440964994803, 4.946031520551585459 ) ) ;
#97219 = CARTESIAN_POINT ( 'NONE',  ( -9.458160343781703006, 19.84743614482962926, -1.500000000000002220 ) ) ;
#97220 = EDGE_CURVE ( 'NONE', #19742, #6577, #9527, .T. ) ;
#97221 = B_SPLINE_CURVE_WITH_KNOTS ( 'NONE', 3,
 ( #77281, #22988, #77776, #6290 ),
 .UNSPECIFIED., .F., .F.,
 ( 4, 4 ),
 ( 0.000000000000000000, 9.999999999997510880E-05 ),
 .UNSPECIFIED. ) ;
#97223 = CARTESIAN_POINT ( 'NONE',  ( -111.6245987100719361, -24.51314013834316796, 0.6176544820404210601 ) ) ;
#97222 = VECTOR ( 'NONE', #28639, 1000.000000000000000 ) ;
#97224 = CARTESIAN_POINT ( 'NONE',  ( -29.24636659181000198, -24.79699738154659983, 4.940287927001176804 ) ) ;
#97225 = ORIENTED_EDGE ( 'NONE', *, *, #42153, .T. ) ;
#97226 = DIRECTION ( 'NONE',  ( -0.06283980576413537855, 0.000000000000000000, -0.9980236263794188822 ) ) ;
#97227 = CARTESIAN_POINT ( 'NONE',  ( -35.62287095715005592, -29.50250786944525672, 11.44777988621624232 ) ) ;
#97228 = VERTEX_POINT ( 'NONE', #39803 ) ;
#97229 = CARTESIAN_POINT ( 'NONE',  ( -84.62287095715005592, -23.72747288104441665, -1.053458166803661111 ) ) ;
#97230 = ORIENTED_EDGE ( 'NONE', *, *, #17584, .F. ) ;
#97231 = ORIENTED_EDGE ( 'NONE', *, *, #27341, .T. ) ;
#97232 = ORIENTED_EDGE ( 'NONE', *, *, #82634, .F. ) ;
#97233 = CARTESIAN_POINT ( 'NONE',  ( -111.2228709571500644, -23.47596703998600631, 11.44779298504227860 ) ) ;
#97234 = DIRECTION ( 'NONE',  ( 0.000000000000000000, 1.000000000000000000, 0.000000000000000000 ) ) ;
#97236 = EDGE_CURVE ( 'NONE', #67798, #28943, #36121, .T. ) ;
#97235 = CARTESIAN_POINT ( 'NONE',  ( 14.53567905697410367, 3.934666312338140237, -28.27917189340610449 ) ) ;
#97237 = CARTESIAN_POINT ( 'NONE',  ( -3.558151220431595707, 20.12126150705307381, -1.500000000000002220 ) ) ;
#97238 = ORIENTED_EDGE ( 'NONE', *, *, #40624, .T. ) ;
#97239 = CARTESIAN_POINT ( 'NONE',  ( -71.53176178743996161, -25.15936612061949162, 6.883890870244061766 ) ) ;
#97240 = CARTESIAN_POINT ( 'NONE',  ( -29.55258301704943946, -23.87856313377009698, 10.65365256123546978 ) ) ;
#97241 = CARTESIAN_POINT ( 'NONE',  ( -105.5573405443120407, -23.85016227208580730, -0.8807180028928328630 ) ) ;
#97242 = LINE ( 'NONE', #57695, #93376 ) ;
#97243 = ORIENTED_EDGE ( 'NONE', *, *, #85339, .T. ) ;
#97244 = DIRECTION ( 'NONE',  ( 0.000000000000000000, -1.000000000000000000, 0.000000000000000000 ) ) ;
#97245 = CARTESIAN_POINT ( 'NONE',  ( -103.6228709571500559, -24.66019654487199375, 8.947790411086124607 ) ) ;
#97246 = ORIENTED_EDGE ( 'NONE', *, *, #48098, .F. ) ;
#97247 = CARTESIAN_POINT ( 'NONE',  ( -5.109682455881146446, -20.12422286529520932, -1.500000000000002220 ) ) ;
#97248 = VERTEX_POINT ( 'NONE', #10354 ) ;
#97250 = ORIENTED_EDGE ( 'NONE', *, *, #22863, .F. ) ;
#97249 = CARTESIAN_POINT ( 'NONE',  ( -71.52287095715007581, -29.50248528299804818, 1.056150453629036701 ) ) ;
#97251 = CARTESIAN_POINT ( 'NONE',  ( 30.13760268648183782, -5.267913728810161622, 19.84760796525321425 ) ) ;
#97252 = CARTESIAN_POINT ( 'NONE',  ( -107.6228709571500985, -24.33832256526968862, 0.1851278514119934215 ) ) ;
#97253 = ORIENTED_EDGE ( 'NONE', *, *, #21034, .F. ) ;
#97254 = ORIENTED_EDGE ( 'NONE', *, *, #86035, .T. ) ;
#97255 = DIRECTION ( 'NONE',  ( 1.000000000000000000, 0.000000000000000000, -0.000000000000000000 ) ) ;
#97256 = CARTESIAN_POINT ( 'NONE',  ( -68.62287095715004170, -23.96177878511307568, 10.65340807706330217 ) ) ;
#97257 = CARTESIAN_POINT ( 'NONE',  ( -27.96875734969026084, 6.143225279485573509, 0.7300228001186309656 ) ) ;
#97259 = EDGE_CURVE ( 'NONE', #18022, #8339, #64677, .T. ) ;
#97258 = CARTESIAN_POINT ( 'NONE',  ( -43.58703515042599719, -24.35071581493542325, 9.817618358456034144 ) ) ;
#97261 = VERTEX_POINT ( 'NONE', #9852 ) ;
#97260 = CARTESIAN_POINT ( 'NONE',  ( 16.06085343747454175, -15.19291221174989204, 11.49999999999999645 ) ) ;
#97262 = CARTESIAN_POINT ( 'NONE',  ( -63.62287095715004881, -29.50248528299804818, 1.056150453629034924 ) ) ;
#97263 = CARTESIAN_POINT ( 'NONE',  ( -2.075279548881721947, -22.52154899835045043, -1.500000000000002220 ) ) ;
#97264 = B_SPLINE_CURVE_WITH_KNOTS ( 'NONE', 3,
 ( #84865, #100065, #23445, #44824 ),
 .UNSPECIFIED., .F., .F.,
 ( 4, 4 ),
 ( 0.000000000000000000, 1.000000000000000000 ),
 .UNSPECIFIED. ) ;
#97265 = B_SPLINE_CURVE_WITH_KNOTS ( 'NONE', 3,
 ( #14058, #92186, #52141, #83066 ),
 .UNSPECIFIED., .F., .F.,
 ( 4, 4 ),
 ( 0.06054323244033155138, 0.06954966371244711287 ),
 .UNSPECIFIED. ) ;
#97267 = ORIENTED_EDGE ( 'NONE', *, *, #76942, .F. ) ;
#97266 = CARTESIAN_POINT ( 'NONE',  ( -99.46410954829916307, -25.30559305872911935, 5.025828599125619967 ) ) ;
#97268 = ADVANCED_FACE ( 'NONE', ( #17466 ), #41825, .T. ) ;
#97269 = ORIENTED_EDGE ( 'NONE', *, *, #15863, .F. ) ;
#97270 = CARTESIAN_POINT ( 'NONE',  ( -75.62287095715005592, -23.48786465467241058, 11.44779295918254647 ) ) ;
#97271 = AXIS2_PLACEMENT_3D ( 'NONE', #2653, #34597, #96986 ) ;
#97272 = EDGE_CURVE ( 'NONE', #4626, #61654, #55072, .T. ) ;
#97273 = EDGE_CURVE ( 'NONE', #11836, #99971, #51807, .T. ) ;
#97274 = CARTESIAN_POINT ( 'NONE',  ( -57.50859435744194315, -23.96169478059713143, 10.65365249895718058 ) ) ;
#97275 = ORIENTED_EDGE ( 'NONE', *, *, #28936, .F. ) ;
#97276 = CARTESIAN_POINT ( 'NONE',  ( -16.93204426113827310, 12.72334981527875186, 11.49999999999998934 ) ) ;
#97277 = CARTESIAN_POINT ( 'NONE',  ( 32.66876533700882845, 5.965225279485572685, -12.58926540598385557 ) ) ;
#97278 = CARTESIAN_POINT ( 'NONE',  ( -40.93037633462841995, -25.29610591104019690, 5.483614025508329881 ) ) ;
#97279 = CARTESIAN_POINT ( 'NONE',  ( 16.98343680692684643, -14.46476453587665389, -1.500000000000002220 ) ) ;
#97280 = DIRECTION ( 'NONE',  ( 1.000000000000000000, 0.000000000000000000, 0.000000000000000000 ) ) ;
#97281 = ORIENTED_EDGE ( 'NONE', *, *, #62519, .T. ) ;
#97282 = CARTESIAN_POINT ( 'NONE',  ( -65.92287095715009571, -23.47593901973090524, -1.443836447538997980 ) ) ;
#97283 = CARTESIAN_POINT ( 'NONE',  ( -37.57568117332552760, -24.65952944569304606, 1.056160979905695907 ) ) ;
#97284 = CARTESIAN_POINT ( 'NONE',  ( -49.62287095715004881, -23.72773821059535493, 11.05748984161097503 ) ) ;
#97285 = DIRECTION ( 'NONE',  ( -0.000000000000000000, -1.000000000000000000, -0.000000000000000000 ) ) ;
#97286 = VECTOR ( 'NONE', #92490, 1000.000000000000000 ) ;
#97287 = CARTESIAN_POINT ( 'NONE',  ( -10.28394983263804185, -16.58134856480417341, -1.500000000000002220 ) ) ;
#97288 = AXIS2_PLACEMENT_3D ( 'NONE', #98193, #58652, #81493 ) ;
#97289 = CARTESIAN_POINT ( 'NONE',  ( 19.78805588120126302, 8.271231038663975355, -1.500000000000002220 ) ) ;
#97290 = DIRECTION ( 'NONE',  ( 1.000000000000000000, -0.000000000000000000, 0.000000000000000000 ) ) ;
#97291 = CARTESIAN_POINT ( 'NONE',  ( 6.660000000000001030, 2.939152317953647106E-16, -2.399999999999999911 ) ) ;
#97292 = CARTESIAN_POINT ( 'NONE',  ( -88.62287095715004170, -24.64965695001469115, 8.947790433994180503 ) ) ;
#97293 = CARTESIAN_POINT ( 'NONE',  ( 15.15630024635751383, 17.02982414992789018, -1.500000000000002220 ) ) ;
#97294 = EDGE_CURVE ( 'NONE', #37802, #65316, #96682, .T. ) ;
#97295 = ADVANCED_FACE ( 'NONE', ( #65671, #57052 ), #88489, .T. ) ;
#97296 = AXIS2_PLACEMENT_3D ( 'NONE', #41642, #40129, #1068 ) ;
#97297 = DATE_TIME_ROLE ( 'classification_date' ) ;
#97298 = AXIS2_PLACEMENT_3D ( 'NONE', #67399, #75480, #91708 ) ;
#97299 = CARTESIAN_POINT ( 'NONE',  ( -116.5228709571500616, -29.50250786944525672, 11.44777988621622811 ) ) ;
#97300 = CARTESIAN_POINT ( 'NONE',  ( -101.5562042904833930, -24.66019654487199730, 8.947790411086124607 ) ) ;
#97301 = CARTESIAN_POINT ( 'NONE',  ( 14.69432462292611952, 13.40460087117274490, 11.49999999999999645 ) ) ;
#97302 = LINE ( 'NONE', #4952, #4948 ) ;
#97303 = CARTESIAN_POINT ( 'NONE',  ( -39.51315756755419528, -23.73791477778911130, 11.05961554403170943 ) ) ;
#97304 = CARTESIAN_POINT ( 'NONE',  ( -101.6228709571500417, -23.72747288104441665, -1.053458166803661333 ) ) ;
#97305 = ORIENTED_EDGE ( 'NONE', *, *, #2634, .T. ) ;
#97306 = CARTESIAN_POINT ( 'NONE',  ( 30.09341516180546350, 1.477225279485574028, -13.89311774897855933 ) ) ;
#97307 = CARTESIAN_POINT ( 'NONE',  ( -62.62287095715010565, -23.95044443724992078, 10.65354141964650125 ) ) ;
#97308 = CARTESIAN_POINT ( 'NONE',  ( 3.708801897538985148, -21.39311272803122321, 11.49999999999998934 ) ) ;
#97309 = EDGE_CURVE ( 'NONE', #80639, #50453, #81368, .T. ) ;
#97310 = CARTESIAN_POINT ( 'NONE',  ( 32.73857899460460175, 6.475225279485576024, -13.20677013500359820 ) ) ;
#97311 = CARTESIAN_POINT ( 'NONE',  ( 11.58774116221665729, 15.72987433093905096, -1.500000000000002220 ) ) ;
#97312 = EDGE_CURVE ( 'NONE', #96476, #79708, #64011, .T. ) ;
#97313 = DIRECTION ( 'NONE',  ( -1.000000000000000000, 0.000000000000000000, -0.000000000000000000 ) ) ;
#97314 = ORIENTED_EDGE ( 'NONE', *, *, #4601, .T. ) ;
#97315 = PERSON_AND_ORGANIZATION_ROLE ( 'creator' ) ;
#97316 = FACE_OUTER_BOUND ( 'NONE', #98978, .T. ) ;
#97317 = CARTESIAN_POINT ( 'NONE',  ( -7.302954156136775232, -19.11528491071161540, 11.49999999999999645 ) ) ;
#97318 = CARTESIAN_POINT ( 'NONE',  ( -78.52287095715006160, -29.50250243563736774, 8.947779886222141599 ) ) ;
#97319 = DIRECTION ( 'NONE',  ( -1.000000000000000000, -0.000000000000000000, -5.238131417152343399E-15 ) ) ;
#97320 = ORIENTED_EDGE ( 'NONE', *, *, #9441, .T. ) ;
#97321 = DIRECTION ( 'NONE',  ( -3.773278334453079030E-23, 0.9999999999976377785, 2.173523156925979128E-06 ) ) ;
#97322 = DIRECTION ( 'NONE',  ( -0.5473052603538086647, -0.000000000000000000, -0.8369330630277725946 ) ) ;
#97323 = FACE_BOUND ( 'NONE', #3037, .T. ) ;
#97324 = EDGE_CURVE ( 'NONE', #65451, #75416, #22794, .T. ) ;
#97325 = CARTESIAN_POINT ( 'NONE',  ( -67.58953762381675290, -23.47596703998600276, 11.44779298504227505 ) ) ;
#97326 = VERTEX_POINT ( 'NONE', #34206 ) ;
#97327 = CARTESIAN_POINT ( 'NONE',  ( 6.199338013146583393, -6.376774720514415407, 20.11757922567734980 ) ) ;
#97328 = CARTESIAN_POINT ( 'NONE',  ( -11.53412672884717871, -19.92380006517282709, 11.49999999999999645 ) ) ;
#97329 = CARTESIAN_POINT ( 'NONE',  ( -19.53289989604362376, -11.71160353944097920, 11.49999999999998934 ) ) ;
#97330 = CARTESIAN_POINT ( 'NONE',  ( -110.6324683602788923, -23.85049219812686516, 10.88485053497526955 ) ) ;
#97331 = CARTESIAN_POINT ( 'NONE',  ( -122.5895376238167387, -24.64898659630368627, 1.056161002820394490 ) ) ;
#97332 = CARTESIAN_POINT ( 'NONE',  ( -49.99340013130950666, -25.20303235495079619, 3.351178797549144051 ) ) ;
#97333 = DIRECTION ( 'NONE',  ( -0.9496245541219264785, 6.845827386180410961E-16, -0.3133898629642195011 ) ) ;
#97334 = CARTESIAN_POINT ( 'NONE',  ( -54.55620429048340014, -23.48786465467240347, 11.44779295918255357 ) ) ;
#97335 = AXIS2_PLACEMENT_3D ( 'NONE', #81033, #87648, #72927 ) ;
#97336 = CARTESIAN_POINT ( 'NONE',  ( -9.708950231915746798, -19.59419465507263070, 11.49999999999998934 ) ) ;
#97337 = EDGE_CURVE ( 'NONE', #56850, #24103, #26590, .T. ) ;
#97338 = CARTESIAN_POINT ( 'NONE',  ( -59.52287095715006160, -24.64965694238407323, 8.947790433994201820 ) ) ;
#97339 = EDGE_CURVE ( 'NONE', #37998, #16727, #35201, .T. ) ;
#97340 = B_SPLINE_CURVE_WITH_KNOTS ( 'NONE', 3,
 ( #52226, #53729, #13141, #60846 ),
 .UNSPECIFIED., .F., .F.,
 ( 4, 4 ),
 ( 0.000000000000000000, 9.999999999997510880E-05 ),
 .UNSPECIFIED. ) ;
#97341 = CARTESIAN_POINT ( 'NONE',  ( -28.62287095715004881, -24.49608681932686949, 1.056161686216224860 ) ) ;
#97342 = DIRECTION ( 'NONE',  ( 0.9951627101165076983, 0.000000000000000000, 0.09824042138329622254 ) ) ;
#97343 = CARTESIAN_POINT ( 'NONE',  ( 9.071512145086499501, -0.9000000000000000222, 3.687490859131163923 ) ) ;
#97344 = ORIENTED_EDGE ( 'NONE', *, *, #32218, .F. ) ;
#97345 = CARTESIAN_POINT ( 'NONE',  ( -8.611577853089924517, -18.50786853157798006, 11.49999999999998934 ) ) ;
#97346 = ORIENTED_EDGE ( 'NONE', *, *, #31323, .T. ) ;
#97347 = ORIENTED_EDGE ( 'NONE', *, *, #38979, .F. ) ;
#97348 = ORIENTED_EDGE ( 'NONE', *, *, #79386, .F. ) ;
#97349 = ORIENTED_EDGE ( 'NONE', *, *, #70685, .F. ) ;
#97350 = CARTESIAN_POINT ( 'NONE',  ( 20.16173082093541424, 11.17373015621797627, -1.500000000000002220 ) ) ;
#97352 = EDGE_CURVE ( 'NONE', #36415, #2798, #40518, .T. ) ;
#97351 = CARTESIAN_POINT ( 'NONE',  ( -60.52287095715008292, -23.48783264082477018, -1.443836473390092801 ) ) ;
#97353 = CARTESIAN_POINT ( 'NONE',  ( -0.9278407348523283193, 20.21260682001012654, -1.500000000000002220 ) ) ;
#97354 = ORIENTED_EDGE ( 'NONE', *, *, #77692, .F. ) ;
#97355 = LINE ( 'NONE', #44067, #99533 ) ;
#97356 = CARTESIAN_POINT ( 'NONE',  ( -34.62287095715005592, -24.64965695001467694, 8.947790433994189385 ) ) ;
#97357 = EDGE_CURVE ( 'NONE', #38454, #75504, #20950, .T. ) ;
#97358 = B_SPLINE_CURVE_WITH_KNOTS ( 'NONE', 3,
 ( #2555, #80170, #81669, #89281 ),
 .UNSPECIFIED., .F., .F.,
 ( 4, 4 ),
 ( 0.000000000000000000, 1.000000000000000000 ),
 .UNSPECIFIED. ) ;
#97360 = CARTESIAN_POINT ( 'NONE',  ( -95.50376372625123622, -24.83618233451450408, 1.606449574219538157 ) ) ;
#97359 = VECTOR ( 'NONE', #24630, 1000.000000000000114 ) ;
#97361 = LINE ( 'NONE', #34465, #20435 ) ;
#97363 = ORIENTED_EDGE ( 'NONE', *, *, #57005, .F. ) ;
#97362 = CARTESIAN_POINT ( 'NONE',  ( 17.72605931280000391, -11.99821887194124770, 11.49999999999999645 ) ) ;
#97364 = LINE ( 'NONE', #27846, #95407 ) ;
#97365 = VECTOR ( 'NONE', #85249, 1000.000000000000114 ) ;
#97366 = EDGE_LOOP ( 'NONE', ( #11644, #22353, #39326, #13611, #36943, #75352, #94345, #69168 ) ) ;
#97367 = CARTESIAN_POINT ( 'NONE',  ( -20.07822104958740539, -9.643837532803976487, -1.500000000000002220 ) ) ;
#97368 = CARTESIAN_POINT ( 'NONE',  ( -17.26476610439243231, 11.37957233835482818, 11.49999999999998934 ) ) ;
#97369 = ORIENTED_EDGE ( 'NONE', *, *, #91023, .F. ) ;
#97370 = CARTESIAN_POINT ( 'NONE',  ( -6.499999999999992895, 2.573529411764704289, 1.544117647058822929 ) ) ;
#97371 = ORIENTED_EDGE ( 'NONE', *, *, #93085, .F. ) ;
#97372 = CARTESIAN_POINT ( 'NONE',  ( -129.5228709571500474, -23.72747288104470798, -1.053458166803224128 ) ) ;
#97373 = ORIENTED_EDGE ( 'NONE', *, *, #77633, .T. ) ;
#97374 = CARTESIAN_POINT ( 'NONE',  ( -111.7814946224345789, -25.28710546256127145, 4.332404433089555695 ) ) ;
#97375 = CARTESIAN_POINT ( 'NONE',  ( 17.15856466979341377, 12.00972951212132855, -1.500000000000002220 ) ) ;
#97376 = CARTESIAN_POINT ( 'NONE',  ( 19.28182042344761626, 10.37885539243483812, 11.49999999999999645 ) ) ;
#97377 = CARTESIAN_POINT ( 'NONE',  ( -89.50343196477413699, -24.66019654487199730, 8.947790411086115725 ) ) ;
#97378 = CARTESIAN_POINT ( 'NONE',  ( -22.36795837939145670, 2.692536522722862813, 11.49999999999998934 ) ) ;
#97379 = CARTESIAN_POINT ( 'NONE',  ( 10.03794737889396771, 18.37758748099471973, 11.49999999999998934 ) ) ;
#97380 = FACE_OUTER_BOUND ( 'NONE', #28327, .T. ) ;
#97381 = LINE ( 'NONE', #89770, #46385 ) ;
#97382 = CARTESIAN_POINT ( 'NONE',  ( -119.5930762842119464, -23.48786465467241769, 11.44779295918253581 ) ) ;
#97384 = EDGE_CURVE ( 'NONE', #70388, #12467, #74253, .T. ) ;
#97383 = CARTESIAN_POINT ( 'NONE',  ( -126.5562042904834215, -24.66019654487200086, 8.947790411086117501 ) ) ;
#97385 = ORIENTED_EDGE ( 'NONE', *, *, #21959, .T. ) ;
#97386 = ORIENTED_EDGE ( 'NONE', *, *, #85761, .T. ) ;
#97387 = VERTEX_POINT ( 'NONE', #4747 ) ;
#97388 = CARTESIAN_POINT ( 'NONE',  ( -66.50544697010404604, -24.15543982623906771, -0.2315651400026687845 ) ) ;
#97389 = B_SPLINE_CURVE_WITH_KNOTS ( 'NONE', 3,
 ( #61436, #92363, #77630, #23, #84753, #15240 ),
 .UNSPECIFIED., .F., .F.,
 ( 4, 2, 4 ),
 ( 0.000000000000000000, 0.001380764517854760195, 0.002761529035709520390 ),
 .UNSPECIFIED. ) ;
#97390 = CARTESIAN_POINT ( 'NONE',  ( -2.231587876719630437, -21.34735720706076378, -1.500000000000002220 ) ) ;
#97391 = CARTESIAN_POINT ( 'NONE',  ( 0.3085469314987323020, -5.876774720514413630, 19.52341893546493523 ) ) ;
#97392 = ORIENTED_EDGE ( 'NONE', *, *, #70799, .F. ) ;
#97393 = CARTESIAN_POINT ( 'NONE',  ( 17.90021246794804810, -11.17811638239879279, -1.500000000000002220 ) ) ;
#97394 = CARTESIAN_POINT ( 'NONE',  ( -70.75516459165498873, -25.29842503980747637, 4.197523792507152685 ) ) ;
#97395 = DIRECTION ( 'NONE',  ( -0.000000000000000000, -1.000000000000000000, -0.000000000000000000 ) ) ;
#97396 = DIRECTION ( 'NONE',  ( 0.000000000000000000, 0.000000000000000000, 1.000000000000000000 ) ) ;
#97397 = CARTESIAN_POINT ( 'NONE',  ( 31.63608488009067443, 0.6647747205144267646, 27.34773273846992225 ) ) ;
#97398 = CARTESIAN_POINT ( 'NONE',  ( -129.5558832449600857, -24.15620529776629155, 10.23563542870659759 ) ) ;
#97399 = CARTESIAN_POINT ( 'NONE',  ( 16.06085343747454175, -15.19291221174989204, -1.500000000000002220 ) ) ;
#97400 = CARTESIAN_POINT ( 'NONE',  ( -118.5228709571500758, -24.64898659630368627, 1.056161002820833028 ) ) ;
#97401 = CARTESIAN_POINT ( 'NONE',  ( -109.3415242670784835, -25.30488224429866406, 5.187382284604649563 ) ) ;
#97402 = LINE ( 'NONE', #27888, #22505 ) ;
#97403 = DIRECTION ( 'NONE',  ( 0.000000000000000000, -2.173523156925980399E-06, 0.9999999999976378895 ) ) ;
#97404 = CARTESIAN_POINT ( 'NONE',  ( -63.52287095715006160, -24.65952944569304606, 1.056160979905695463 ) ) ;
#97405 = CARTESIAN_POINT ( 'NONE',  ( 20.50650179695670872, -5.950058665555418180, -1.500000000000002220 ) ) ;
#97406 = LINE ( 'NONE', #58851, #1268 ) ;
#97407 = CARTESIAN_POINT ( 'NONE',  ( 32.16024265030974050, 5.965225279485572685, 16.27760796525321751 ) ) ;
#97408 = AXIS2_PLACEMENT_3D ( 'NONE', #74812, #45387, #91041 ) ;
#97409 = CARTESIAN_POINT ( 'NONE',  ( -64.55379066836746915, -23.96169478059713498, 10.65365249895718058 ) ) ;
#97410 = CARTESIAN_POINT ( 'NONE',  ( -53.62287095715005592, -29.50250243563736774, 8.947779886222146928 ) ) ;
#97411 = B_SPLINE_CURVE_WITH_KNOTS ( 'NONE', 3,
 ( #100351, #62845, #69434, #85149, #93766, #24747, #85658, #16138 ),
 .UNSPECIFIED., .F., .F.,
 ( 4, 2, 2, 4 ),
 ( 0.000000000000000000, 0.002001098010032684085, 0.003001647015049024609, 0.004002196020065364700 ),
 .UNSPECIFIED. ) ;
#97412 = CARTESIAN_POINT ( 'NONE',  ( 12.73759380600583846, -18.68238426224762350, -1.500000000000002220 ) ) ;
#97413 = EDGE_CURVE ( 'NONE', #41185, #100230, #17892, .T. ) ;
#97414 = EDGE_LOOP ( 'NONE', ( #69515, #35630, #24623, #37645 ) ) ;
#97415 = DIRECTION ( 'NONE',  ( -1.611864046919725738E-15, -0.000000000000000000, -1.000000000000000000 ) ) ;
#97416 = CARTESIAN_POINT ( 'NONE',  ( -104.5895376238167245, -24.64965694238408034, 8.947790433994649462 ) ) ;
#97417 = CARTESIAN_POINT ( 'NONE',  ( 17.61170953066113398, -8.936083093766256980, 11.49999999999999645 ) ) ;
#97418 = CARTESIAN_POINT ( 'NONE',  ( -82.62287095715005592, -24.64965695001468404, 8.947790433994182280 ) ) ;
#97419 = DIRECTION ( 'NONE',  ( -1.000000000000000000, 0.000000000000000000, 0.000000000000000000 ) ) ;
#97420 = ORIENTED_EDGE ( 'NONE', *, *, #8071, .T. ) ;
#97421 = CARTESIAN_POINT ( 'NONE',  ( -89.40841769935767047, -29.50249591506787894, 5.947779886229223045 ) ) ;
#97422 = CARTESIAN_POINT ( 'NONE',  ( -70.52287095715007581, -23.85229601348996198, 10.88205029486209163 ) ) ;
#97424 = EDGE_CURVE ( 'NONE', #41475, #62694, #85641, .T. ) ;
#97423 = CARTESIAN_POINT ( 'NONE',  ( -100.8583591130402937, -25.17353330799204514, 7.041620660005706966 ) ) ;
#97425 = CARTESIAN_POINT ( 'NONE',  ( -21.57582672592670292, -1.461774377805347802, 11.49999999999998934 ) ) ;
#97426 = ADVANCED_FACE ( 'NONE', ( #28086 ), #59039, .T. ) ;
#97427 = CARTESIAN_POINT ( 'NONE',  ( 3.797776442307698286, -6.376774720514401196, 18.16025641025640525 ) ) ;
#97428 = CARTESIAN_POINT ( 'NONE',  ( -40.52287095715006870, -23.47596703998600631, 11.44779298504229281 ) ) ;
#97429 = EDGE_CURVE ( 'NONE', #38183, #11909, #20451, .T. ) ;
#97430 = CARTESIAN_POINT ( 'NONE',  ( -10.31943567505730996, -5.151096386430394247, 28.35664311630200984 ) ) ;
#97431 = DIRECTION ( 'NONE',  ( 1.000000000000000000, 3.773278334444167608E-23, 8.201307833595939069E-29 ) ) ;
#97432 = CARTESIAN_POINT ( 'NONE',  ( -15.09475962229707591, 12.77647934908296712, 11.49999999999998934 ) ) ;
#97433 = CIRCLE ( 'NONE', #16364, 5.000000000000001776 ) ;
#97434 = ORIENTED_EDGE ( 'NONE', *, *, #77697, .F. ) ;
#97435 = ADVANCED_FACE ( 'NONE', ( #43807 ), #29068, .T. ) ;
#97436 = CARTESIAN_POINT ( 'NONE',  ( 20.24638344296597836, 0.1212440198127159030, 11.49999999999999645 ) ) ;
#97437 = LINE ( 'NONE', #35047, #74814 ) ;
#97438 = CARTESIAN_POINT ( 'NONE',  ( -44.52287095715006160, -24.65952944569303895, 1.056160979905691910 ) ) ;
#97439 = ORIENTED_EDGE ( 'NONE', *, *, #47622, .F. ) ;
#97440 = CARTESIAN_POINT ( 'NONE',  ( -37.52287095715006160, -24.51387760970724727, 9.387446482453418284 ) ) ;
#97441 = CARTESIAN_POINT ( 'NONE',  ( -28.52287095715005805, -29.50250243563660391, 8.947779535157950548 ) ) ;
#97442 = CYLINDRICAL_SURFACE ( 'NONE', #15953, 2.249999999999998668 ) ;
#97443 = CARTESIAN_POINT ( 'NONE',  ( -47.62287095715004881, -23.47593901973091235, -1.443836447539009749 ) ) ;
#97444 = LINE ( 'NONE', #75585, #57605 ) ;
#97445 = CARTESIAN_POINT ( 'NONE',  ( -8.782848147209532996, 18.00178819457707746, -1.500000000000002220 ) ) ;
#97446 = ADVANCED_FACE ( 'NONE', ( #67160 ), #21439, .F. ) ;
#97447 = CARTESIAN_POINT ( 'NONE',  ( -79.52287095715010423, -23.47593901973090524, -1.443836447538996870 ) ) ;
#97448 = ORIENTED_EDGE ( 'NONE', *, *, #1936, .F. ) ;
#97449 = B_SPLINE_CURVE_WITH_KNOTS ( 'NONE', 3,
 ( #50991, #29632, #53493, #6788, #83412, #37745 ),
 .UNSPECIFIED., .F., .F.,
 ( 4, 2, 4 ),
 ( 1.570887131794176733E-05, 0.001396322306279759555, 0.002776935741241577573 ),
 .UNSPECIFIED. ) ;
#97450 = ADVANCED_FACE ( 'NONE', ( #50764 ), #95430, .F. ) ;
#97451 = CARTESIAN_POINT ( 'NONE',  ( 8.978253834636468866, -6.376774720514426953, 21.48128695274316158 ) ) ;
#97452 = CARTESIAN_POINT ( 'NONE',  ( 30.57287095715020087, 6.475225279485571583, 25.41160796525326404 ) ) ;
#97453 = LINE ( 'NONE', #28938, #67879 ) ;
#97454 = CARTESIAN_POINT ( 'NONE',  ( -105.5228709571500758, -23.47593901973090524, -1.443836447538996426 ) ) ;
#97455 = EDGE_CURVE ( 'NONE', #46180, #5514, #86894, .T. ) ;
#97456 = DIRECTION ( 'NONE',  ( 0.000000000000000000, 0.000000000000000000, 1.000000000000000000 ) ) ;
#97457 = CARTESIAN_POINT ( 'NONE',  ( -71.62287095715005592, -24.66019654487199020, 8.947790411086131712 ) ) ;
#97458 = VERTEX_POINT ( 'NONE', #11681 ) ;
#97459 = CARTESIAN_POINT ( 'NONE',  ( -19.77321833943668850, 4.698914572609424134, -1.500000000000002220 ) ) ;
#97460 = VERTEX_POINT ( 'NONE', #56890 ) ;
#97461 = CARTESIAN_POINT ( 'NONE',  ( 6.461317529299694051, 22.01590093704556850, 11.49999999999998934 ) ) ;
#97462 = EDGE_CURVE ( 'NONE', #49715, #12228, #18309, .T. ) ;
#97463 = CARTESIAN_POINT ( 'NONE',  ( -32.53167805950398161, -24.51314013834315375, 0.6176544820404111791 ) ) ;
#97464 = ORIENTED_EDGE ( 'NONE', *, *, #70858, .T. ) ;
#97465 = DIRECTION ( 'NONE',  ( 0.000000000000000000, -0.9999999999976377785, -2.173523156925979975E-06 ) ) ;
#97466 = EDGE_CURVE ( 'NONE', #30992, #55957, #27600, .T. ) ;
#97467 = CARTESIAN_POINT ( 'NONE',  ( -108.8968792378191921, -25.14264220134206695, 6.986250900936221697 ) ) ;
#97468 = CARTESIAN_POINT ( 'NONE',  ( -38.58953762381672448, -24.66019654487199020, 8.947790411086129936 ) ) ;
#97469 = CARTESIAN_POINT ( 'NONE',  ( -19.38594737788604405, 8.525550480899875438, 11.49999999999999645 ) ) ;
#97470 = ORIENTED_EDGE ( 'NONE', *, *, #81840, .T. ) ;
#97471 = CARTESIAN_POINT ( 'NONE',  ( -5.843409716339609261, -21.38298466452703650, 11.49999999999998934 ) ) ;
#97472 = AXIS2_PLACEMENT_3D ( 'NONE', #53639, #45025, #98280 ) ;
#97473 = CARTESIAN_POINT ( 'NONE',  ( 18.80685554986811070, -8.408966509905500430, 11.49999999999998934 ) ) ;
#97474 = EDGE_LOOP ( 'NONE', ( #71032, #75267, #36408, #24063, #90117 ) ) ;
#97475 = ORIENTED_EDGE ( 'NONE', *, *, #77141, .F. ) ;
#97476 = FACE_OUTER_BOUND ( 'NONE', #58893, .T. ) ;
#97477 = B_SPLINE_CURVE_WITH_KNOTS ( 'NONE', 3,
 ( #35159, #15293, #22397, #61493, #30527, #83813 ),
 .UNSPECIFIED., .F., .F.,
 ( 4, 2, 4 ),
 ( 6.384118678620055848E-06, 0.001386860460828382791, 0.002767336802978145795 ),
 .UNSPECIFIED. ) ;
#97478 = CARTESIAN_POINT ( 'NONE',  ( -70.27422298781921484, -29.50249353255212270, 4.851626040077965385 ) ) ;
#97479 = ORIENTED_EDGE ( 'NONE', *, *, #76209, .F. ) ;
#97480 = VERTEX_POINT ( 'NONE', #81707 ) ;
#97481 = ORIENTED_EDGE ( 'NONE', *, *, #76787, .T. ) ;
#97482 = CARTESIAN_POINT ( 'NONE',  ( -77.52287095715006160, -23.48786465467241058, 11.44779295918254469 ) ) ;
#97483 = CARTESIAN_POINT ( 'NONE',  ( -28.58648369522600063, -24.19411652871865215, 9.817618374534072601 ) ) ;
#97484 = CARTESIAN_POINT ( 'NONE',  ( -80.43221577628075636, -29.50249378334325101, 4.967010655462308577 ) ) ;
#97485 = CARTESIAN_POINT ( 'NONE',  ( 5.906898857431191807, -19.90033995357616092, -1.500000000000002220 ) ) ;
#97486 = CARTESIAN_POINT ( 'NONE',  ( 20.88924836996103451, 6.054424527964996194, 11.49999999999999645 ) ) ;
#97487 = ORIENTED_EDGE ( 'NONE', *, *, #35331, .F. ) ;
#97488 = CARTESIAN_POINT ( 'NONE',  ( -122.5228709571500758, -23.47593901973090524, -1.443836447538996204 ) ) ;
#97489 = CARTESIAN_POINT ( 'NONE',  ( 28.20688450243646272, -5.356774720514425603, -7.073367244510395224 ) ) ;
#97490 = CARTESIAN_POINT ( 'NONE',  ( -19.78178409256797465, 10.57734301857266246, 11.49999999999998934 ) ) ;
#97491 = CARTESIAN_POINT ( 'NONE',  ( 22.81105451610979173, -6.475225279485573360, -19.61691820600746539 ) ) ;
#97492 = CARTESIAN_POINT ( 'NONE',  ( -65.58122548746410985, -24.83618233451449697, 1.606449574219540155 ) ) ;
#97493 = ORIENTED_EDGE ( 'NONE', *, *, #1253, .T. ) ;
#97494 = CARTESIAN_POINT ( 'NONE',  ( -59.52287095715008292, -23.72773821059535848, 11.05748984161097681 ) ) ;
#97495 = AXIS2_PLACEMENT_3D ( 'NONE', #97318, #83068, #19184 ) ;
#97496 = CARTESIAN_POINT ( 'NONE',  ( -77.58953762381675290, -23.47596703998600276, 11.44779298504227683 ) ) ;
#97497 = CC_DESIGN_APPROVAL ( #80452, ( #21292 ) ) ;
#97498 = ORIENTED_EDGE ( 'NONE', *, *, #62267, .F. ) ;
#97499 = VERTEX_POINT ( 'NONE', #58383 ) ;
#97500 = CARTESIAN_POINT ( 'NONE',  ( -8.376690734369036662, 11.49999999999999645, 0.000000000000000000 ) ) ;
#97501 = ORIENTED_EDGE ( 'NONE', *, *, #9917, .T. ) ;
#97502 = CARTESIAN_POINT ( 'NONE',  ( -6.620899627221215944, -20.26055204357936290, -1.500000000000002220 ) ) ;
#97503 = ORIENTED_EDGE ( 'NONE', *, *, #20672, .F. ) ;
#97504 = CARTESIAN_POINT ( 'NONE',  ( -6.033988668995577065, -5.876774720514413630, 19.86422795159478483 ) ) ;
#97505 = CARTESIAN_POINT ( 'NONE',  ( 17.39636294008568740, -13.23181597624684791, 11.49999999999998934 ) ) ;
#97506 = CARTESIAN_POINT ( 'NONE',  ( -45.52287095715004739, -23.48783264082477018, -1.443836473390097019 ) ) ;
#97507 = CARTESIAN_POINT ( 'NONE',  ( -1.179572987637725889, 22.66035800735570049, -1.500000000000002220 ) ) ;
#97508 = DIRECTION ( 'NONE',  ( 0.000000000000000000, 0.000000000000000000, 1.000000000000000000 ) ) ;
#97509 = CYLINDRICAL_SURFACE ( 'NONE', #77324, 1.149999999999998135 ) ;
#97510 = CARTESIAN_POINT ( 'NONE',  ( 21.92589416912191069, -1.073809401359021143, -1.500000000000002220 ) ) ;
#97511 = CARTESIAN_POINT ( 'NONE',  ( 7.041152093163508319, -5.876774720514423400, 21.17127001373575368 ) ) ;
#97512 = ORIENTED_EDGE ( 'NONE', *, *, #67221, .T. ) ;
#97513 = CARTESIAN_POINT ( 'NONE',  ( 29.77147767949874435, -6.376774720514426953, 26.15915692125051706 ) ) ;
#97514 = LINE ( 'NONE', #12267, #16768 ) ;
#97515 = ORIENTED_EDGE ( 'NONE', *, *, #93991, .T. ) ;
#97516 = CARTESIAN_POINT ( 'NONE',  ( -32.52287095715006160, -23.95044443724991368, 10.65354141964649948 ) ) ;
#97517 = CARTESIAN_POINT ( 'NONE',  ( 10.24966870126729646, 6.475225279485571583, -27.02528057709740850 ) ) ;
#97518 = CARTESIAN_POINT ( 'NONE',  ( -10.19904569043877984, -23.73148148933709578, 3.856996771330998719 ) ) ;
#97519 = CARTESIAN_POINT ( 'NONE',  ( -16.96849063341007380, -12.82450338531451450, 11.49999999999998934 ) ) ;
#97520 = CARTESIAN_POINT ( 'NONE',  ( -112.6235203339132340, -24.65952944569305316, 1.056160979905707897 ) ) ;
#97521 = CARTESIAN_POINT ( 'NONE',  ( -26.42246413733907673, -24.75186158583077400, 3.141773372700918721 ) ) ;
#97522 = DIRECTION ( 'NONE',  ( 0.8246584009594635223, 0.5656310827093757876, 2.309263891220325920E-14 ) ) ;
#97523 = CARTESIAN_POINT ( 'NONE',  ( -68.59719488501549733, -23.96119346886880663, -0.6495511937832112448 ) ) ;
#97524 = AXIS2_PLACEMENT_3D ( 'NONE', #13508, #27753, #20133 ) ;
#97525 = CARTESIAN_POINT ( 'NONE',  ( -29.49875734969026198, 0.3587747205144265483, 10.11402280011862587 ) ) ;
#97526 = ORIENTED_EDGE ( 'NONE', *, *, #75071, .F. ) ;
#97527 = EDGE_CURVE ( 'NONE', #3028, #92001, #19789, .T. ) ;
#97528 = CARTESIAN_POINT ( 'NONE',  ( -13.92019785312828972, -13.74635529968554515, 11.49999999999999645 ) ) ;
#97529 = CARTESIAN_POINT ( 'NONE',  ( -105.5228709571500758, -23.48786465467241769, 11.44779295918253936 ) ) ;
#97530 = ADVANCED_FACE ( 'NONE', ( #43154 ), #80206, .T. ) ;
#97531 = CARTESIAN_POINT ( 'NONE',  ( -27.89245932500631397, -24.65620490964798250, 8.246149411531419560 ) ) ;
#97532 = ORIENTED_EDGE ( 'NONE', *, *, #603, .T. ) ;
#97533 = ADVANCED_FACE ( 'NONE', ( #25916 ), #94927, .F. ) ;
#97534 = CARTESIAN_POINT ( 'NONE',  ( 4.115044103975469270, -6.376774720514427841, 21.79213183355573946 ) ) ;
#97535 = FACE_OUTER_BOUND ( 'NONE', #82025, .T. ) ;
#97536 = EDGE_CURVE ( 'NONE', #64400, #34336, #63929, .T. ) ;
#97537 = CARTESIAN_POINT ( 'NONE',  ( -31.62287095715005236, -23.47593901973091235, -1.443836447539013301 ) ) ;
#97538 = EDGE_CURVE ( 'NONE', #27461, #48074, #43765, .T. ) ;
#97539 = DIRECTION ( 'NONE',  ( 0.000000000000000000, -0.000000000000000000, 1.000000000000000000 ) ) ;
#97540 = CARTESIAN_POINT ( 'NONE',  ( -15.16924259816527609, 12.53091941037558854, -1.500000000000002220 ) ) ;
#97541 = ORIENTED_EDGE ( 'NONE', *, *, #43781, .T. ) ;
#97542 = AXIS2_PLACEMENT_3D ( 'NONE', #26936, #57904, #73121 ) ;
#97543 = CARTESIAN_POINT ( 'NONE',  ( -81.52287095715006160, -29.50250786944525672, 11.44777988621623521 ) ) ;
#97544 = CARTESIAN_POINT ( 'NONE',  ( 3.036358173076929123, -5.876774720514420736, 20.87990785256409865 ) ) ;
#97545 = PERSON_AND_ORGANIZATION ( #70597, #27821 ) ;
#97546 = VERTEX_POINT ( 'NONE', #33532 ) ;
#97547 = CARTESIAN_POINT ( 'NONE',  ( -107.6228709571500701, -24.64965695001469115, 8.947790433994176951 ) ) ;
#97548 = CARTESIAN_POINT ( 'NONE',  ( -1.409217194013772101, -6.376774720514417183, 20.11414146978959749 ) ) ;
#97549 = CARTESIAN_POINT ( 'NONE',  ( -47.55323112900108384, -23.96119346886880663, -0.6495511937831951466 ) ) ;
#97550 = DIRECTION ( 'NONE',  ( -0.000000000000000000, -1.000000000000000000, -0.000000000000000000 ) ) ;
#97551 = DIRECTION ( 'NONE',  ( -0.000000000000000000, -1.000000000000000000, -0.000000000000000000 ) ) ;
#97552 = CARTESIAN_POINT ( 'NONE',  ( -69.96836528472165639, -25.31201604173465114, 5.376154465515825542 ) ) ;
#97553 = CARTESIAN_POINT ( 'NONE',  ( 14.76093561896379214, 6.475225279485573360, -26.55548769130089681 ) ) ;
#97554 = CARTESIAN_POINT ( 'NONE',  ( -11.44242300287478820, -16.35863574123370512, -1.500000000000002220 ) ) ;
#97555 = ADVANCED_FACE ( 'NONE', ( #3102 ), #10195, .T. ) ;
#97556 = CARTESIAN_POINT ( 'NONE',  ( -32.52287095715005449, -24.50216790748203621, 0.6166512839542446223 ) ) ;
#97557 = CARTESIAN_POINT ( 'NONE',  ( -0.07904045033472657800, -22.02675925722719441, 0.06506293307687280314 ) ) ;
#97558 = ORIENTED_EDGE ( 'NONE', *, *, #11189, .F. ) ;
#97559 = CARTESIAN_POINT ( 'NONE',  ( -63.52287095715006160, -24.64898659630367561, 1.056161002820822592 ) ) ;
#97560 = DIRECTION ( 'NONE',  ( -0.9890158633619159367, -0.1478094111296165969, 0.000000000000000000 ) ) ;
#97561 = VECTOR ( 'NONE', #46229, 1000.000000000000114 ) ;
#97562 = EDGE_CURVE ( 'NONE', #30827, #18132, #33524, .T. ) ;
#97563 = B_SPLINE_CURVE_WITH_KNOTS ( 'NONE', 3,
 ( #17124, #48093, #54210, #40475, #23732, #9516 ),
 .UNSPECIFIED., .F., .F.,
 ( 4, 2, 4 ),
 ( 6.384118678610141327E-06, 0.001386860460828372599, 0.002767336802978134953 ),
 .UNSPECIFIED. ) ;
#97564 = SECURITY_CLASSIFICATION ( '', '', #51885 ) ;
#97565 = CARTESIAN_POINT ( 'NONE',  ( 12.30588647384254841, -6.376774720514765349, -28.11066263748569227 ) ) ;
#97566 = CARTESIAN_POINT ( 'NONE',  ( -124.4728709571500360, -25.30558663486635851, 5.000950659935021747 ) ) ;
#97567 = CARTESIAN_POINT ( 'NONE',  ( -81.50255920297891521, -24.51314013834316796, 0.6176544820404249458 ) ) ;
#97568 = LINE ( 'NONE', #67144, #58056 ) ;
#97569 = CARTESIAN_POINT ( 'NONE',  ( -10.34999999999999254, -1.267509437117509414E-15, 0.000000000000000000 ) ) ;
#97570 = ORIENTED_EDGE ( 'NONE', *, *, #21808, .T. ) ;
#97571 = FACE_OUTER_BOUND ( 'NONE', #44211, .T. ) ;
#97572 = CARTESIAN_POINT ( 'NONE',  ( -127.5561563051774385, -23.73766607897670866, -1.055555164236447574 ) ) ;
#97573 = ORIENTED_EDGE ( 'NONE', *, *, #27996, .T. ) ;
#97574 = CARTESIAN_POINT ( 'NONE',  ( 18.19722386731275066, -8.884848157732822216, -1.500000000000002220 ) ) ;
#97575 = CARTESIAN_POINT ( 'NONE',  ( -97.62287095715008434, -23.47596703998600631, 11.44779298504227860 ) ) ;
#97576 = FACE_OUTER_BOUND ( 'NONE', #97982, .T. ) ;
#97577 = CARTESIAN_POINT ( 'NONE',  ( 14.52511747680497933, 5.965225279485572685, -27.86035006098926559 ) ) ;
#97579 = VERTEX_POINT ( 'NONE', #96431 ) ;
#97578 = EDGE_CURVE ( 'NONE', #83369, #59550, #69820, .T. ) ;
#97580 = DIRECTION ( 'NONE',  ( -0.000000000000000000, -1.000000000000000000, -0.000000000000000000 ) ) ;
#97581 = CARTESIAN_POINT ( 'NONE',  ( -105.5895376238167103, -25.00158670708909625, 2.256160236439166411 ) ) ;
#97582 = CARTESIAN_POINT ( 'NONE',  ( -5.935188749463110369, 19.13178230186815298, -1.500000000000002220 ) ) ;
#97583 = CARTESIAN_POINT ( 'NONE',  ( -19.40065202112720755, 8.109199488025859992, 11.49999999999999645 ) ) ;
#97584 = CARTESIAN_POINT ( 'NONE',  ( -29.23548819942161003, -25.20429460498101193, 5.522040770699941703 ) ) ;
#97585 = CARTESIAN_POINT ( 'NONE',  ( -70.58423071201757182, -24.73531770709095312, 8.716586749053508498 ) ) ;
#97586 = CARTESIAN_POINT ( 'NONE',  ( -21.55788180805707555, 4.768121097544787190, -1.500000000000002220 ) ) ;
#97587 = EDGE_CURVE ( 'NONE', #79917, #63070, #79530, .T. ) ;
#97588 = CARTESIAN_POINT ( 'NONE',  ( 6.655121222440027573, 5.350247568484731708, -25.44127467601040138 ) ) ;
#97589 = AXIS2_PLACEMENT_3D ( 'NONE', #55607, #78416, #84535 ) ;
#97590 = CARTESIAN_POINT ( 'NONE',  ( -117.6228709571500559, -23.48786465467241769, 11.44779295918253759 ) ) ;
#97591 = CARTESIAN_POINT ( 'NONE',  ( -50.20044999871004165, -25.18440104506130339, 3.305837384632741127 ) ) ;
#97592 = EDGE_LOOP ( 'NONE', ( #32619, #69995, #88961, #55432 ) ) ;
#97593 = FACE_OUTER_BOUND ( 'NONE', #91443, .T. ) ;
#97594 = CARTESIAN_POINT ( 'NONE',  ( -31.48876216871021683, -24.34968618360933590, 0.1864209137778850556 ) ) ;
#97595 = VERTEX_POINT ( 'NONE', #42167 ) ;
#97596 = VERTEX_POINT ( 'NONE', #50265 ) ;
#97597 = DIRECTION ( 'NONE',  ( 0.9888510809027409865, 7.885106708985486076E-16, 0.1489078231574183231 ) ) ;
#97598 = CARTESIAN_POINT ( 'NONE',  ( -89.58953762381671027, -23.48786465467241413, 11.44779295918254114 ) ) ;
#97599 = PLANE ( 'NONE',  #13110 ) ;
#97600 = CARTESIAN_POINT ( 'NONE',  ( -7.709890279958820258, -19.11728055126480186, -1.500000000000002220 ) ) ;
#97601 = CARTESIAN_POINT ( 'NONE',  ( -21.46803524902295024, 1.580295693706654347, 11.49999999999999645 ) ) ;
#97602 = ORIENTED_EDGE ( 'NONE', *, *, #65892, .T. ) ;
#97603 = CARTESIAN_POINT ( 'NONE',  ( -83.62287095715011276, -23.95044443724992789, 10.65354141964649592 ) ) ;
#97604 = CARTESIAN_POINT ( 'NONE',  ( -56.58953762381671737, -24.66019654487199020, 8.947790411086133489 ) ) ;
#97605 = FACE_OUTER_BOUND ( 'NONE', #76242, .T. ) ;
#97606 = CARTESIAN_POINT ( 'NONE',  ( 13.15158565771796084, -18.08388448789661851, 11.49999999999998934 ) ) ;
#97607 = DIRECTION ( 'NONE',  ( 0.000000000000000000, 0.000000000000000000, -1.000000000000000000 ) ) ;
#97608 = DIRECTION ( 'NONE',  ( 0.000000000000000000, 0.000000000000000000, 1.000000000000000000 ) ) ;
#97609 = ORIENTED_EDGE ( 'NONE', *, *, #14238, .T. ) ;
#97610 = CARTESIAN_POINT ( 'NONE',  ( -94.52287095715001897, -23.73907113216990084, -1.053371485793246798 ) ) ;
#97611 = DIRECTION ( 'NONE',  ( -0.000000000000000000, 1.000000000000000000, -0.000000000000000000 ) ) ;
#97612 = AXIS2_PLACEMENT_3D ( 'NONE', #450, #56266, #55259 ) ;
#97613 = CARTESIAN_POINT ( 'NONE',  ( 3.889286922045745776, 20.52237432693057073, 11.49999999999998934 ) ) ;
#97614 = ORIENTED_EDGE ( 'NONE', *, *, #42697, .T. ) ;
#97616 = ORIENTED_EDGE ( 'NONE', *, *, #17378, .F. ) ;
#97615 = DIRECTION ( 'NONE',  ( 0.000000000000000000, -2.173523156925980399E-06, 0.9999999999976378895 ) ) ;
#97617 = EDGE_LOOP ( 'NONE', ( #92340, #6083, #56814, #23733 ) ) ;
#97618 = CARTESIAN_POINT ( 'NONE',  ( -100.5972929639658844, -23.85049219812686161, 10.88485053497527133 ) ) ;
#97619 = CARTESIAN_POINT ( 'NONE',  ( 4.565063516603933280, 20.63981631578574039, -1.500000000000002220 ) ) ;
#97620 = ORIENTED_EDGE ( 'NONE', *, *, #7371, .F. ) ;
#97621 = CARTESIAN_POINT ( 'NONE',  ( 9.278253834636473130, -5.876774720514426953, 18.21871304725684482 ) ) ;
#97622 = CARTESIAN_POINT ( 'NONE',  ( 18.22465585706453339, -0.5000000000000000000, -2.153101996372891236 ) ) ;
#97623 = DIRECTION ( 'NONE',  ( 0.000000000000000000, 0.9999999999976377785, 2.173523156925979128E-06 ) ) ;
#97624 = CARTESIAN_POINT ( 'NONE',  ( -103.5228709571500758, -29.50248528299804818, 1.056150453629042030 ) ) ;
#97625 = CARTESIAN_POINT ( 'NONE',  ( 7.141559373243376641, -6.376774720514415407, 19.83742167145384983 ) ) ;
#97626 = CARTESIAN_POINT ( 'NONE',  ( 18.41774212405765709, -11.57998961627671441, -1.500000000000002220 ) ) ;
#97627 = CARTESIAN_POINT ( 'NONE',  ( -80.51244414166535535, -25.04307398257883577, 7.563174194274490780 ) ) ;
#97629 = ORIENTED_EDGE ( 'NONE', *, *, #88042, .F. ) ;
#97628 = CARTESIAN_POINT ( 'NONE',  ( -20.55042600948665310, 8.738301046694649798, 11.49999999999999645 ) ) ;
#97630 = CARTESIAN_POINT ( 'NONE',  ( -90.52287095715006160, -29.50250786944525672, 11.44777988621623344 ) ) ;
#97631 = CARTESIAN_POINT ( 'NONE',  ( 15.29947331669757737, 3.406413700670902323, -27.16854001216721670 ) ) ;
#97632 = DIRECTION ( 'NONE',  ( 0.000000000000000000, 0.000000000000000000, 1.000000000000000000 ) ) ;
#97633 = VERTEX_POINT ( 'NONE', #52394 ) ;
#97634 = EDGE_LOOP ( 'NONE', ( #17658, #78583, #57384, #14497 ) ) ;
#97635 = B_SPLINE_CURVE_WITH_KNOTS ( 'NONE', 3,
 ( #32520, #2090, #41649, #56882, #64507, #86802 ),
 .UNSPECIFIED., .F., .F.,
 ( 4, 2, 4 ),
 ( 0.000000000000000000, 0.001380764517853253154, 0.002761529035706506308 ),
 .UNSPECIFIED. ) ;
#97636 = AXIS2_PLACEMENT_3D ( 'NONE', #97421, #80203, #4082 ) ;
#97637 = EDGE_LOOP ( 'NONE', ( #31193, #82507, #92424, #67648 ) ) ;
#97638 = CC_DESIGN_APPROVAL ( #93371, ( #10919 ) ) ;
#97639 = CARTESIAN_POINT ( 'NONE',  ( -95.52287095715006160, -24.99156044556203327, 7.747789690856173195 ) ) ;
#97640 = FACE_OUTER_BOUND ( 'NONE', #88997, .T. ) ;
#97641 = CARTESIAN_POINT ( 'NONE',  ( 29.71903944837828604, -4.668615314384465087, 27.69752233256919993 ) ) ;
#97642 = CARTESIAN_POINT ( 'NONE',  ( -49.10841169077954049, -25.28221692862581804, 4.100616102390435280 ) ) ;
#97644 = CARTESIAN_POINT ( 'NONE',  ( 31.44230187582509117, 4.132774720514425404, -3.488634554324459014 ) ) ;
#97643 = AXIS2_PLACEMENT_3D ( 'NONE', #44507, #82065, #12549 ) ;
#97645 = CARTESIAN_POINT ( 'NONE',  ( -31.52287095715007581, -23.96177878511307213, 10.65340807706330750 ) ) ;
#97646 = ORIENTED_EDGE ( 'NONE', *, *, #22751, .T. ) ;
#97647 = EDGE_CURVE ( 'NONE', #65066, #87928, #22414, .T. ) ;
#97648 = CARTESIAN_POINT ( 'NONE',  ( -1.428710472040144452, 19.32843595812722626, 11.49999999999999645 ) ) ;
#97649 = DIRECTION ( 'NONE',  ( 0.000000000000000000, -1.000000000000000000, 0.000000000000000000 ) ) ;
#97650 = AXIS2_PLACEMENT_3D ( 'NONE', #921, #68550, #6144 ) ;
#97651 = ORIENTED_EDGE ( 'NONE', *, *, #45493, .F. ) ;
#97652 = FACE_OUTER_BOUND ( 'NONE', #71120, .T. ) ;
#97653 = EDGE_CURVE ( 'NONE', #51956, #33854, #92348, .T. ) ;
#97654 = CARTESIAN_POINT ( 'NONE',  ( 2.590388488674697953, -5.876774720514416295, 19.94764386045124027 ) ) ;
#97655 = DIRECTION ( 'NONE',  ( 1.000000000000000000, 0.000000000000000000, 0.000000000000000000 ) ) ;
#97656 = ADVANCED_FACE ( 'NONE', ( #22903 ), #90947, .F. ) ;
#97657 = DIRECTION ( 'NONE',  ( -1.000000000000000000, -3.773278334444167608E-23, -8.201307833595939069E-29 ) ) ;
#97658 = CARTESIAN_POINT ( 'NONE',  ( -15.96901387740391343, -11.39031854172415947, -1.500000000000002220 ) ) ;
#97659 = B_SPLINE_SURFACE_WITH_KNOTS ( 'NONE', 3, 3, ( 
 ( #8137, #40084, #39074, #94862 ),
 ( #56329, #55320, #513, #61926 ),
 ( #62427, #93859, #62938, #16239 ),
 ( #15734, #46702, #86255, #16734 ),
 ( #72047, #12626, #64953, #80646 ),
 ( #34972, #26359, #33463, #81145 ),
 ( #42600, #49714, #20230, #42101 ) ),
 .UNSPECIFIED., .F., .F., .F.,
 ( 4, 3, 4 ),
 ( 4, 4 ),
 ( 0.3389040617923331777, 0.5146334493826508760, 0.6903628369729686298 ),
 ( 0.5884930944281638876, 0.6165182179194964585 ),
 .UNSPECIFIED. ) ;
#97660 = EDGE_CURVE ( 'NONE', #14117, #20204, #43239, .T. ) ;
#97661 = CARTESIAN_POINT ( 'NONE',  ( -46.62370088052639971, -24.65952944569304606, 1.056160979905696351 ) ) ;
#97662 = EDGE_LOOP ( 'NONE', ( #17372, #47458, #64438, #1631, #2888, #94478, #80095, #40546, #79502, #44184, #62537, #86487, #68672, #33993 ) ) ;
#97663 = CARTESIAN_POINT ( 'NONE',  ( -5.754811884962036217, -20.78327508566754389, 11.49999999999998934 ) ) ;
#97664 = CARTESIAN_POINT ( 'NONE',  ( -56.62287095715005592, -24.64898659630528499, 1.056161002820822592 ) ) ;
#97665 = EDGE_CURVE ( 'NONE', #53585, #62582, #82050, .T. ) ;
#97666 = DIRECTION ( 'NONE',  ( 0.000000000000000000, -1.000000000000000000, 0.000000000000000000 ) ) ;
#97667 = CARTESIAN_POINT ( 'NONE',  ( -40.57354299436993017, -23.48783264082477018, -1.443836473390102793 ) ) ;
#97668 = CARTESIAN_POINT ( 'NONE',  ( -99.62727860833967952, -25.27473303363792922, 3.670122111435337953 ) ) ;
#97669 = CARTESIAN_POINT ( 'NONE',  ( 10.47623847176155820, -20.49086732513842080, -1.500000000000002220 ) ) ;
#97670 = AXIS2_PLACEMENT_3D ( 'NONE', #75931, #66499, #6435 ) ;
#97671 = COORDINATED_UNIVERSAL_TIME_OFFSET ( 0, 0, .AHEAD. ) ;
#97672 = DIRECTION ( 'NONE',  ( -0.000000000000000000, 1.000000000000000000, -0.000000000000000000 ) ) ;
#97673 = DIRECTION ( 'NONE',  ( 0.000000000000000000, -2.173523156925980399E-06, 0.9999999999976378895 ) ) ;
#97674 = CARTESIAN_POINT ( 'NONE',  ( -9.895454706725905325, 17.58729670687104729, 11.49999999999999645 ) ) ;
#97675 = CARTESIAN_POINT ( 'NONE',  ( -109.0059884841570153, -25.10927603167520417, 3.784296689362763644 ) ) ;
#97676 = CARTESIAN_POINT ( 'NONE',  ( -32.61960262707817293, -23.48786465467240347, 11.44779295918255535 ) ) ;
#97677 = DIRECTION ( 'NONE',  ( 0.000000000000000000, 2.173523156925980399E-06, -0.9999999999976378895 ) ) ;
#97678 = LINE ( 'NONE', #34295, #5123 ) ;
#97679 = EDGE_CURVE ( 'NONE', #35661, #93691, #30034, .T. ) ;
#97680 = CARTESIAN_POINT ( 'NONE',  ( -126.5895376238167529, -24.64965694238408034, 8.947790433994645909 ) ) ;
#97681 = CARTESIAN_POINT ( 'NONE',  ( -12.84220538718065185, 15.17226672225704398, 11.49999999999998934 ) ) ;
#97682 = VECTOR ( 'NONE', #46808, 1000.000000000000114 ) ;
#97683 = CARTESIAN_POINT ( 'NONE',  ( -113.5904894942459720, -24.15543982623907837, -0.2315651400026574602 ) ) ;
#97684 = CARTESIAN_POINT ( 'NONE',  ( 10.86211995951333620, 16.47970581058804740, -1.500000000000002220 ) ) ;
#97685 = ADVANCED_FACE ( 'NONE', ( #28545 ), #42830, .T. ) ;
#97686 = CARTESIAN_POINT ( 'NONE',  ( -126.5552517768743286, -24.35071581493544102, 9.817618358456011052 ) ) ;
#97687 = VECTOR ( 'NONE', #98533, 1000.000000000000000 ) ;
#97688 = CARTESIAN_POINT ( 'NONE',  ( -55.62287095715005592, -29.50247984919015209, -1.443849546365056913 ) ) ;
#97689 = CARTESIAN_POINT ( 'NONE',  ( 3.559170184186323915, -6.376774720514402972, 18.55412939673608719 ) ) ;
#97690 = CARTESIAN_POINT ( 'NONE',  ( -1.706377481887368486, -20.59057665607738130, 11.49999999999999645 ) ) ;
#97691 = CARTESIAN_POINT ( 'NONE',  ( 7.344278919687202922, -6.376774720514417183, 20.19896341048075783 ) ) ;
#97692 = CARTESIAN_POINT ( 'NONE',  ( 31.27821779315964790, 4.116118814799345493, -3.972734673865978117 ) ) ;
#97693 = CARTESIAN_POINT ( 'NONE',  ( -15.33504971967173702, 16.71734053393862496, 11.49999999999999645 ) ) ;
#97694 = VERTEX_POINT ( 'NONE', #91435 ) ;
#97695 = DIRECTION ( 'NONE',  ( -0.000000000000000000, -1.000000000000000000, -0.000000000000000000 ) ) ;
#97696 = CARTESIAN_POINT ( 'NONE',  ( -62.52287095715006160, -23.47593901973090169, -1.443836447538997092 ) ) ;
#97697 = EDGE_CURVE ( 'NONE', #73137, #3035, #60020, .T. ) ;
#97698 = CARTESIAN_POINT ( 'NONE',  ( -63.51556559896057053, -23.73766607897669445, -1.055555164236456900 ) ) ;
#97699 = CARTESIAN_POINT ( 'NONE',  ( -2.457093156980370452, -6.376774720514411854, 19.51167604195716976 ) ) ;
#97700 = EDGE_LOOP ( 'NONE', ( #35748, #2038, #64891, #27141, #5373, #95522, #3522, #16, #31921, #30178, #66057, #66584, #45968, #23594 ) ) ;
#97701 = ORIENTED_EDGE ( 'NONE', *, *, #88964, .T. ) ;
#97702 = VECTOR ( 'NONE', #54142, 1000.000000000000114 ) ;
#97703 = CARTESIAN_POINT ( 'NONE',  ( 0.3908843598833069422, -5.876774720514419847, 20.63520656483649773 ) ) ;
#97704 = B_SPLINE_CURVE_WITH_KNOTS ( 'NONE', 3,
 ( #18457, #19449, #64669, #64162 ),
 .UNSPECIFIED., .F., .F.,
 ( 4, 4 ),
 ( 0.000000000000000000, 9.999999999999592548E-05 ),
 .UNSPECIFIED. ) ;
#97705 = CARTESIAN_POINT ( 'NONE',  ( -20.58715743568940226, -9.973749938417524774, 11.49999999999998934 ) ) ;
#97706 = CARTESIAN_POINT ( 'NONE',  ( -29.65134019565081047, -23.88568904270062276, -0.6495508823503304274 ) ) ;
#97707 = CARTESIAN_POINT ( 'NONE',  ( -16.67190562677319932, -13.68652177170558204, -1.500000000000002220 ) ) ;
#97708 = CARTESIAN_POINT ( 'NONE',  ( -113.5585651354342502, -23.48786465467241058, 11.44779295918254292 ) ) ;
#97709 = FACE_OUTER_BOUND ( 'NONE', #98281, .T. ) ;
#97710 = LOCAL_TIME ( 0, 54, 15.00000000000000000, #53648 ) ;
#97711 = CARTESIAN_POINT ( 'NONE',  ( 6.936750662203477802, 21.44973376661030429, 11.49999999999999645 ) ) ;
#97712 = ORIENTED_EDGE ( 'NONE', *, *, #78044, .T. ) ;
#97713 = CARTESIAN_POINT ( 'NONE',  ( -28.24471377493544111, -24.85223738551369266, 2.395901059869563809 ) ) ;
#97714 = CARTESIAN_POINT ( 'NONE',  ( 12.93620265873104991, 17.78788284566447331, -1.500000000000002220 ) ) ;
#97715 = CARTESIAN_POINT ( 'NONE',  ( -111.5868598658171891, -24.65952944569305316, 1.056160979905705455 ) ) ;
#97716 = CARTESIAN_POINT ( 'NONE',  ( -70.52287095715007581, -25.00182538069145366, 7.747789668545101094 ) ) ;
#97717 = AXIS2_PLACEMENT_3D ( 'NONE', #51262, #19794, #35544 ) ;
#97718 = VERTEX_POINT ( 'NONE', #21917 ) ;
#97719 = CARTESIAN_POINT ( 'NONE',  ( -98.52287095715006160, -29.50250243563736774, 8.947779886222138046 ) ) ;
#97720 = EDGE_CURVE ( 'NONE', #17929, #87231, #100160, .T. ) ;
#97721 = DIRECTION ( 'NONE',  ( 0.000000000000000000, -2.173523156925979552E-06, 0.9999999999976378895 ) ) ;
#97722 = ORIENTED_EDGE ( 'NONE', *, *, #74300, .T. ) ;
#97723 = CARTESIAN_POINT ( 'NONE',  ( -84.62287095715007013, -23.94994826722515668, -0.6494450866351710872 ) ) ;
#97724 = ORIENTED_EDGE ( 'NONE', *, *, #17492, .F. ) ;
#97725 = VECTOR ( 'NONE', #91739, 1000.000000000000000 ) ;
#97726 = ORIENTED_EDGE ( 'NONE', *, *, #74006, .T. ) ;
#97727 = CARTESIAN_POINT ( 'NONE',  ( -49.73963891290676287, -25.31032741935931440, 5.370288135609136759 ) ) ;
#97728 = LINE ( 'NONE', #50560, #11294 ) ;
#97729 = CARTESIAN_POINT ( 'NONE',  ( -57.65691505428798536, -23.48783264082477018, -1.443836473390095243 ) ) ;
#97730 = CARTESIAN_POINT ( 'NONE',  ( 5.749347661499963458, 19.61174949527739386, -1.500000000000002220 ) ) ;
#97731 = EDGE_CURVE ( 'NONE', #85265, #44470, #36040, .T. ) ;
#97732 = ORIENTED_EDGE ( 'NONE', *, *, #16817, .T. ) ;
#97733 = DIRECTION ( 'NONE',  ( 0.000000000000000000, 0.000000000000000000, -1.000000000000000000 ) ) ;
#97734 = CARTESIAN_POINT ( 'NONE',  ( 1.949999999999999956, 0.1924999999999999489, 0.1925000000000000322 ) ) ;
#97735 = CARTESIAN_POINT ( 'NONE',  ( -105.5995553614588403, -23.48783264082477018, -1.443836473390094355 ) ) ;
#97736 = FACE_OUTER_BOUND ( 'NONE', #73648, .T. ) ;
#97737 = ORIENTED_EDGE ( 'NONE', *, *, #91797, .F. ) ;
#97738 = CARTESIAN_POINT ( 'NONE',  ( -122.9228709571500389, -23.47593901973090524, -1.443836447538996426 ) ) ;
#97739 = CARTESIAN_POINT ( 'NONE',  ( -27.99827674658315502, -25.26248072559767266, 8.232206008816641329 ) ) ;
#97740 = EDGE_LOOP ( 'NONE', ( #86384, #53003, #8024, #100166 ) ) ;
#97741 = CARTESIAN_POINT ( 'NONE',  ( -2.100290975465340271, -20.70549805216813510, 11.49999999999998934 ) ) ;
#97742 = ORIENTED_EDGE ( 'NONE', *, *, #51787, .T. ) ;
#97743 = CC_DESIGN_DATE_AND_TIME_ASSIGNMENT ( #100273, #843, ( #91265 ) ) ;
#97745 = ORIENTED_EDGE ( 'NONE', *, *, #35696, .F. ) ;
#97744 = CARTESIAN_POINT ( 'NONE',  ( -39.78242746767242721, -25.30509143442804998, 4.885129823892348178 ) ) ;
#97746 = B_SPLINE_SURFACE_WITH_KNOTS ( 'NONE', 3, 1, ( 
 ( #88079, #18553 ),
 ( #80959, #71856 ),
 ( #64261, #56639 ),
 ( #87570, #10949 ),
 ( #49022, #41914 ),
 ( #3357, #83945 ),
 ( #44401, #27676 ),
 ( #12436, #97182 ),
 ( #20054, #89570 ),
 ( #52009, #67244 ),
 ( #67745, #51513 ),
 ( #22027, #58625 ),
 ( #51016, #13927 ),
 ( #45400, #53015 ),
 ( #12928, #97675 ),
 ( #5823, #81952 ),
 ( #5324, #43897 ),
 ( #60633, #35787 ),
 ( #82939, #66258 ) ),
 .UNSPECIFIED., .F., .F., .F.,
 ( 4, 1, 1, 1, 1, 1, 1, 1, 1, 1, 1, 1, 1, 1, 1, 1, 4 ),
 ( 2, 2 ),
 ( 0.000000000000000000, 0.06947546024967000966, 0.1365167976177991127, 0.2007888236092598422, 0.2638296728558247040, 0.3257350229654227269, 0.3872906922152893339, 0.4495092187626021918, 0.5129678195454410172, 0.5762752154930611548, 0.6375801002639256421, 0.6979026059171035135, 0.7571720884269868002, 0.8165985284886555506, 0.8766531708928191335, 0.9372896424102402646, 1.000000000000000000 ),
 ( 0.000000000000000000, 1.000000000000000000 ),
 .UNSPECIFIED. ) ;
#97747 = DIRECTION ( 'NONE',  ( -0.000000000000000000, 1.000000000000000000, -0.000000000000000000 ) ) ;
#97748 = CARTESIAN_POINT ( 'NONE',  ( -52.52287095715006870, -23.48786465467241058, 11.44779295918255002 ) ) ;
#97749 = VERTEX_POINT ( 'NONE', #55401 ) ;
#97750 = ORIENTED_EDGE ( 'NONE', *, *, #74125, .T. ) ;
#97751 = CARTESIAN_POINT ( 'NONE',  ( -79.52287095715006160, -24.65952944569304961, 1.056160979905698794 ) ) ;
#97752 = CARTESIAN_POINT ( 'NONE',  ( -121.2228709571500218, -23.47593901973090524, -1.443836447538996204 ) ) ;
#97753 = CARTESIAN_POINT ( 'NONE',  ( -80.52287095715006160, -25.00158670708909625, 2.256160236439166411 ) ) ;
#97754 = CARTESIAN_POINT ( 'NONE',  ( -71.15736797201716968, -25.24515128636431527, 5.711157537062583778 ) ) ;
#97756 = VERTEX_POINT ( 'NONE', #86340 ) ;
#97755 = CARTESIAN_POINT ( 'NONE',  ( -16.84257673422482426, -14.26466048179180568, 11.49999999999999645 ) ) ;
#97757 = CARTESIAN_POINT ( 'NONE',  ( -108.5134097286098722, -24.51314013834316086, 0.6176544820404235026 ) ) ;
#97758 = AXIS2_PLACEMENT_3D ( 'NONE', #52074, #28230, #83001 ) ;
#97759 = CARTESIAN_POINT ( 'NONE',  ( 18.79633983808273712, -12.56333175589740847, 11.49999999999998934 ) ) ;
#97761 = ORIENTED_EDGE ( 'NONE', *, *, #89344, .T. ) ;
#97760 = CARTESIAN_POINT ( 'NONE',  ( -46.52287095715006160, -23.73934037231757088, 11.05740245334329153 ) ) ;
#97762 = VECTOR ( 'NONE', #36909, 1000.000000000000114 ) ;
#97763 = EDGE_LOOP ( 'NONE', ( #29053, #40977, #57100 ) ) ;
#97764 = CARTESIAN_POINT ( 'NONE',  ( -10.27747606359964117, -6.067502657846070235, 28.80925224784997596 ) ) ;
#97765 = B_SPLINE_CURVE_WITH_KNOTS ( 'NONE', 3,
 ( #34320, #50052, #72389, #95216 ),
 .UNSPECIFIED., .F., .F.,
 ( 4, 4 ),
 ( 0.000000000000000000, 9.999999999998897304E-05 ),
 .UNSPECIFIED. ) ;
#97766 = FACE_OUTER_BOUND ( 'NONE', #80799, .T. ) ;
#97767 = ORIENTED_EDGE ( 'NONE', *, *, #34030, .F. ) ;
#97768 = CYLINDRICAL_SURFACE ( 'NONE', #1682, 3.060000000000000053 ) ;
#97769 = CARTESIAN_POINT ( 'NONE',  ( -21.75032768068154354, -4.810781854073628239, -1.500000000000002220 ) ) ;
#97770 = DIRECTION ( 'NONE',  ( 0.1489078231574191002, -6.845827386180410961E-16, -0.9888510809027407644 ) ) ;
#97771 = ORIENTED_EDGE ( 'NONE', *, *, #22783, .F. ) ;
#97772 = CARTESIAN_POINT ( 'NONE',  ( 1.949999999999999956, -0.1925000000000001155, -0.1925000000000000600 ) ) ;
#97773 = CARTESIAN_POINT ( 'NONE',  ( 0.3000000000000007661, 2.681976490132703452E-15, -21.89999999999999858 ) ) ;
#97774 = LINE ( 'NONE', #84917, #94923 ) ;
#97775 = DIRECTION ( 'NONE',  ( -0.000000000000000000, -0.000000000000000000, -1.000000000000000000 ) ) ;
#97776 = CIRCLE ( 'NONE', #13530, 28.96799999999999287 ) ;
#97777 = CARTESIAN_POINT ( 'NONE',  ( -14.81708852449743929, -12.69844354874750181, 11.49999999999998934 ) ) ;
#97778 = ADVANCED_FACE ( 'NONE', ( #46778 ), #82539, .T. ) ;
#97779 = CARTESIAN_POINT ( 'NONE',  ( 0.5228555243449846124, 21.43159495547403282, -1.500000000000002220 ) ) ;
#97780 = CARTESIAN_POINT ( 'NONE',  ( -1.222978892338334012, -5.876774720514411854, 19.56655654527324373 ) ) ;
#97781 = ADVANCED_FACE ( 'NONE', ( #69620 ), #70113, .F. ) ;
#97782 = DIRECTION ( 'NONE',  ( -1.000000000000000000, -3.773278334444167608E-23, -8.201307833595939069E-29 ) ) ;
#97783 = DIRECTION ( 'NONE',  ( -1.000000000000000000, -3.773278334444166432E-23, -8.201307841325785021E-29 ) ) ;
#97784 = CARTESIAN_POINT ( 'NONE',  ( -17.61067154241388977, 14.45706175128816184, -1.500000000000002220 ) ) ;
#97785 = AXIS2_PLACEMENT_3D ( 'NONE', #9451, #338, #16053 ) ;
#97786 = MECHANICAL_CONTEXT ( 'NONE', #25210, 'mechanical' ) ;
#97787 = DIRECTION ( 'NONE',  ( -0.000000000000000000, -1.000000000000000000, -0.000000000000000000 ) ) ;
#97788 = LINE ( 'NONE', #72977, #578 ) ;
#97789 = CARTESIAN_POINT ( 'NONE',  ( 17.55240489776628721, -9.587225365216566431, 11.49999999999999645 ) ) ;
#97790 = CARTESIAN_POINT ( 'NONE',  ( -104.6266640182791008, -24.34968618360934300, 0.1864209137778872205 ) ) ;
#97791 = VECTOR ( 'NONE', #83291, 1000.000000000000114 ) ;
#97792 = CARTESIAN_POINT ( 'NONE',  ( -39.52202212734117381, -23.48786465467240347, 11.44779295918255002 ) ) ;
#97793 = CARTESIAN_POINT ( 'NONE',  ( -48.62834717164137288, -24.51314013834315375, 0.6176544820404137326 ) ) ;
#97794 = ORIENTED_EDGE ( 'NONE', *, *, #16200, .F. ) ;
#97795 = EDGE_CURVE ( 'NONE', #28755, #33442, #86832, .T. ) ;
#97796 = DIRECTION ( 'NONE',  ( 0.000000000000000000, 0.000000000000000000, -1.000000000000000000 ) ) ;
#97797 = CARTESIAN_POINT ( 'NONE',  ( 8.499999999999989342, 18.74999999999999645, 0.000000000000000000 ) ) ;
#97798 = CARTESIAN_POINT ( 'NONE',  ( 17.51545567653809954, -12.82042131148251229, -1.500000000000002220 ) ) ;
#97799 = FACE_OUTER_BOUND ( 'NONE', #72991, .T. ) ;
#97800 = CARTESIAN_POINT ( 'NONE',  ( -8.292788067677484776, 17.68049324621676632, -1.500000000000002220 ) ) ;
#97801 = DIRECTION ( 'NONE',  ( -3.773278334444166432E-23, 1.000000000000000000, 0.000000000000000000 ) ) ;
#97802 = ORIENTED_EDGE ( 'NONE', *, *, #25519, .T. ) ;
#97803 = CALENDAR_DATE ( 2026, 9, 10 ) ;
#97804 = FACE_OUTER_BOUND ( 'NONE', #9611, .T. ) ;
#97805 = CARTESIAN_POINT ( 'NONE',  ( -110.6228709571500985, -24.83602698348161297, 1.605859176311268399 ) ) ;
#97806 = CARTESIAN_POINT ( 'NONE',  ( 1.124825640313904973, 20.40429917142216354, 11.49999999999999645 ) ) ;
#97807 = DIRECTION ( 'NONE',  ( 0.7071067811865474617, 0.000000000000000000, 0.7071067811865474617 ) ) ;
#97808 = CARTESIAN_POINT ( 'NONE',  ( -93.58953762381671027, -23.48783264082478794, -1.443836473390063713 ) ) ;
#97809 = EDGE_LOOP ( 'NONE', ( #79504, #75081, #28363, #36876 ) ) ;
#97810 = CARTESIAN_POINT ( 'NONE',  ( -51.58953762381673158, -23.47593901973091235, -1.443836447539009749 ) ) ;
#97811 = DIRECTION ( 'NONE',  ( -3.773278334453079030E-23, 0.9999999999976377785, 2.173523156925979128E-06 ) ) ;
#97812 = CARTESIAN_POINT ( 'NONE',  ( -116.5567474348173675, -23.73791477778912551, 11.05961554403170055 ) ) ;
#97813 = APPLICATION_CONTEXT ( 'configuration controlled 3d designs of mechanical parts and assemblies' ) ;
#97814 = CARTESIAN_POINT ( 'NONE',  ( 2.899999999999999023, 33.29999999999999716, 0.000000000000000000 ) ) ;
#97815 = VECTOR ( 'NONE', #68691, 1000.000000000000114 ) ;
#97816 = ORIENTED_EDGE ( 'NONE', *, *, #47305, .T. ) ;
#97817 = CARTESIAN_POINT ( 'NONE',  ( 26.73860345374794534, -1.477225279485574028, -7.113848178280766099 ) ) ;
#97818 = ADVANCED_FACE ( 'NONE', ( #48288 ), #54394, .F. ) ;
#97819 = CARTESIAN_POINT ( 'NONE',  ( -19.18584950847915493, -12.73052202388904952, 11.49999999999999645 ) ) ;
#97820 = CARTESIAN_POINT ( 'NONE',  ( -17.51746294255814718, -14.55262482891283504, 11.49999999999998934 ) ) ;
#97821 = CARTESIAN_POINT ( 'NONE',  ( -110.5222005053990557, -23.48786465467241413, 11.44779295918253581 ) ) ;
#97822 = DIRECTION ( 'NONE',  ( -0.000000000000000000, -0.000000000000000000, 1.000000000000000000 ) ) ;
#97823 = CARTESIAN_POINT ( 'NONE',  ( -120.5228709571500616, -24.99156044556120904, 7.747789690856173195 ) ) ;
#97824 = CARTESIAN_POINT ( 'NONE',  ( -50.58953762381673158, -25.00158670708909625, 2.256160236439164635 ) ) ;
#97825 = CARTESIAN_POINT ( 'NONE',  ( -110.5103941636743485, -25.00158670708910336, 2.256160236439219258 ) ) ;
#97826 = CARTESIAN_POINT ( 'NONE',  ( -9.857428550561325054, -19.57614489166009264, -1.500000000000002220 ) ) ;
#97827 = EDGE_CURVE ( 'NONE', #23628, #2616, #85325, .T. ) ;
#97828 = CARTESIAN_POINT ( 'NONE',  ( 6.467769777575680834, -5.876774720514426953, 21.83821538399986650 ) ) ;
#97829 = CARTESIAN_POINT ( 'NONE',  ( -103.6228709571500559, -24.66019654487199375, 8.947790411086124607 ) ) ;
#97830 = CARTESIAN_POINT ( 'NONE',  ( -71.60138352291718888, -25.29053162850427583, 5.617232799301285162 ) ) ;
#97831 = CARTESIAN_POINT ( 'NONE',  ( -28.62287095715004881, -29.50247984919086264, -1.443849221408822103 ) ) ;
#97832 = EDGE_LOOP ( 'NONE', ( #30751, #88745, #36101, #77119 ) ) ;
#97833 = CARTESIAN_POINT ( 'NONE',  ( 17.38039551199336685, -10.77953091123627694, 11.49999999999998934 ) ) ;
#97834 = ORIENTED_EDGE ( 'NONE', *, *, #46571, .T. ) ;
#97835 = ORIENTED_EDGE ( 'NONE', *, *, #7723, .F. ) ;
#97836 = ORIENTED_EDGE ( 'NONE', *, *, #92370, .T. ) ;
#97837 = ORIENTED_EDGE ( 'NONE', *, *, #44409, .F. ) ;
#97838 = CARTESIAN_POINT ( 'NONE',  ( 1.550618966079767347, 22.99078241098900932, -1.500000000000002220 ) ) ;
#97839 = CARTESIAN_POINT ( 'NONE',  ( -61.58322304524284618, -24.51314013834316441, 0.6176544820404165081 ) ) ;
#97840 = CARTESIAN_POINT ( 'NONE',  ( -9.806399893892750796, 17.69452640759178408, -1.500000000000002220 ) ) ;
#97841 = VERTEX_POINT ( 'NONE', #62506 ) ;
#97842 = PLANE ( 'NONE',  #60685 ) ;
#97843 = CARTESIAN_POINT ( 'NONE',  ( -127.5228709571500616, -24.64965694238408034, 8.947790433994189385 ) ) ;
#97844 = CARTESIAN_POINT ( 'NONE',  ( 29.73860345376319358, 1.682774720514426114, -1.352392034746782823 ) ) ;
#97845 = CARTESIAN_POINT ( 'NONE',  ( -27.83739072329610664, -0.3587747205143967943, -8.084349702057700426 ) ) ;
#97847 = VERTEX_POINT ( 'NONE', #40674 ) ;
#97846 = CARTESIAN_POINT ( 'NONE',  ( -19.74196057798672399, -8.316236533413031040, 11.49999999999999645 ) ) ;
#97848 = CARTESIAN_POINT ( 'NONE',  ( -77.58953762381672448, -23.48783264082478794, -1.443836473390065933 ) ) ;
#97849 = ORIENTED_EDGE ( 'NONE', *, *, #34428, .F. ) ;
#97850 = CARTESIAN_POINT ( 'NONE',  ( 0.6114060112162268412, -22.25658958135186793, -1.500000000000002220 ) ) ;
#97851 = CARTESIAN_POINT ( 'NONE',  ( 19.89799572200132971, -5.707369160466581270, 11.49999999999998934 ) ) ;
#97852 = EDGE_CURVE ( 'NONE', #85757, #41954, #16320, .T. ) ;
#97853 = VERTEX_POINT ( 'NONE', #96451 ) ;
#97854 = CARTESIAN_POINT ( 'NONE',  ( -28.55248484695741595, -23.80080791946256014, -0.6495505116914124244 ) ) ;
#97855 = ORIENTED_EDGE ( 'NONE', *, *, #47073, .T. ) ;
#97856 = DIRECTION ( 'NONE',  ( 0.000000000000000000, 2.173523156925980399E-06, -0.9999999999976378895 ) ) ;
#97857 = VERTEX_POINT ( 'NONE', #58407 ) ;
#97858 = CARTESIAN_POINT ( 'NONE',  ( -3.950822543831816080, -20.53616823614468956, -1.500000000000002220 ) ) ;
#97859 = CARTESIAN_POINT ( 'NONE',  ( -3.478157889954244464, -21.63767827151469447, 11.49999999999999645 ) ) ;
#97860 = CARTESIAN_POINT ( 'NONE',  ( -91.58953762381672448, -24.65952944569304606, 1.056160979905697239 ) ) ;
#97861 = CARTESIAN_POINT ( 'NONE',  ( -12.86601690267178100, 18.50254183665605012, 11.49999999999998934 ) ) ;
#97862 = EDGE_CURVE ( 'NONE', #2525, #79654, #95346, .T. ) ;
#97863 = CARTESIAN_POINT ( 'NONE',  ( 11.42219733811748306, 17.55150860717643724, -1.500000000000002220 ) ) ;
#97864 = DIRECTION ( 'NONE',  ( 0.000000000000000000, -2.173523156925980399E-06, 0.9999999999976378895 ) ) ;
#97865 = CARTESIAN_POINT ( 'NONE',  ( 0.6000000000000007550, 2.939152317953647894E-15, -24.00000000000000000 ) ) ;
#97866 = FACE_OUTER_BOUND ( 'NONE', #78491, .T. ) ;
#97867 = EDGE_LOOP ( 'NONE', ( #37630, #16890, #72333, #34255 ) ) ;
#97868 = EDGE_LOOP ( 'NONE', ( #62247, #66005, #21371, #37577 ) ) ;
#97869 = ORIENTED_EDGE ( 'NONE', *, *, #97852, .F. ) ;
#97870 = CARTESIAN_POINT ( 'NONE',  ( -66.59743583313027671, -23.96119346886880308, -0.6495511937832151306 ) ) ;
#97871 = CARTESIAN_POINT ( 'NONE',  ( -15.31780299886000485, -15.04297462106122474, -1.500000000000002220 ) ) ;
#97872 = CARTESIAN_POINT ( 'NONE',  ( -86.62287095715005592, -24.66019654487199375, 8.947790411086124607 ) ) ;
#97873 = ORIENTED_EDGE ( 'NONE', *, *, #74757, .F. ) ;
#97874 = CARTESIAN_POINT ( 'NONE',  ( -20.97943885474387216, 2.004451313549292735, 11.49999999999998934 ) ) ;
#97875 = CARTESIAN_POINT ( 'NONE',  ( -99.52885836007774856, -25.26978538596253188, 3.946409558071873214 ) ) ;
#97876 = LINE ( 'NONE', #59333, #25242 ) ;
#97877 = CARTESIAN_POINT ( 'NONE',  ( -0.02075734969026423599, 6.376774720514426953, -0.08597719988137648983 ) ) ;
#97878 = CARTESIAN_POINT ( 'NONE',  ( 8.205893897551582938, 3.316774720514426456, -27.11136772256261196 ) ) ;
#97879 = CARTESIAN_POINT ( 'NONE',  ( -1.064504969004270052, -5.876774720514408301, 19.35667676486395905 ) ) ;
#97880 = CARTESIAN_POINT ( 'NONE',  ( -8.904070064990065703, -20.24664451029508783, -1.500000000000002220 ) ) ;
#97881 = EDGE_CURVE ( 'NONE', #75111, #34031, #27451, .T. ) ;
#97882 = CARTESIAN_POINT ( 'NONE',  ( -116.5525168704854195, -24.51314013834316086, 0.6176544820404277214 ) ) ;
#97883 = EDGE_CURVE ( 'NONE', #29958, #85000, #3359, .T. ) ;
#97884 = AXIS2_PLACEMENT_3D ( 'NONE', #20943, #58044, #74731 ) ;
#97885 = CARTESIAN_POINT ( 'NONE',  ( -109.1632612664256357, -25.30553889313048543, 4.924919525099058504 ) ) ;
#97886 = CARTESIAN_POINT ( 'NONE',  ( -99.52287095715011844, -24.33927499327856481, 9.819080762295815390 ) ) ;
#97887 = CARTESIAN_POINT ( 'NONE',  ( -58.58953762381671027, -23.47593901973091235, -1.443836447539007972 ) ) ;
#97888 = AXIS2_PLACEMENT_3D ( 'NONE', #11365, #57060, #42338 ) ;
#97889 = CARTESIAN_POINT ( 'NONE',  ( 1.664315604108443925, 19.36118569274438528, -1.500000000000002220 ) ) ;
#97890 = CARTESIAN_POINT ( 'NONE',  ( 19.59546714036918758, 8.467717511154198462, -1.500000000000002220 ) ) ;
#97891 = FACE_OUTER_BOUND ( 'NONE', #60673, .T. ) ;
#97892 = CARTESIAN_POINT ( 'NONE',  ( -51.94981768477178008, -25.25978491487771649, 3.590542621692356384 ) ) ;
#97893 = EDGE_CURVE ( 'NONE', #13741, #44036, #51677, .T. ) ;
#97894 = DIRECTION ( 'NONE',  ( -3.773278334444166432E-23, 1.000000000000000000, 0.000000000000000000 ) ) ;
#97895 = CARTESIAN_POINT ( 'NONE',  ( -70.74026866089612042, -25.30511070033976395, 4.894904393956083233 ) ) ;
#97896 = CARTESIAN_POINT ( 'NONE',  ( 17.73637878876437668, -14.10177982315242318, -1.500000000000002220 ) ) ;
#97897 = EDGE_CURVE ( 'NONE', #2798, #64622, #69693, .T. ) ;
#97898 = ORIENTED_EDGE ( 'NONE', *, *, #66394, .T. ) ;
#97899 = FACE_OUTER_BOUND ( 'NONE', #18198, .T. ) ;
#97900 = CARTESIAN_POINT ( 'NONE',  ( -79.59586967038401895, -23.96119346886880308, -0.6495511937832122440 ) ) ;
#97901 = CARTESIAN_POINT ( 'NONE',  ( 5.037983044326730386, -19.10262670698400100, 11.49999999999999645 ) ) ;
#97902 = CARTESIAN_POINT ( 'NONE',  ( -50.52287095715006160, -29.50247984919015209, -1.443849546365058689 ) ) ;
#97903 = PLANE ( 'NONE',  #82973 ) ;
#97904 = VERTEX_POINT ( 'NONE', #10218 ) ;
#97905 = EDGE_CURVE ( 'NONE', #77370, #13904, #16623, .T. ) ;
#97906 = CARTESIAN_POINT ( 'NONE',  ( -59.52287095715006160, -24.64898659630528854, 1.056161002820822592 ) ) ;
#97907 = DIRECTION ( 'NONE',  ( -1.000000000000000000, -3.773278334444167608E-23, -8.201307833595939069E-29 ) ) ;
#97908 = CARTESIAN_POINT ( 'NONE',  ( -100.8583591130402937, -25.12268552722101944, 7.041620770524536610 ) ) ;
#97909 = CARTESIAN_POINT ( 'NONE',  ( -16.54959454218438708, 13.92943311328891554, -1.500000000000002220 ) ) ;
#97910 = CARTESIAN_POINT ( 'NONE',  ( -49.19632817692706084, -25.10935285274896245, 3.560434298826884447 ) ) ;
#97911 = CARTESIAN_POINT ( 'NONE',  ( -15.38109395195050233, 11.78095549196778258, -1.500000000000002220 ) ) ;
#97912 = ADVANCED_FACE ( 'NONE', ( #57910 ), #43178, .F. ) ;
#97913 = CARTESIAN_POINT ( 'NONE',  ( -34.52287095715006160, -29.50250243563736774, 8.947779886222150481 ) ) ;
#97914 = PLANE ( 'NONE',  #47460 ) ;
#97915 = CARTESIAN_POINT ( 'NONE',  ( 14.04693994163893578, -13.95676237773968609, 11.49999999999998934 ) ) ;
#97916 = ORIENTED_EDGE ( 'NONE', *, *, #91235, .F. ) ;
#97917 = CARTESIAN_POINT ( 'NONE',  ( 5.465678960246475704, -19.50585317057041124, 11.49999999999999645 ) ) ;
#97918 = CARTESIAN_POINT ( 'NONE',  ( -0.1456595461938881009, 0.5911710074084819411, -2.677392948487098267E-15 ) ) ;
#97919 = CARTESIAN_POINT ( 'NONE',  ( -7.749999999999996447, 23.99999999999999289, 2.100000000000000089 ) ) ;
#97920 = VERTEX_POINT ( 'NONE', #74118 ) ;
#97921 = B_SPLINE_SURFACE_WITH_KNOTS ( 'NONE', 3, 3, ( 
 ( #70109, #21413, #38146, #91941 ),
 ( #61509, #92434, #23407, #84824 ),
 ( #52390, #83326, #6702, #13806 ),
 ( #99040, #44781, #68119, #91431 ),
 ( #54392, #46270, #69099, #99535 ),
 ( #69615, #97, #76206, #62002 ),
 ( #85321, #6204, #52890, #15812 ),
 ( #83829, #37656, #30032, #61007 ),
 ( #22411, #53394, #84322, #14804 ),
 ( #45771, #55398, #73486, #93939 ) ),
 .UNSPECIFIED., .F., .F., .F.,
 ( 4, 3, 3, 4 ),
 ( 4, 4 ),
 ( 0.7022005934544807149, 0.7765311282028797280, 0.8508616629512786300, 0.9995227324480766562 ),
 ( 0.8495965314205278229, 0.8511156036249712953 ),
 .UNSPECIFIED. ) ;
#97922 = CARTESIAN_POINT ( 'NONE',  ( -88.88918693012689687, -29.50249591506787894, 5.947779886229223045 ) ) ;
#97923 = DIRECTION ( 'NONE',  ( -3.773278334453079618E-23, 0.9999999999976377785, 2.173523156925979552E-06 ) ) ;
#97924 = CARTESIAN_POINT ( 'NONE',  ( -10.79305683637731228, -0.3587747205144057872, -27.49869550653261285 ) ) ;
#97925 = CARTESIAN_POINT ( 'NONE',  ( -6.499999999999992895, 0.000000000000000000, 0.000000000000000000 ) ) ;
#97926 = LINE ( 'NONE', #13690, #98128 ) ;
#97927 = CARTESIAN_POINT ( 'NONE',  ( 7.329891291799937925, -18.66831812819665970, 11.49999999999998934 ) ) ;
#97928 = CARTESIAN_POINT ( 'NONE',  ( -51.52287095715006870, -23.47596703998600631, 11.44779298504229104 ) ) ;
#97929 = VERTEX_POINT ( 'NONE', #97451 ) ;
#97930 = CARTESIAN_POINT ( 'NONE',  ( -41.26959558397305727, -25.07899898050004950, 7.338714981574760543 ) ) ;
#97931 = B_SPLINE_CURVE_WITH_KNOTS ( 'NONE', 3,
 ( #94705, #40923, #94196, #71884, #25693, #24682 ),
 .UNSPECIFIED., .F., .F.,
 ( 4, 2, 4 ),
 ( 6.396512625966562883E-06, 0.001387752252890995597, 0.002769107993156024686 ),
 .UNSPECIFIED. ) ;
#97932 = CARTESIAN_POINT ( 'NONE',  ( 8.071512145086529699, -9.528487854913505473, 6.500000000000001776 ) ) ;
#97933 = CARTESIAN_POINT ( 'NONE',  ( -11.64875734969026233, 5.965225279485572685, 31.02402280011862246 ) ) ;
#97934 = CARTESIAN_POINT ( 'NONE',  ( -89.55620429048339304, -23.47593901973091235, -1.443836447539002865 ) ) ;
#97935 = VECTOR ( 'NONE', #62898, 1000.000000000000000 ) ;
#97936 = CARTESIAN_POINT ( 'NONE',  ( -118.6228709571500701, -23.96177878511309345, 10.65340807706328974 ) ) ;
#97937 = EDGE_CURVE ( 'NONE', #32607, #27420, #66537, .T. ) ;
#97938 = CARTESIAN_POINT ( 'NONE',  ( -14.39434090420295220, 17.20869321163716492, 11.49999999999999645 ) ) ;
#97939 = CARTESIAN_POINT ( 'NONE',  ( -101.9714687704791487, -25.03707831087709934, 7.590867751134624086 ) ) ;
#97940 = ORIENTED_EDGE ( 'NONE', *, *, #29992, .T. ) ;
#97941 = CARTESIAN_POINT ( 'NONE',  ( 20.34676669208793953, -0.1217515720461415790, 11.49999999999998934 ) ) ;
#97942 = ORIENTED_EDGE ( 'NONE', *, *, #84082, .T. ) ;
#97943 = CARTESIAN_POINT ( 'NONE',  ( 6.461317529299694051, 22.01590093704556850, -1.500000000000002220 ) ) ;
#97944 = DIRECTION ( 'NONE',  ( 1.000000000000000000, -0.000000000000000000, -0.000000000000000000 ) ) ;
#97945 = AXIS2_PLACEMENT_3D ( 'NONE', #59807, #75497, #21214 ) ;
#97946 = ORIENTED_EDGE ( 'NONE', *, *, #78393, .T. ) ;
#97947 = CARTESIAN_POINT ( 'NONE',  ( -49.65594356225680173, -25.30517875835296593, 4.891185000421574891 ) ) ;
#97948 = CARTESIAN_POINT ( 'NONE',  ( -77.55620429048342146, -24.64965694238574656, 8.947790433994196491 ) ) ;
#97949 = CARTESIAN_POINT ( 'NONE',  ( 3.794707603699265519E-15, -6.376774720514426953, 17.50000000000000000 ) ) ;
#97951 = ORIENTED_EDGE ( 'NONE', *, *, #70853, .T. ) ;
#97950 = CARTESIAN_POINT ( 'NONE',  ( -10.94853654022341516, 18.13385389444049522, 11.49999999999999645 ) ) ;
#97952 = ORIENTED_EDGE ( 'NONE', *, *, #74861, .F. ) ;
#97953 = CARTESIAN_POINT ( 'NONE',  ( -21.91774099701738621, 3.392077650570975766, 11.49999999999998934 ) ) ;
#97954 = CARTESIAN_POINT ( 'NONE',  ( -3.210669876418242197, 20.33209092710186638, -1.500000000000002220 ) ) ;
#97955 = EDGE_CURVE ( 'NONE', #67776, #63299, #71094, .T. ) ;
#97956 = ORIENTED_EDGE ( 'NONE', *, *, #34194, .F. ) ;
#97957 = ORIENTED_EDGE ( 'NONE', *, *, #57037, .F. ) ;
#97958 = CARTESIAN_POINT ( 'NONE',  ( 32.53346577320679245, -0.6027747205144262654, -11.93731717363830747 ) ) ;
#97959 = CARTESIAN_POINT ( 'NONE',  ( -77.62287095715005592, -23.47593901973091235, -1.443836447539004642 ) ) ;
#97960 = ORIENTED_EDGE ( 'NONE', *, *, #42796, .F. ) ;
#97961 = ORIENTED_EDGE ( 'NONE', *, *, #6288, .F. ) ;
#97962 = ORIENTED_EDGE ( 'NONE', *, *, #68126, .T. ) ;
#97963 = FACE_BOUND ( 'NONE', #30362, .T. ) ;
#97964 = CARTESIAN_POINT ( 'NONE',  ( -28.57980741741397068, -24.35756971646765479, 9.386484685950513551 ) ) ;
#97965 = CARTESIAN_POINT ( 'NONE',  ( 14.58759568486751235, -3.520387117353680484, -28.38990263572715733 ) ) ;
#97966 = CARTESIAN_POINT ( 'NONE',  ( -2.730994233912177549, 20.60462238790213618, -1.500000000000002220 ) ) ;
#97967 = CARTESIAN_POINT ( 'NONE',  ( 17.51545567653809954, -12.82042131148251229, 11.49999999999999645 ) ) ;
#97968 = ORIENTED_EDGE ( 'NONE', *, *, #7498, .F. ) ;
#97969 = CARTESIAN_POINT ( 'NONE',  ( -100.8391834046851159, -25.19504552050077706, 3.366519573641078011 ) ) ;
#97970 = DIRECTION ( 'NONE',  ( -3.773278334453079618E-23, 0.9999999999976377785, 2.173523156925979975E-06 ) ) ;
#97971 = CARTESIAN_POINT ( 'NONE',  ( -115.5161532992356967, -24.52300882791528380, 0.6510814631126371488 ) ) ;
#97972 = CARTESIAN_POINT ( 'NONE',  ( -13.02831144489870319, 18.26546089674541307, 11.49999999999998934 ) ) ;
#97973 = EDGE_CURVE ( 'NONE', #23684, #82501, #39630, .T. ) ;
#97974 = ADVANCED_FACE ( 'NONE', ( #56911 ), #18820, .T. ) ;
#97975 = CARTESIAN_POINT ( 'NONE',  ( 32.90495245295455362, -3.622774720514437607, -13.06061886496134861 ) ) ;
#97976 = CARTESIAN_POINT ( 'NONE',  ( -124.5228709571501042, -24.51387760970726504, 9.387446482453404073 ) ) ;
#97977 = ORIENTED_EDGE ( 'NONE', *, *, #84803, .T. ) ;
#97978 = CARTESIAN_POINT ( 'NONE',  ( -71.63953589603883643, -25.29442214193731076, 5.728881397446647483 ) ) ;
#97979 = CARTESIAN_POINT ( 'NONE',  ( -129.5895376238167387, -24.64898659630367916, 1.056161002820393602 ) ) ;
#97980 = ADVANCED_FACE ( 'NONE', ( #73126 ), #58226, .T. ) ;
#97981 = CIRCLE ( 'NONE', #54271, 129.7684398600581517 ) ;
#97982 = EDGE_LOOP ( 'NONE', ( #71405, #94646, #19282, #89638 ) ) ;
#97983 = ORIENTED_EDGE ( 'NONE', *, *, #95655, .T. ) ;
#97984 = LINE ( 'NONE', #91378, #83077 ) ;
#97985 = ORIENTED_EDGE ( 'NONE', *, *, #24513, .T. ) ;
#97986 = CARTESIAN_POINT ( 'NONE',  ( -12.29646723538143505, -17.35194501319736560, -1.500000000000002220 ) ) ;
#97987 = ORIENTED_EDGE ( 'NONE', *, *, #17962, .T. ) ;
#97988 = CARTESIAN_POINT ( 'NONE',  ( 0.000000000000000000, 1.477225279485574028, 19.84760796525321425 ) ) ;
#97989 = CARTESIAN_POINT ( 'NONE',  ( 9.711643268838683341, -19.58466107313252635, -1.500000000000002220 ) ) ;
#97990 = FACE_OUTER_BOUND ( 'NONE', #30561, .T. ) ;
#97991 = CARTESIAN_POINT ( 'NONE',  ( -2.919094682108430483, 22.50186656173435296, -1.500000000000002220 ) ) ;
#97992 = CARTESIAN_POINT ( 'NONE',  ( -40.65892442973913745, -25.18430874473797942, 3.308410199191338386 ) ) ;
#97993 = PLANE ( 'NONE',  #44911 ) ;
#97994 = CARTESIAN_POINT ( 'NONE',  ( 15.04091035147580335, -15.99806323810862274, -1.500000000000002220 ) ) ;
#97995 = CARTESIAN_POINT ( 'NONE',  ( -39.52287095715005449, -23.96127896941631619, -0.6493128931038099072 ) ) ;
#97996 = VERTEX_POINT ( 'NONE', #97930 ) ;
#97997 = DIRECTION ( 'NONE',  ( -0.000000000000000000, 1.000000000000000000, -0.000000000000000000 ) ) ;
#97998 = ADVANCED_FACE ( 'NONE', ( #29930 ), #37550, .T. ) ;
#97999 = EDGE_LOOP ( 'NONE', ( #81035, #95263, #29717, #88180 ) ) ;
#98000 = DIRECTION ( 'NONE',  ( -3.773278334453080206E-23, 0.9999999999976377785, 2.173523156925979975E-06 ) ) ;
#98001 = LINE ( 'NONE', #84281, #6801 ) ;
#98002 = PLANE ( 'NONE',  #65941 ) ;
#98003 = CARTESIAN_POINT ( 'NONE',  ( -18.72683625574626376, -10.08736549105613278, 11.49999999999998934 ) ) ;
#98004 = CARTESIAN_POINT ( 'NONE',  ( -112.6245392106819452, -24.51314013834317151, 0.6176544820404282765 ) ) ;
#98005 = DIRECTION ( 'NONE',  ( -1.000000000000000000, -8.334928612639484546E-17, 0.000000000000000000 ) ) ;
#98006 = VECTOR ( 'NONE', #13195, 1000.000000000000114 ) ;
#98007 = EDGE_CURVE ( 'NONE', #39472, #70078, #29125, .T. ) ;
#98008 = CARTESIAN_POINT ( 'NONE',  ( -85.54470288293350677, -24.63355581998384736, 0.9682620441943965428 ) ) ;
#98009 = CARTESIAN_POINT ( 'NONE',  ( -85.62287095715011276, -24.82576562982393042, 8.398263435472971494 ) ) ;
#98010 = EDGE_CURVE ( 'NONE', #89989, #61715, #67502, .T. ) ;
#98011 = CARTESIAN_POINT ( 'NONE',  ( -29.49875734969025842, 5.965225279485572685, 15.62202280011862321 ) ) ;
#98012 = ORIENTED_EDGE ( 'NONE', *, *, #10133, .F. ) ;
#98013 = CARTESIAN_POINT ( 'NONE',  ( 12.76379665850700640, 14.79237594083867080, 11.49999999999999645 ) ) ;
#98014 = CARTESIAN_POINT ( 'NONE',  ( -109.3584176993576591, -25.27948031066536672, 4.206202526585778756 ) ) ;
#98015 = DIRECTION ( 'NONE',  ( -0.000000000000000000, 1.000000000000000000, -0.000000000000000000 ) ) ;
#98016 = EDGE_LOOP ( 'NONE', ( #99813, #95602, #416, #8983 ) ) ;
#98017 = ADVANCED_FACE ( 'NONE', ( #74604 ), #82220, .F. ) ;
#98018 = AXIS2_PLACEMENT_3D ( 'NONE', #9019, #33351, #70933 ) ;
#98019 = CARTESIAN_POINT ( 'NONE',  ( -97.52287095715006160, -24.65952944569304606, 1.056160979905702346 ) ) ;
#98020 = DIRECTION ( 'NONE',  ( 0.000000000000000000, 0.000000000000000000, 1.000000000000000000 ) ) ;
#98021 = VECTOR ( 'NONE', #85480, 1000.000000000000000 ) ;
#98023 = EDGE_CURVE ( 'NONE', #79287, #100338, #38363, .T. ) ;
#98022 = CARTESIAN_POINT ( 'NONE',  ( -63.52287095715006160, -23.47596703998600631, 11.44779298504228926 ) ) ;
#98024 = CARTESIAN_POINT ( 'NONE',  ( -106.5228709571500900, -24.34917612406837151, 0.1852690917426598749 ) ) ;
#98025 = CARTESIAN_POINT ( 'NONE',  ( -6.535591236171724105, 18.61618873491671877, 11.49999999999998934 ) ) ;
#98026 = EDGE_CURVE ( 'NONE', #35495, #63790, #36543, .T. ) ;
#98027 = ORIENTED_EDGE ( 'NONE', *, *, #13025, .F. ) ;
#98028 = CARTESIAN_POINT ( 'NONE',  ( 10.46399479596578175, 3.400839389856524342, -27.03001098546515735 ) ) ;
#98029 = CARTESIAN_POINT ( 'NONE',  ( -1.164890887384984586, 4.028272616778474813, 3.549999999999996714 ) ) ;
#98031 = EDGE_CURVE ( 'NONE', #9929, #87827, #98928, .T. ) ;
#98030 = PERSON_AND_ORGANIZATION ( #70597, #27821 ) ;
#98032 = B_SPLINE_CURVE_WITH_KNOTS ( 'NONE', 3,
 ( #94294, #70976, #54256, #8065, #78057, #62881, #7566, #79069, #69964, #32912 ),
 .UNSPECIFIED., .F., .F.,
 ( 4, 2, 2, 2, 4 ),
 ( 0.000000000000000000, 0.2500000000000000000, 0.5000000000000000000, 0.7500000000000000000, 1.000000000000000000 ),
 .UNSPECIFIED. ) ;
#98033 = VERTEX_POINT ( 'NONE', #32943 ) ;
#98034 = CARTESIAN_POINT ( 'NONE',  ( 9.045337356650573923, -0.9026027323331682339, 3.697389739420775090 ) ) ;
#98035 = CARTESIAN_POINT ( 'NONE',  ( -69.55620429048339304, -24.66019654487199020, 8.947790411086131712 ) ) ;
#98036 = CARTESIAN_POINT ( 'NONE',  ( -105.2228709571501213, -23.47593901973090524, -1.443836447538997092 ) ) ;
#98037 = CARTESIAN_POINT ( 'NONE',  ( -118.6289494624385696, -23.48783264082477018, -1.443836473390085695 ) ) ;
#98038 = DIRECTION ( 'NONE',  ( 3.773278334444166432E-23, -1.000000000000000000, 0.000000000000000000 ) ) ;
#98039 = DIRECTION ( 'NONE',  ( 0.000000000000000000, 0.9999999999976377785, 2.173523156925979128E-06 ) ) ;
#98040 = B_SPLINE_CURVE_WITH_KNOTS ( 'NONE', 3,
 ( #32742, #63725, #25634, #87539, #48985, #79915 ),
 .UNSPECIFIED., .F., .F.,
 ( 4, 2, 4 ),
 ( 0.000000000000000000, 0.001380901958385392448, 0.002761803916770784895 ),
 .UNSPECIFIED. ) ;
#98041 = CARTESIAN_POINT ( 'NONE',  ( -107.5199659751638706, -23.73766607897672642, -1.055555164236427590 ) ) ;
#98042 = CARTESIAN_POINT ( 'NONE',  ( 0.05828707793547563409, -19.95834144014285272, 11.49999999999998934 ) ) ;
#98043 = DIRECTION ( 'NONE',  ( -6.938893903907241788E-15, 0.000000000000000000, 1.000000000000000000 ) ) ;
#98044 = CARTESIAN_POINT ( 'NONE',  ( -0.01870951811792301994, -22.80779058525763148, 2.574493158953922389 ) ) ;
#98045 = ORIENTED_EDGE ( 'NONE', *, *, #17346, .T. ) ;
#98046 = CARTESIAN_POINT ( 'NONE',  ( -128.5562042904834072, -23.48786465467241413, 11.44779295918253226 ) ) ;
#98047 = FACE_OUTER_BOUND ( 'NONE', #83025, .T. ) ;
#98048 = CARTESIAN_POINT ( 'NONE',  ( -119.5547944261018074, -24.15543982623907837, -0.2315651400026547124 ) ) ;
#98049 = VECTOR ( 'NONE', #95445, 1000.000000000000114 ) ;
#98050 = DIRECTION ( 'NONE',  ( 1.000000000000000000, 0.000000000000000000, 0.000000000000000000 ) ) ;
#98051 = DIRECTION ( 'NONE',  ( -3.773278334453079030E-23, 0.9999999999976377785, 2.173523156925979128E-06 ) ) ;
#98052 = CARTESIAN_POINT ( 'NONE',  ( -39.64153697460106685, -24.15543982623906416, -0.2315651400026677575 ) ) ;
#98053 = CARTESIAN_POINT ( 'NONE',  ( 14.76093561896379214, -5.965225279485572685, -27.88148769130088667 ) ) ;
#98054 = CARTESIAN_POINT ( 'NONE',  ( -51.44554956638231147, -25.26280043022318367, 4.646412833070179715 ) ) ;
#98055 = ORIENTED_EDGE ( 'NONE', *, *, #64696, .T. ) ;
#98056 = LINE ( 'NONE', #91950, #46274 ) ;
#98057 = CARTESIAN_POINT ( 'NONE',  ( 5.994920710892026605, -6.376774720514429617, 21.76186867112717138 ) ) ;
#98058 = ORIENTED_EDGE ( 'NONE', *, *, #81577, .F. ) ;
#98059 = CARTESIAN_POINT ( 'NONE',  ( -0.9278407348523283193, 20.21260682001012654, -1.500000000000002220 ) ) ;
#98060 = CARTESIAN_POINT ( 'NONE',  ( -69.59881849519349828, -25.31566999480822489, 5.022752278581846141 ) ) ;
#98061 = CARTESIAN_POINT ( 'NONE',  ( 14.83405752585509596, 4.881907540129173384, -27.54622755360215791 ) ) ;
#98062 = CYLINDRICAL_SURFACE ( 'NONE', #49252, 2.249999999999998668 ) ;
#98063 = VERTEX_POINT ( 'NONE', #87940 ) ;
#98064 = CARTESIAN_POINT ( 'NONE',  ( -79.06555067710175422, -25.31161594763374012, 5.326296773346069102 ) ) ;
#98065 = DIRECTION ( 'NONE',  ( 0.000000000000000000, -2.173523156925979552E-06, 0.9999999999976378895 ) ) ;
#98066 = CARTESIAN_POINT ( 'NONE',  ( -10.05502934987021391, 17.38067806581081598, -1.500000000000002220 ) ) ;
#98067 = CARTESIAN_POINT ( 'NONE',  ( -13.78326148797977169, 15.88460234914768421, 11.49999999999999645 ) ) ;
#98068 = CARTESIAN_POINT ( 'NONE',  ( -27.75915168180601000, -24.81617282942779923, 7.602034626381156457 ) ) ;
#98069 = CARTESIAN_POINT ( 'NONE',  ( -70.65896739798220949, -23.48786465467241058, 11.44779295918254824 ) ) ;
#98070 = CARTESIAN_POINT ( 'NONE',  ( -22.07534667767119174, -0.2742745133902674826, -1.500000000000002220 ) ) ;
#98071 = VECTOR ( 'NONE', #80457, 1000.000000000000114 ) ;
#98072 = LINE ( 'NONE', #90975, #70578 ) ;
#98073 = EDGE_CURVE ( 'NONE', #91284, #78758, #77097, .T. ) ;
#98074 = DIRECTION ( 'NONE',  ( -0.000000000000000000, 1.000000000000000000, -0.000000000000000000 ) ) ;
#98075 = CARTESIAN_POINT ( 'NONE',  ( -6.660000000000001030, 0.000000000000000000, 2.399999999999999911 ) ) ;
#98076 = VERTEX_POINT ( 'NONE', #40560 ) ;
#98077 = CARTESIAN_POINT ( 'NONE',  ( -35.52287095715006870, -23.48786465467240347, 11.44779295918255180 ) ) ;
#98078 = CARTESIAN_POINT ( 'NONE',  ( -31.66883481474841489, -23.48783264082477018, -1.443836473390079256 ) ) ;
#98079 = EDGE_CURVE ( 'NONE', #22811, #82785, #52933, .T. ) ;
#98080 = ORIENTED_EDGE ( 'NONE', *, *, #24132, .F. ) ;
#98081 = ORIENTED_EDGE ( 'NONE', *, *, #88211, .T. ) ;
#98082 = DIRECTION ( 'NONE',  ( 0.000000000000000000, 0.000000000000000000, -1.000000000000000000 ) ) ;
#98083 = CARTESIAN_POINT ( 'NONE',  ( -93.52287095715006160, -24.66019654487200086, 8.947790411086110396 ) ) ;
#98084 = DIRECTION ( 'NONE',  ( 0.000000000000000000, 0.000000000000000000, 1.000000000000000000 ) ) ;
#98085 = CARTESIAN_POINT ( 'NONE',  ( -6.273408026305254737, 19.60348359158234288, -1.500000000000002220 ) ) ;
#98086 = VECTOR ( 'NONE', #42861, 1000.000000000000000 ) ;
#98087 = EDGE_CURVE ( 'NONE', #72503, #5107, #29921, .T. ) ;
#98088 = CARTESIAN_POINT ( 'NONE',  ( 11.68953838083566588, 18.09531432177502808, 11.49999999999999645 ) ) ;
#98089 = ORIENTED_EDGE ( 'NONE', *, *, #23752, .F. ) ;
#98090 = CARTESIAN_POINT ( 'NONE',  ( -50.33521035800622201, -25.13337234701628020, 7.100306106499248315 ) ) ;
#98091 = CARTESIAN_POINT ( 'NONE',  ( -99.12380231474227799, -25.26431306044052150, 4.001575155705512366 ) ) ;
#98092 = DIRECTION ( 'NONE',  ( 0.000000000000000000, 0.000000000000000000, -1.000000000000000000 ) ) ;
#98093 = CARTESIAN_POINT ( 'NONE',  ( 3.003370282714790562, 22.13870467353671856, 11.49999999999998934 ) ) ;
#98094 = ADVANCED_FACE ( 'NONE', ( #8099 ), #71010, .F. ) ;
#98095 = CIRCLE ( 'NONE', #5758, 1.999999999999963141 ) ;
#98096 = EDGE_CURVE ( 'NONE', #67044, #67306, #38831, .T. ) ;
#98097 = DIRECTION ( 'NONE',  ( -0.000000000000000000, -1.000000000000000000, -0.000000000000000000 ) ) ;
#98098 = CARTESIAN_POINT ( 'NONE',  ( -82.55620429048339304, -23.47593901973091235, -1.443836447539004642 ) ) ;
#98099 = ORIENTED_EDGE ( 'NONE', *, *, #49029, .T. ) ;
#98100 = CARTESIAN_POINT ( 'NONE',  ( -29.49875734969026198, 0.3587747205144262708, 0.1180228001186258285 ) ) ;
#98101 = CARTESIAN_POINT ( 'NONE',  ( 31.18725089179298138, 4.540774720514433760, 2.579558749741450718 ) ) ;
#98102 = EDGE_CURVE ( 'NONE', #43485, #43478, #15207, .T. ) ;
#98103 = CARTESIAN_POINT ( 'NONE',  ( -5.628781154649386664, 20.11113626451368219, 11.49999999999998934 ) ) ;
#98104 = ORIENTED_EDGE ( 'NONE', *, *, #60446, .F. ) ;
#98106 = ORIENTED_EDGE ( 'NONE', *, *, #36713, .T. ) ;
#98105 = CARTESIAN_POINT ( 'NONE',  ( -40.43756433397305727, -25.11033443737753501, 2.832404817301930056 ) ) ;
#98107 = ORIENTED_EDGE ( 'NONE', *, *, #10912, .T. ) ;
#98108 = CARTESIAN_POINT ( 'NONE',  ( -100.5484574693091986, -24.63419186844611275, 9.035850630976915099 ) ) ;
#98109 = CARTESIAN_POINT ( 'NONE',  ( 7.532573551308565207, 19.69859070278346991, -1.500000000000002220 ) ) ;
#98110 = ORIENTED_EDGE ( 'NONE', *, *, #94198, .T. ) ;
#98111 = CARTESIAN_POINT ( 'NONE',  ( -0.02075734969026423599, -5.965225279485572685, -0.08597719988137648983 ) ) ;
#98112 = CARTESIAN_POINT ( 'NONE',  ( -102.6228709571500559, -24.64965695001469115, 8.947790433994178727 ) ) ;
#98113 = CARTESIAN_POINT ( 'NONE',  ( -108.5228709571500616, -29.50250786944525672, 11.44777988621622988 ) ) ;
#98114 = CARTESIAN_POINT ( 'NONE',  ( -76.63418645068684043, -24.15620529776628089, 10.23563542870660470 ) ) ;
#98115 = CARTESIAN_POINT ( 'NONE',  ( -50.06411376349647924, -25.11622845616857802, 2.865105794236846748 ) ) ;
#98116 = CARTESIAN_POINT ( 'NONE',  ( -21.42251255223715134, 3.917230396363152067, -1.500000000000002220 ) ) ;
#98117 = CARTESIAN_POINT ( 'NONE',  ( -72.52287095715007581, -29.50250243563736774, 8.947779886222143375 ) ) ;
#98119 = ORIENTED_EDGE ( 'NONE', *, *, #45259, .F. ) ;
#98118 = CARTESIAN_POINT ( 'NONE',  ( -21.40455707349245529, -6.346402434563959361, 11.49999999999999645 ) ) ;
#98120 = CARTESIAN_POINT ( 'NONE',  ( -116.5228709571501042, -23.47593901973090524, -1.443836447538996426 ) ) ;
#98121 = DIRECTION ( 'NONE',  ( -0.000000000000000000, 1.000000000000000000, 0.000000000000000000 ) ) ;
#98122 = EDGE_CURVE ( 'NONE', #12874, #93569, #54107, .T. ) ;
#98123 = DIRECTION ( 'NONE',  ( -0.000000000000000000, -1.000000000000000000, -0.000000000000000000 ) ) ;
#98124 = ORIENTED_EDGE ( 'NONE', *, *, #26435, .F. ) ;
#98125 = ORIENTED_EDGE ( 'NONE', *, *, #65166, .F. ) ;
#98126 = EDGE_CURVE ( 'NONE', #81255, #99009, #45652, .T. ) ;
#98127 = VERTEX_POINT ( 'NONE', #46672 ) ;
#98128 = VECTOR ( 'NONE', #82214, 1000.000000000000114 ) ;
#98129 = CARTESIAN_POINT ( 'NONE',  ( -0.6703829557040269504, 4.102177322343282917, -2.677392948487098267E-15 ) ) ;
#98130 = CARTESIAN_POINT ( 'NONE',  ( -2.899999999999996803, 31.80000000000000071, 2.100000000000000089 ) ) ;
#98131 = CARTESIAN_POINT ( 'NONE',  ( 30.64109438017208120, -3.316774720514426456, 28.31981406664616330 ) ) ;
#98132 = EDGE_CURVE ( 'NONE', #94223, #33873, #77079, .T. ) ;
#98133 = CARTESIAN_POINT ( 'NONE',  ( -47.62287095715004881, -29.50250243563736774, 8.947779886222146928 ) ) ;
#98134 = FACE_OUTER_BOUND ( 'NONE', #38693, .T. ) ;
#98135 = CARTESIAN_POINT ( 'NONE',  ( -86.52287095715006160, -29.50250243563736774, 8.947779886222139822 ) ) ;
#98136 = ORIENTED_EDGE ( 'NONE', *, *, #51787, .F. ) ;
#98137 = CARTESIAN_POINT ( 'NONE',  ( -9.862393454161701101, 16.67994275214481092, 11.49999999999999645 ) ) ;
#98138 = CARTESIAN_POINT ( 'NONE',  ( 7.160000000000000142, 10.80195425911416507, -0.9450485415980990345 ) ) ;
#98139 = ORIENTED_EDGE ( 'NONE', *, *, #78839, .F. ) ;
#98140 = CARTESIAN_POINT ( 'NONE',  ( 3.296033061219842519, -6.376774720514406525, 18.71226942120119574 ) ) ;
#98141 = CARTESIAN_POINT ( 'NONE',  ( 7.227401621296005274, 3.316774720515020203, -27.22638491047315767 ) ) ;
#98142 = CARTESIAN_POINT ( 'NONE',  ( -116.5228709571500616, -24.64898659630368627, 1.056161002820833028 ) ) ;
#98144 = EDGE_CURVE ( 'NONE', #44615, #66922, #12923, .T. ) ;
#98143 = DIRECTION ( 'NONE',  ( 3.773278334444167608E-23, -1.000000000000000000, 0.000000000000000000 ) ) ;
#98145 = CARTESIAN_POINT ( 'NONE',  ( 15.22544387773384500, -12.34335808662847178, -1.500000000000002220 ) ) ;
#98146 = CARTESIAN_POINT ( 'NONE',  ( -37.52287095715006870, -24.64898659630367206, 1.056161002820819261 ) ) ;
#98147 = VERTEX_POINT ( 'NONE', #19691 ) ;
#98148 = CARTESIAN_POINT ( 'NONE',  ( -20.03152041342270806, -8.007337437543776915, 11.49999999999998934 ) ) ;
#98149 = CARTESIAN_POINT ( 'NONE',  ( -33.62922567200806867, -24.51419770103157347, 9.386484678747185839 ) ) ;
#98150 = CARTESIAN_POINT ( 'NONE',  ( -96.55620429048337883, -23.48783264082478439, -1.443836473390062380 ) ) ;
#98151 = CARTESIAN_POINT ( 'NONE',  ( -81.55620429048336462, -24.64965694238574301, 8.947790433994203596 ) ) ;
#98152 = EDGE_CURVE ( 'NONE', #67539, #86043, #27505, .T. ) ;
#98153 = CARTESIAN_POINT ( 'NONE',  ( -99.56269727232219680, -25.18439444651947312, 3.795001273127148078 ) ) ;
#98154 = CARTESIAN_POINT ( 'NONE',  ( 12.94906671069258763, 19.00495796004926419, -1.500000000000002220 ) ) ;
#98155 = AXIS2_PLACEMENT_3D ( 'NONE', #6234, #29570, #60548 ) ;
#98156 = B_SPLINE_CURVE_WITH_KNOTS ( 'NONE', 3,
 ( #35620, #82282, #12757, #13258 ),
 .UNSPECIFIED., .F., .F.,
 ( 4, 4 ),
 ( 0.9394548040336853090, 0.9404555510744508906 ),
 .UNSPECIFIED. ) ;
#98157 = COORDINATED_UNIVERSAL_TIME_OFFSET ( 0, 0, .AHEAD. ) ;
#98158 = DIRECTION ( 'NONE',  ( -0.7682573101345352429, 0.000000000000000000, 0.6401411605457412168 ) ) ;
#98159 = CARTESIAN_POINT ( 'NONE',  ( 4.653846153846159517, -6.376774720514415407, 19.99999999999999289 ) ) ;
#98160 = CARTESIAN_POINT ( 'NONE',  ( 9.931738293602487389, -17.53800358597336384, 11.49999999999999645 ) ) ;
#98161 = CARTESIAN_POINT ( 'NONE',  ( 7.749999999999998224, 25.69999999999999574, 0.000000000000000000 ) ) ;
#98162 = DIRECTION ( 'NONE',  ( 1.000000000000000000, 0.000000000000000000, 0.000000000000000000 ) ) ;
#98163 = VECTOR ( 'NONE', #49609, 1000.000000000000000 ) ;
#98165 = PLANE ( 'NONE',  #47353 ) ;
#98164 = VECTOR ( 'NONE', #64251, 1000.000000000000114 ) ;
#98166 = DIRECTION ( 'NONE',  ( 0.000000000000000000, 0.000000000000000000, -1.000000000000000000 ) ) ;
#98167 = CARTESIAN_POINT ( 'NONE',  ( -111.2787752023839971, -25.29779285926202803, 3.894639243670172668 ) ) ;
#98168 = ADVANCED_FACE ( 'NONE', ( #87729 ), #52597, .T. ) ;
#98169 = CARTESIAN_POINT ( 'NONE',  ( -14.63867168220055781, -13.42826565525684579, 11.49999999999998934 ) ) ;
#98170 = B_SPLINE_CURVE_WITH_KNOTS ( 'NONE', 3,
 ( #89709, #20180, #59259, #20679, #13064, #27307, #58270, #36413, #67376, #19677, #50646, #36911, #89210, #81595 ),
 .UNSPECIFIED., .F., .F.,
 ( 4, 2, 2, 2, 2, 2, 4 ),
 ( 1.734723475976807094E-18, 0.0002000904627446527533, 0.0004001809254893037718, 0.0008003618509786153499, 0.001200542776467926820, 0.001400633239212573230, 0.001600723701957219424 ),
 .UNSPECIFIED. ) ;
#98171 = VECTOR ( 'NONE', #82059, 1000.000000000000114 ) ;
#98172 = CARTESIAN_POINT ( 'NONE',  ( -113.5949026862529507, -23.48783264082477018, -1.443836473390084363 ) ) ;
#98173 = CARTESIAN_POINT ( 'NONE',  ( 14.45944668481935658, 13.51102189132778442, -1.500000000000002220 ) ) ;
#98174 = AXIS2_PLACEMENT_3D ( 'NONE', #51307, #90861, #98460 ) ;
#98175 = CARTESIAN_POINT ( 'NONE',  ( -126.5212060924008313, -24.15620529776629155, 10.23563542870658871 ) ) ;
#98176 = CARTESIAN_POINT ( 'NONE',  ( -114.6228709571500701, -23.48783264082478794, -1.443836473390060382 ) ) ;
#98177 = CARTESIAN_POINT ( 'NONE',  ( -66.55620429048340725, -23.47593901973091235, -1.443836447539006196 ) ) ;
#98178 = CARTESIAN_POINT ( 'NONE',  ( 0.1934390699377774303, 20.68474938276070318, 11.49999999999999645 ) ) ;
#98179 = CARTESIAN_POINT ( 'NONE',  ( -58.52287095715006160, -24.64898659630528499, 1.056161002820822592 ) ) ;
#98180 = B_SPLINE_CURVE_WITH_KNOTS ( 'NONE', 3,
 ( #29745, #92135, #16503, #69808, #23109, #93129 ),
 .UNSPECIFIED., .F., .F.,
 ( 4, 2, 4 ),
 ( 1.570887131794638196E-05, 0.001396322306279762591, 0.002776935741241578874 ),
 .UNSPECIFIED. ) ;
#98181 = DIRECTION ( 'NONE',  ( 0.6599726524652352877, 0.000000000000000000, -0.7512896232465891000 ) ) ;
#98182 = CARTESIAN_POINT ( 'NONE',  ( -2.243088942307695177, -5.876774720514409189, 19.14743589743590491 ) ) ;
#98183 = CARTESIAN_POINT ( 'NONE',  ( 22.64978874513612439, 0.4204215919581203442, 11.49999999999999645 ) ) ;
#98184 = ORIENTED_EDGE ( 'NONE', *, *, #83019, .T. ) ;
#98185 = CARTESIAN_POINT ( 'NONE',  ( -70.52287095715007581, -24.99156044556120548, 7.747789690856173195 ) ) ;
#98186 = CARTESIAN_POINT ( 'NONE',  ( -42.58953762381672448, -23.47596703998600276, 11.44779298504227505 ) ) ;
#98187 = DIRECTION ( 'NONE',  ( 3.773278334444167608E-23, -1.000000000000000000, 0.000000000000000000 ) ) ;
#98188 = DIRECTION ( 'NONE',  ( -0.000000000000000000, -1.000000000000000000, -0.000000000000000000 ) ) ;
#98189 = VERTEX_POINT ( 'NONE', #44545 ) ;
#98190 = ORIENTED_EDGE ( 'NONE', *, *, #96283, .F. ) ;
#98191 = CARTESIAN_POINT ( 'NONE',  ( -99.71988582849684235, -25.15588143334361249, 6.904968122648902806 ) ) ;
#98192 = CARTESIAN_POINT ( 'NONE',  ( -17.76840699843883442, -14.40508365592194195, 11.49999999999998934 ) ) ;
#98193 = CARTESIAN_POINT ( 'NONE',  ( 21.57151214508649772, 3.625915217019311583E-15, 0.5000000000000000000 ) ) ;
#98194 = CARTESIAN_POINT ( 'NONE',  ( -7.206546067468990735, 20.34698395366585189, -1.500000000000002220 ) ) ;
#98195 = CARTESIAN_POINT ( 'NONE',  ( -113.5554261954940074, -23.96169478059713853, 10.65365249895717348 ) ) ;
#98196 = CARTESIAN_POINT ( 'NONE',  ( -85.62287095715005592, -29.50250243563736774, 8.947779886222139822 ) ) ;
#98197 = CARTESIAN_POINT ( 'NONE',  ( -5.352388609804938469, -21.92410630658433845, 11.49999999999999645 ) ) ;
#98198 = ORIENTED_EDGE ( 'NONE', *, *, #84463, .T. ) ;
#98199 = CARTESIAN_POINT ( 'NONE',  ( -70.22848692110255797, -25.31612420714911238, 4.852864425714633612 ) ) ;
#98200 = CARTESIAN_POINT ( 'NONE',  ( 21.99661117994144988, 0.4758108284031232760, 11.49999999999998934 ) ) ;
#98201 = FACE_OUTER_BOUND ( 'NONE', #60982, .T. ) ;
#98202 = CARTESIAN_POINT ( 'NONE',  ( 6.573941812937369455, -0.2639660507643297183, -9.295380466955404257E-16 ) ) ;
#98203 = ORIENTED_EDGE ( 'NONE', *, *, #47042, .T. ) ;
#98204 = LINE ( 'NONE', #96233, #11928 ) ;
#98205 = EDGE_CURVE ( 'NONE', #35967, #99333, #4873, .T. ) ;
#98206 = CARTESIAN_POINT ( 'NONE',  ( -9.278253834636469577, -5.876774720514426953, 18.51871304725684553 ) ) ;
#98207 = VERTEX_POINT ( 'NONE', #44043 ) ;
#98208 = LINE ( 'NONE', #75374, #22586 ) ;
#98209 = EDGE_CURVE ( 'NONE', #27813, #65922, #51663, .T. ) ;
#98210 = VERTEX_POINT ( 'NONE', #60283 ) ;
#98211 = ORIENTED_EDGE ( 'NONE', *, *, #79267, .F. ) ;
#98212 = CARTESIAN_POINT ( 'NONE',  ( -65.52287095715006160, -23.47593901973090169, -1.443836447538996870 ) ) ;
#98213 = DIRECTION ( 'NONE',  ( 1.000000000000000000, 3.773278334444166432E-23, 8.201307841325785021E-29 ) ) ;
#98214 = LINE ( 'NONE', #59178, #82789 ) ;
#98215 = CARTESIAN_POINT ( 'NONE',  ( -1.999887071766271784, 20.33596237858139233, -1.500000000000002220 ) ) ;
#98216 = EDGE_CURVE ( 'NONE', #36438, #94640, #21190, .T. ) ;
#98217 = ORIENTED_EDGE ( 'NONE', *, *, #6718, .F. ) ;
#98218 = CARTESIAN_POINT ( 'NONE',  ( -2.492070857093962921, -6.376774720514408301, 19.17707164986947177 ) ) ;
#98219 = CARTESIAN_POINT ( 'NONE',  ( -115.6228709571500985, -23.84081130438200802, 10.88220057463249191 ) ) ;
#98220 = EDGE_CURVE ( 'NONE', #68551, #66723, #37191, .T. ) ;
#98221 = B_SPLINE_CURVE_WITH_KNOTS ( 'NONE', 3,
 ( #37624, #70077, #8180, #54864 ),
 .UNSPECIFIED., .F., .F.,
 ( 4, 4 ),
 ( 0.000000000000000000, 0.0001000000000000167422 ),
 .UNSPECIFIED. ) ;
#98222 = CARTESIAN_POINT ( 'NONE',  ( -89.46310519935765626, -25.11033443737753856, 2.832404817301929612 ) ) ;
#98223 = CARTESIAN_POINT ( 'NONE',  ( -7.962149653358833845, 10.40864506560536462, -0.9106384459055537617 ) ) ;
#98224 = VERTEX_POINT ( 'NONE', #6976 ) ;
#98225 = DIRECTION ( 'NONE',  ( -0.000000000000000000, -1.000000000000000000, -0.000000000000000000 ) ) ;
#98226 = CARTESIAN_POINT ( 'NONE',  ( -28.27652290204276042, -24.63646046079093210, 8.166125576339837266 ) ) ;
#98227 = ADVANCED_FACE ( 'NONE', ( #75972 ), #98757, .T. ) ;
#98228 = CARTESIAN_POINT ( 'NONE',  ( 11.56195852851363526, -17.29799701895051811, 11.49999999999998934 ) ) ;
#98229 = VERTEX_POINT ( 'NONE', #4981 ) ;
#98231 = ORIENTED_EDGE ( 'NONE', *, *, #3842, .T. ) ;
#98230 = DIRECTION ( 'NONE',  ( -1.000000000000000000, -3.773278334444167608E-23, -8.201307833595939069E-29 ) ) ;
#98232 = CIRCLE ( 'NONE', #33413, 18.50000000000000000 ) ;
#98233 = CARTESIAN_POINT ( 'NONE',  ( -28.62287095715006302, -23.79536559617938352, 10.65372852085395117 ) ) ;
#98234 = DIRECTION ( 'NONE',  ( -0.000000000000000000, 2.173523156925979552E-06, -0.9999999999976378895 ) ) ;
#98235 = ORIENTED_EDGE ( 'NONE', *, *, #35823, .F. ) ;
#98236 = ORIENTED_EDGE ( 'NONE', *, *, #91154, .F. ) ;
#98237 = TOROIDAL_SURFACE ( 'NONE', #35092, 1.020000000000000018, 3.060000000000000053 ) ;
#98238 = CARTESIAN_POINT ( 'NONE',  ( 31.50024378385495893, -5.449202613762975211, -3.047402719862319032 ) ) ;
#98239 = CARTESIAN_POINT ( 'NONE',  ( -119.2834285841887976, -25.28334328158019417, 4.245358510314063416 ) ) ;
#98240 = CIRCLE ( 'NONE', #7565, 24.00000000000000000 ) ;
#98241 = CARTESIAN_POINT ( 'NONE',  ( 32.16024265030974050, 5.965225279485572685, 16.27760796525321751 ) ) ;
#98242 = CARTESIAN_POINT ( 'NONE',  ( -71.30358265130861639, -25.31201778570714822, 6.178525724323167267 ) ) ;
#98244 = VERTEX_POINT ( 'NONE', #59270 ) ;
#98243 = CARTESIAN_POINT ( 'NONE',  ( -13.50798789833325664, 17.53495777034937220, 11.49999999999999645 ) ) ;
#98245 = VECTOR ( 'NONE', #20776, 1000.000000000000114 ) ;
#98246 = CARTESIAN_POINT ( 'NONE',  ( -108.5200659837138915, -23.73766607897671221, -1.055555164236429144 ) ) ;
#98247 = CARTESIAN_POINT ( 'NONE',  ( -8.787219534579676861, -20.84281209399103929, 11.49999999999998934 ) ) ;
#98248 = CIRCLE ( 'NONE', #18800, 1.325999999999969647 ) ;
#98250 = ORIENTED_EDGE ( 'NONE', *, *, #11779, .T. ) ;
#98249 = DIRECTION ( 'NONE',  ( -1.000000000000000000, -0.000000000000000000, -0.000000000000000000 ) ) ;
#98251 = ORIENTED_EDGE ( 'NONE', *, *, #87511, .F. ) ;
#98252 = CARTESIAN_POINT ( 'NONE',  ( -81.10288410982862217, -25.31541542150557689, 5.079550372627416266 ) ) ;
#98253 = FACE_OUTER_BOUND ( 'NONE', #83502, .T. ) ;
#98254 = VERTEX_POINT ( 'NONE', #98816 ) ;
#98255 = LINE ( 'NONE', #36374, #68100 ) ;
#98256 = CARTESIAN_POINT ( 'NONE',  ( -4.481184387785930312, -21.81124396384582909, -1.500000000000002220 ) ) ;
#98257 = B_SPLINE_CURVE_WITH_KNOTS ( 'NONE', 3,
 ( #38549, #23309, #69505, #85221, #61404, #15709 ),
 .UNSPECIFIED., .F., .F.,
 ( 4, 2, 4 ),
 ( 6.391158118972359742E-06, 0.001387004593080794169, 0.002767618028042615873 ),
 .UNSPECIFIED. ) ;
#98258 = LINE ( 'NONE', #20146, #50069 ) ;
#98259 = ORIENTED_EDGE ( 'NONE', *, *, #33872, .T. ) ;
#98260 = CARTESIAN_POINT ( 'NONE',  ( -97.62287095715005592, -24.64898659630367916, 1.056161002820829697 ) ) ;
#98261 = CARTESIAN_POINT ( 'NONE',  ( -6.660000000000001030, 9.283009703645923594, -0.8121581124701985344 ) ) ;
#98262 = LINE ( 'NONE', #28769, #31137 ) ;
#98263 = AXIS2_PLACEMENT_3D ( 'NONE', #78499, #70915, #93730 ) ;
#98264 = CARTESIAN_POINT ( 'NONE',  ( -8.160000000000000142, -10.15233964170348457, 0.003711184059992174607 ) ) ;
#98265 = DIRECTION ( 'NONE',  ( 0.000000000000000000, 0.000000000000000000, -1.000000000000000000 ) ) ;
#98266 = CARTESIAN_POINT ( 'NONE',  ( -1.849579639615634097, -19.42000222497389927, 11.49999999999998934 ) ) ;
#98267 = CARTESIAN_POINT ( 'NONE',  ( -19.99255411920323056, 7.849732829375159149, -1.500000000000002220 ) ) ;
#98268 = CARTESIAN_POINT ( 'NONE',  ( -25.81533462945560942, -24.57999804855655057, 3.045127745384520690 ) ) ;
#98269 = DIRECTION ( 'NONE',  ( 0.000000000000000000, -0.7071067811865513475, -0.7071067811865436870 ) ) ;
#98270 = CARTESIAN_POINT ( 'NONE',  ( -34.52287095715006160, -24.64898659630366851, 1.056161002820817485 ) ) ;
#98271 = EDGE_CURVE ( 'NONE', #69448, #76836, #90218, .T. ) ;
#98272 = B_SPLINE_CURVE_WITH_KNOTS ( 'NONE', 3,
 ( #67229, #60615, #99141, #19530 ),
 .UNSPECIFIED., .F., .F.,
 ( 4, 4 ),
 ( 0.6509648380567879533, 0.6599712693289033760 ),
 .UNSPECIFIED. ) ;
#98273 = CARTESIAN_POINT ( 'NONE',  ( -0.7673284989158746239, 22.82873350090251918, -1.500000000000002220 ) ) ;
#98274 = EDGE_CURVE ( 'NONE', #50179, #234, #31062, .T. ) ;
#98275 = CARTESIAN_POINT ( 'NONE',  ( -39.52287095715006160, -24.50216790748204332, 0.6166512839542465096 ) ) ;
#98276 = CARTESIAN_POINT ( 'NONE',  ( -5.366453405989236813, 0.000000000000000000, 0.000000000000000000 ) ) ;
#98277 = CARTESIAN_POINT ( 'NONE',  ( -2.986242917674419850, -19.73498743542299749, 11.49999999999999645 ) ) ;
#98278 = CARTESIAN_POINT ( 'NONE',  ( -89.54303308397305727, -25.06732983082694943, 7.447789526168954843 ) ) ;
#98279 = CARTESIAN_POINT ( 'NONE',  ( -123.6228709571500559, -23.72747288104441665, -1.053458166803660667 ) ) ;
#98280 = DIRECTION ( 'NONE',  ( 0.000000000000000000, 0.000000000000000000, 1.000000000000000000 ) ) ;
#98281 = EDGE_LOOP ( 'NONE', ( #55805, #39751, #35494, #62939 ) ) ;
#98282 = CARTESIAN_POINT ( 'NONE',  ( -26.80331358727276836, -24.60615731223736802, 1.843589714496689957 ) ) ;
#98283 = CARTESIAN_POINT ( 'NONE',  ( -68.52287095715006160, -24.64898659630528854, 1.056161002820824368 ) ) ;
#98284 = CARTESIAN_POINT ( 'NONE',  ( 10.83000837110471082, 18.85367679709202804, -1.500000000000002220 ) ) ;
#98285 = PLANE ( 'NONE',  #20422 ) ;
#98286 = CARTESIAN_POINT ( 'NONE',  ( 7.829539893445508270, 17.95258299782629408, -1.500000000000002220 ) ) ;
#98287 = AXIS2_PLACEMENT_3D ( 'NONE', #15181, #44644, #68972 ) ;
#98288 = DIRECTION ( 'NONE',  ( -3.773278334453079030E-23, 0.9999999999976377785, 2.173523156925979128E-06 ) ) ;
#98289 = EDGE_LOOP ( 'NONE', ( #94933, #29749, #35367, #12823 ) ) ;
#98290 = PERSON_AND_ORGANIZATION_ROLE ( 'classification_officer' ) ;
#98291 = CARTESIAN_POINT ( 'NONE',  ( -91.54409249466895915, -24.66019654487199730, 8.947790411086115725 ) ) ;
#98292 = CARTESIAN_POINT ( 'NONE',  ( -1.382686142301752019, 8.868309232919825646, 9.000000000000000000 ) ) ;
#98293 = CARTESIAN_POINT ( 'NONE',  ( -13.21525772315781388, 15.71049578022273785, 11.49999999999999645 ) ) ;
#98294 = CARTESIAN_POINT ( 'NONE',  ( 13.03371494964462407, -6.475225279485575136, -27.13839018153349869 ) ) ;
#98295 = VECTOR ( 'NONE', #25944, 1000.000000000000000 ) ;
#98296 = DIRECTION ( 'NONE',  ( -3.773278334453079030E-23, 0.9999999999976377785, 2.173523156925979128E-06 ) ) ;
#98297 = ORIENTED_EDGE ( 'NONE', *, *, #724, .T. ) ;
#98298 = CARTESIAN_POINT ( 'NONE',  ( 3.675000000000002043, 14.49999999999999645, 11.24599928863594300 ) ) ;
#98299 = FACE_OUTER_BOUND ( 'NONE', #59208, .T. ) ;
#98300 = CIRCLE ( 'NONE', #36756, 1.000000000000000222 ) ;
#98301 = CARTESIAN_POINT ( 'NONE',  ( -63.62287095715007723, -23.47596703998600631, 11.44779298504227683 ) ) ;
#98302 = VECTOR ( 'NONE', #59707, 1000.000000000000000 ) ;
#98303 = B_SPLINE_CURVE_WITH_KNOTS ( 'NONE', 3,
 ( #35239, #27630, #89516, #20001, #43356, #74293 ),
 .UNSPECIFIED., .F., .F.,
 ( 4, 2, 4 ),
 ( 0.000000000000000000, 0.001381509706665132392, 0.002763019413330264785 ),
 .UNSPECIFIED. ) ;
#98304 = DIRECTION ( 'NONE',  ( 0.000000000000000000, 0.000000000000000000, -1.000000000000000000 ) ) ;
#98305 = EDGE_LOOP ( 'NONE', ( #19576, #60471, #76266, #22844 ) ) ;
#98306 = DIRECTION ( 'NONE',  ( 0.000000000000000000, -1.000000000000000000, 0.000000000000000000 ) ) ;
#98307 = VECTOR ( 'NONE', #98296, 1000.000000000000114 ) ;
#98308 = B_SPLINE_CURVE_WITH_KNOTS ( 'NONE', 3,
 ( #92124, #7382, #54086, #99718, #85007, #38338 ),
 .UNSPECIFIED., .F., .F.,
 ( 4, 2, 4 ),
 ( 6.391158118967745954E-06, 0.001387004593080787013, 0.002767618028042606333 ),
 .UNSPECIFIED. ) ;
#98309 = B_SPLINE_CURVE_WITH_KNOTS ( 'NONE', 3,
 ( #10047, #87173, #54739, #62864, #70959, #24271 ),
 .UNSPECIFIED., .F., .F.,
 ( 4, 2, 4 ),
 ( 0.000000000000000000, 0.001380764517853247950, 0.002761529035706495900 ),
 .UNSPECIFIED. ) ;
#98310 = EDGE_CURVE ( 'NONE', #15278, #2149, #49266, .T. ) ;
#98311 = CARTESIAN_POINT ( 'NONE',  ( -11.96207688724106610, 19.68918167733909641, 11.49999999999999645 ) ) ;
#98312 = CARTESIAN_POINT ( 'NONE',  ( -4.239441843796335263, -22.36999388947090139, 11.49999999999998934 ) ) ;
#98313 = CARTESIAN_POINT ( 'NONE',  ( -70.74026866089612042, -25.30458806305164643, 4.894904395092048333 ) ) ;
#98314 = CARTESIAN_POINT ( 'NONE',  ( 6.184520403203631389, -5.356774720514425603, -25.32021290018218451 ) ) ;
#98315 = CARTESIAN_POINT ( 'NONE',  ( -49.51012166095222256, -25.26844836852635368, 3.931178963968652962 ) ) ;
#98316 = CARTESIAN_POINT ( 'NONE',  ( -40.52287095715004739, -24.15516710230293995, 10.28746687063727450 ) ) ;
#98317 = CARTESIAN_POINT ( 'NONE',  ( -99.16166289166535819, -25.31582281884252339, 5.311370716827876315 ) ) ;
#98318 = CARTESIAN_POINT ( 'NONE',  ( -16.46405638241306946, -14.47283864684382237, 11.49999999999998934 ) ) ;
#98319 = LINE ( 'NONE', #43060, #8936 ) ;
#98320 = CARTESIAN_POINT ( 'NONE',  ( 11.13529270535513760, 4.132774720514426292, -26.87372982997969117 ) ) ;
#98321 = DIRECTION ( 'NONE',  ( -1.000000000000000000, -1.387778780781445429E-16, -0.000000000000000000 ) ) ;
#98322 = DIRECTION ( 'NONE',  ( 5.328431011793917330E-15, 0.000000000000000000, 1.000000000000000000 ) ) ;
#98323 = CARTESIAN_POINT ( 'NONE',  ( -60.24005634512300844, -25.33055341027920093, 4.734098254060623567 ) ) ;
#98324 = ORIENTED_EDGE ( 'NONE', *, *, #34132, .T. ) ;
#98325 = EDGE_CURVE ( 'NONE', #73153, #98739, #17797, .T. ) ;
#98326 = CARTESIAN_POINT ( 'NONE',  ( 2.691128592823461840, 20.25793168094256202, -1.500000000000002220 ) ) ;
#98327 = ORIENTED_EDGE ( 'NONE', *, *, #1587, .F. ) ;
#98328 = ORIENTED_EDGE ( 'NONE', *, *, #20317, .T. ) ;
#98329 = ORIENTED_EDGE ( 'NONE', *, *, #7869, .T. ) ;
#98330 = ORIENTED_EDGE ( 'NONE', *, *, #60899, .F. ) ;
#98331 = CARTESIAN_POINT ( 'NONE',  ( 23.03040035405544472, 1.057182387018521963, -1.500000000000002220 ) ) ;
#98332 = CARTESIAN_POINT ( 'NONE',  ( -62.62287095715004881, -29.50250786944525672, 11.44777988621623876 ) ) ;
#98333 = CARTESIAN_POINT ( 'NONE',  ( -5.148175472751820081, -19.54457232503198227, -1.500000000000002220 ) ) ;
#98334 = EDGE_CURVE ( 'NONE', #76664, #87834, #10604, .T. ) ;
#98335 = ORIENTED_EDGE ( 'NONE', *, *, #81969, .T. ) ;
#98336 = VECTOR ( 'NONE', #50466, 1000.000000000000114 ) ;
#98337 = FACE_OUTER_BOUND ( 'NONE', #51940, .T. ) ;
#98338 = CARTESIAN_POINT ( 'NONE',  ( -116.6228709571500559, -29.50250786944525672, 11.44777988621622811 ) ) ;
#98339 = ADVANCED_FACE ( 'NONE', ( #55170 ), #47049, .T. ) ;
#98340 = CARTESIAN_POINT ( 'NONE',  ( -101.5228709571500190, -23.73934037231757088, 11.05740245334327909 ) ) ;
#98341 = CARTESIAN_POINT ( 'NONE',  ( -53.61319971673114537, -23.48786465467240347, 11.44779295918255002 ) ) ;
#98343 = VERTEX_POINT ( 'NONE', #37925 ) ;
#98342 = CARTESIAN_POINT ( 'NONE',  ( -7.042111407433782055, -20.27750348750624099, 11.49999999999999645 ) ) ;
#98344 = DIRECTION ( 'NONE',  ( -3.773278334444166432E-23, 1.000000000000000000, 0.000000000000000000 ) ) ;
#98345 = ADVANCED_FACE ( 'NONE', ( #94202 ), #73608, .T. ) ;
#98346 = ORIENTED_EDGE ( 'NONE', *, *, #94324, .T. ) ;
#98347 = VECTOR ( 'NONE', #78782, 1000.000000000000000 ) ;
#98348 = ADVANCED_FACE ( 'NONE', ( #2884 ), #79487, .F. ) ;
#98349 = CARTESIAN_POINT ( 'NONE',  ( -16.63904852704994042, -12.34428335884295969, 11.49999999999998934 ) ) ;
#98350 = VERTEX_POINT ( 'NONE', #26203 ) ;
#98351 = B_SPLINE_CURVE_WITH_KNOTS ( 'NONE', 3,
 ( #4420, #49602, #56719, #87654 ),
 .UNSPECIFIED., .F., .F.,
 ( 4, 4 ),
 ( 0.000000000000000000, 9.999999999998897304E-05 ),
 .UNSPECIFIED. ) ;
#98352 = CARTESIAN_POINT ( 'NONE',  ( -28.53660849338690042, -24.18923150054469318, 0.1864216068622559508 ) ) ;
#98353 = ORIENTED_EDGE ( 'NONE', *, *, #75100, .F. ) ;
#98354 = CARTESIAN_POINT ( 'NONE',  ( -61.52287095715006160, -24.66019654487199730, 8.947790411086121054 ) ) ;
#98355 = VERTEX_POINT ( 'NONE', #3385 ) ;
#98356 = CARTESIAN_POINT ( 'NONE',  ( -5.518977837361389582, -20.17201009624758257, -1.500000000000002220 ) ) ;
#98357 = ADVANCED_FACE ( 'NONE', ( #87607 ), #3881, .T. ) ;
#98358 = CARTESIAN_POINT ( 'NONE',  ( -18.59763704738199408, -11.70098744416181979, 11.49999999999999645 ) ) ;
#98359 = CARTESIAN_POINT ( 'NONE',  ( -37.62372564847699152, -24.66019654487199730, 8.947790411086113949 ) ) ;
#98360 = CARTESIAN_POINT ( 'NONE',  ( -6.671648801611133273, 21.52854475820963032, -1.500000000000002220 ) ) ;
#98361 = VECTOR ( 'NONE', #32505, 1000.000000000000000 ) ;
#98362 = CARTESIAN_POINT ( 'NONE',  ( -0.6469382494902750080, 20.97623560764392181, 11.49999999999998934 ) ) ;
#98363 = CARTESIAN_POINT ( 'NONE',  ( -80.58953762381673869, -24.99132157543084531, 2.256160258750495640 ) ) ;
#98364 = CARTESIAN_POINT ( 'NONE',  ( -29.52287095715006160, -29.50250473134420659, 10.00399446418115268 ) ) ;
#98365 = CARTESIAN_POINT ( 'NONE',  ( 5.642884982650352654, -6.376774720514426065, 20.85668005806743608 ) ) ;
#98366 = ORIENTED_EDGE ( 'NONE', *, *, #52630, .F. ) ;
#98367 = ORIENTED_EDGE ( 'NONE', *, *, #54940, .T. ) ;
#98368 = ORIENTED_EDGE ( 'NONE', *, *, #73817, .T. ) ;
#98369 = CARTESIAN_POINT ( 'NONE',  ( -31.52287095715006160, -24.64965694238574656, 8.947790433994207149 ) ) ;
#98370 = VECTOR ( 'NONE', #44676, 1000.000000000000114 ) ;
#98371 = CARTESIAN_POINT ( 'NONE',  ( 8.645823604709390153, 19.67543227842514852, -1.500000000000002220 ) ) ;
#98372 = CARTESIAN_POINT ( 'NONE',  ( -11.64875734969026233, -0.3587747205144265483, 30.51402280011862089 ) ) ;
#98373 = VERTEX_POINT ( 'NONE', #33814 ) ;
#98374 = CARTESIAN_POINT ( 'NONE',  ( -18.69274626484788371, 9.848020819832786543, 11.49999999999998934 ) ) ;
#98375 = CARTESIAN_POINT ( 'NONE',  ( -71.20541289166536103, -25.30502758240210071, 4.885889971059796721 ) ) ;
#98376 = CARTESIAN_POINT ( 'NONE',  ( -64.50492162725981871, -24.15543982623906416, -0.2315651400026674800 ) ) ;
#98377 = CARTESIAN_POINT ( 'NONE',  ( -83.58528645688662095, -24.51419770103157347, 9.386484678747182286 ) ) ;
#98378 = CIRCLE ( 'NONE', #80575, 1.500000000000000666 ) ;
#98379 = CARTESIAN_POINT ( 'NONE',  ( 0.4987820251299121543, -0.03487823687206273449, 9.000000000000000000 ) ) ;
#98380 = CARTESIAN_POINT ( 'NONE',  ( -99.20106123879247662, -25.22504103827928290, 3.603421885566837624 ) ) ;
#98381 = CARTESIAN_POINT ( 'NONE',  ( 10.35204687333978057, 19.51823071965408829, -1.500000000000002220 ) ) ;
#98382 = CARTESIAN_POINT ( 'NONE',  ( -116.5884090418037431, -24.51314013834316086, 0.6176544820404278324 ) ) ;
#98383 = CARTESIAN_POINT ( 'NONE',  ( -51.90278039571972357, -25.24860200595528781, 5.898133925283090662 ) ) ;
#98384 = CARTESIAN_POINT ( 'NONE',  ( -33.92287095715005307, -23.47593901973090169, -1.443836447538998202 ) ) ;
#98385 = CARTESIAN_POINT ( 'NONE',  ( 31.88667425545053291, 1.477225279485574028, -9.651215965565024035 ) ) ;
#98386 = EDGE_CURVE ( 'NONE', #56311, #44968, #73507, .T. ) ;
#98387 = CARTESIAN_POINT ( 'NONE',  ( -58.52287095715004739, -23.47593901973090169, -1.443836447538997092 ) ) ;
#98388 = CARTESIAN_POINT ( 'NONE',  ( -16.98888496755095545, 9.415225082695979353, 11.49999999999998934 ) ) ;
#98389 = CARTESIAN_POINT ( 'NONE',  ( -21.34312709018487553, 1.176582458498846462, -1.500000000000002220 ) ) ;
#98390 = LINE ( 'NONE', #75053, #96871 ) ;
#98391 = CARTESIAN_POINT ( 'NONE',  ( -61.52287095715006160, -23.48786465467241058, 11.44779295918254824 ) ) ;
#98392 = EDGE_CURVE ( 'NONE', #42618, #67734, #19579, .T. ) ;
#98393 = DIRECTION ( 'NONE',  ( 1.000000000000000000, 0.000000000000000000, 0.000000000000000000 ) ) ;
#98394 = CARTESIAN_POINT ( 'NONE',  ( -129.2228709571500644, -23.47593901973090524, -1.443836447538995982 ) ) ;
#98395 = CARTESIAN_POINT ( 'NONE',  ( -17.13258802378025791, -14.77425600068537115, -1.500000000000002220 ) ) ;
#98396 = ORIENTED_EDGE ( 'NONE', *, *, #44173, .F. ) ;
#98397 = CARTESIAN_POINT ( 'NONE',  ( -128.5562042904834072, -24.65952944569305316, 1.056160979905707009 ) ) ;
#98398 = CARTESIAN_POINT ( 'NONE',  ( -79.64682910312916420, -23.48783264082476308, -1.443836473390096575 ) ) ;
#98399 = CARTESIAN_POINT ( 'NONE',  ( -9.134819693115781902, 17.59984377705169933, 11.49999999999999645 ) ) ;
#98400 = CARTESIAN_POINT ( 'NONE',  ( -23.29179552176162105, 0.3587747205144061202, -17.29637630388739211 ) ) ;
#98401 = CARTESIAN_POINT ( 'NONE',  ( -113.6228709571500559, -29.50248528299804818, 1.056150453629043584 ) ) ;
#98402 = EDGE_LOOP ( 'NONE', ( #30692, #85855, #96863, #58830 ) ) ;
#98403 = DIRECTION ( 'NONE',  ( -3.773278334453079030E-23, 0.9999999999976377785, 2.173523156925979128E-06 ) ) ;
#98404 = CARTESIAN_POINT ( 'NONE',  ( -116.5228709571500616, -29.50250243563736774, 8.947779886222134493 ) ) ;
#98405 = CARTESIAN_POINT ( 'NONE',  ( 1.408343819019456028E-16, -6.943225279485572443, 1.149999999999999911 ) ) ;
#98406 = CARTESIAN_POINT ( 'NONE',  ( -2.642555958445479192, -21.45212208726272607, 11.49999999999998934 ) ) ;
#98407 = AXIS2_PLACEMENT_3D ( 'NONE', #49984, #58094, #36241 ) ;
#98408 = DIRECTION ( 'NONE',  ( 0.000000000000000000, -1.000000000000000000, 0.000000000000000000 ) ) ;
#98409 = CARTESIAN_POINT ( 'NONE',  ( 18.72033823704212097, 5.060218808788302880, -1.500000000000002220 ) ) ;
#98410 = DIRECTION ( 'NONE',  ( -0.000000000000000000, 2.173523156925979552E-06, -0.9999999999976378895 ) ) ;
#98411 = CARTESIAN_POINT ( 'NONE',  ( -61.52287095715006160, -29.50250243563736774, 8.947779886222145151 ) ) ;
#98412 = CARTESIAN_POINT ( 'NONE',  ( 4.927431051831622000, -19.18327824014073357, -1.500000000000002220 ) ) ;
#98413 = ORIENTED_EDGE ( 'NONE', *, *, #86793, .F. ) ;
#98414 = AXIS2_PLACEMENT_3D ( 'NONE', #70833, #37880, #54608 ) ;
#98415 = CARTESIAN_POINT ( 'NONE',  ( 17.42226438573850800, -10.51879874471254261, 11.49999999999999645 ) ) ;
#98416 = CARTESIAN_POINT ( 'NONE',  ( -1.164890887384984586, 4.028272616778474813, -2.677392948487098267E-15 ) ) ;
#98417 = CC_DESIGN_PERSON_AND_ORGANIZATION_ASSIGNMENT ( #80955, #17551, ( #95340 ) ) ;
#98418 = CARTESIAN_POINT ( 'NONE',  ( 33.61456970919608978, -3.316774720514426900, -11.35828564741662738 ) ) ;
#98419 = ORIENTED_EDGE ( 'NONE', *, *, #53289, .F. ) ;
#98420 = CARTESIAN_POINT ( 'NONE',  ( -102.5982595925881213, -23.48786465467241058, 11.44779295918254292 ) ) ;
#98421 = FACE_OUTER_BOUND ( 'NONE', #79234, .T. ) ;
#98422 = DIRECTION ( 'NONE',  ( 0.000000000000000000, 0.000000000000000000, 1.000000000000000000 ) ) ;
#98423 = DIRECTION ( 'NONE',  ( -1.607395343451207646E-13, 0.000000000000000000, -1.000000000000000000 ) ) ;
#98424 = CARTESIAN_POINT ( 'NONE',  ( -33.55620429048339304, -23.48783264082477373, -1.443836473390074593 ) ) ;
#98425 = CARTESIAN_POINT ( 'NONE',  ( -17.52916707085001136, 9.785066945116392745, 11.49999999999998934 ) ) ;
#98426 = CARTESIAN_POINT ( 'NONE',  ( -28.62287095715006302, -23.33147402473456822, -1.443835808584760683 ) ) ;
#98427 = ORIENTED_EDGE ( 'NONE', *, *, #29493, .F. ) ;
#98428 = CARTESIAN_POINT ( 'NONE',  ( -5.576923076923076650, -6.376774720514418959, 20.44941907051282470 ) ) ;
#98429 = AXIS2_PLACEMENT_3D ( 'NONE', #15524, #93144, #23630 ) ;
#98430 = CARTESIAN_POINT ( 'NONE',  ( -5.953223121155255981, 22.05028593715628560, 11.49999999999999645 ) ) ;
#98431 = CARTESIAN_POINT ( 'NONE',  ( -30.47287095715008221, -24.37837718399783782, 0.3290379132693308506 ) ) ;
#98432 = CARTESIAN_POINT ( 'NONE',  ( -86.62287095715008434, -24.33832256526968862, 0.1851278514119904517 ) ) ;
#98433 = CARTESIAN_POINT ( 'NONE',  ( 22.02124265030973760, -4.543225279485573864, 16.20402280011862217 ) ) ;
#98434 = DIRECTION ( 'NONE',  ( 2.910297583984928910E-15, -1.000000000000000000, -3.056206645085457922E-15 ) ) ;
#98435 = AXIS2_PLACEMENT_3D ( 'NONE', #14983, #86498, #38320 ) ;
#98436 = PERSON ( 'NAUO-PER12', 'UNSPECIFIED', 'UNSPECIFIED', ('UNSPECIFIED'), ('UNSPECIFIED'), ('UNSPECIFIED') ) ;
#98437 = CARTESIAN_POINT ( 'NONE',  ( -7.749999999999996447, 25.69999999999999574, 2.100000000000000089 ) ) ;
#98438 = CARTESIAN_POINT ( 'NONE',  ( 11.64234319522276095, -19.14997049866658330, 11.49999999999999645 ) ) ;
#98439 = LINE ( 'NONE', #28434, #46881 ) ;
#98440 = EDGE_LOOP ( 'NONE', ( #32740, #77643, #39367, #58177 ) ) ;
#98441 = AXIS2_PLACEMENT_3D ( 'NONE', #2196, #4187, #88925 ) ;
#98442 = CARTESIAN_POINT ( 'NONE',  ( 15.61528876134825161, -13.05345633644532732, -1.500000000000002220 ) ) ;
#98443 = VERTEX_POINT ( 'NONE', #57175 ) ;
#98444 = EDGE_CURVE ( 'NONE', #27962, #37175, #88111, .T. ) ;
#98445 = CARTESIAN_POINT ( 'NONE',  ( 4.748521865011817944, 22.44708532425888592, 11.49999999999998934 ) ) ;
#98446 = DIRECTION ( 'NONE',  ( 0.000000000000000000, 0.000000000000000000, 1.000000000000000000 ) ) ;
#98447 = VERTEX_POINT ( 'NONE', #71387 ) ;
#98448 = CARTESIAN_POINT ( 'NONE',  ( -60.52287095715006160, -23.47593901973090169, -1.443836447538996870 ) ) ;
#98449 = CARTESIAN_POINT ( 'NONE',  ( 282.9764569301858046, 5.965225279485572685, 20.79159422840526616 ) ) ;
#98450 = CARTESIAN_POINT ( 'NONE',  ( -87.52287095715006160, -24.64898659630528854, 1.056161002820827921 ) ) ;
#98452 = ORIENTED_EDGE ( 'NONE', *, *, #33990, .F. ) ;
#98451 = CARTESIAN_POINT ( 'NONE',  ( -12.22836702412972087, 17.35733969022439993, 11.49999999999999645 ) ) ;
#98453 = ADVANCED_FACE ( 'NONE', ( #87097 ), #18579, .F. ) ;
#98454 = ORIENTED_EDGE ( 'NONE', *, *, #22237, .F. ) ;
#98455 = CARTESIAN_POINT ( 'NONE',  ( 13.47465251475156656, -17.59220275312388182, -1.500000000000002220 ) ) ;
#98456 = EDGE_CURVE ( 'NONE', #22596, #50681, #17905, .T. ) ;
#98457 = CARTESIAN_POINT ( 'NONE',  ( 0.06016934085327452914, 20.63536315578604174, 11.49999999999998934 ) ) ;
#98458 = ORIENTED_EDGE ( 'NONE', *, *, #70625, .F. ) ;
#98459 = ORIENTED_EDGE ( 'NONE', *, *, #8299, .F. ) ;
#98460 = DIRECTION ( 'NONE',  ( -3.773278334444166432E-23, 1.000000000000000000, 0.000000000000000000 ) ) ;
#98461 = CARTESIAN_POINT ( 'NONE',  ( 2.880689065218799083, -5.876774720514425177, 21.31732089891691828 ) ) ;
#98462 = ORIENTED_EDGE ( 'NONE', *, *, #51370, .T. ) ;
#98463 = ORIENTED_EDGE ( 'NONE', *, *, #56668, .F. ) ;
#98464 = CARTESIAN_POINT ( 'NONE',  ( 30.56422633351845519, 2.967394884211873585, 24.91953760856571520 ) ) ;
#98465 = CARTESIAN_POINT ( 'NONE',  ( -111.5920143885692539, -23.96169478059714564, 10.65365249895717348 ) ) ;
#98466 = LINE ( 'NONE', #46197, #73039 ) ;
#98467 = CARTESIAN_POINT ( 'NONE',  ( -19.91680486407696904, 5.911688619927280008, -1.500000000000002220 ) ) ;
#98468 = EDGE_CURVE ( 'NONE', #94978, #68827, #89105, .T. ) ;
#98469 = CARTESIAN_POINT ( 'NONE',  ( -9.857415191643349672, 19.42730305858377449, 11.49999999999999645 ) ) ;
#98470 = EDGE_LOOP ( 'NONE', ( #91340, #563, #29978, #25345 ) ) ;
#98471 = CARTESIAN_POINT ( 'NONE',  ( -39.50194508182622144, -25.25391041027802075, 3.881369232628720134 ) ) ;
#98472 = CARTESIAN_POINT ( 'NONE',  ( -52.52287095715006160, -24.50216790748203621, 0.6166512839542510616 ) ) ;
#98473 = AXIS2_PLACEMENT_3D ( 'NONE', #87665, #72946, #80545 ) ;
#98474 = CARTESIAN_POINT ( 'NONE',  ( -115.6256605899217647, -24.63355581998384736, 0.9682620441943983192 ) ) ;
#98475 = CARTESIAN_POINT ( 'NONE',  ( -13.02831144489870319, 18.26546089674541307, -1.500000000000002220 ) ) ;
#98476 = CARTESIAN_POINT ( 'NONE',  ( 22.02124265030973760, -6.143225279485574397, 12.85402280011862430 ) ) ;
#98477 = VERTEX_POINT ( 'NONE', #40434 ) ;
#98478 = CARTESIAN_POINT ( 'NONE',  ( -11.64875734969026233, -5.965225279485572685, 30.51402280011862089 ) ) ;
#98479 = CARTESIAN_POINT ( 'NONE',  ( -51.50945306740351981, -25.19752791585493412, 3.378729448321072137 ) ) ;
#98480 = B_SPLINE_SURFACE_WITH_KNOTS ( 'NONE', 1, 3, ( 
 ( #21063, #52033, #82962, #75349, #60159, #5850, #91082, #13951, #37309, #68255 ),
 ( #99184, #91576, #45919, #55029, #30680, #47916, #86466, #77835, #61651, #84466 ) ),
 .UNSPECIFIED., .F., .F., .F.,
 ( 2, 2 ),
 ( 4, 2, 2, 2, 4 ),
 ( 0.000000000000000000, 1.000000000000000000 ),
 ( 0.000000000000000000, 0.2500000000000000000, 0.5000000000000000000, 0.7500000000000000000, 1.000000000000000000 ),
 .UNSPECIFIED. ) ;
#98481 = ORIENTED_EDGE ( 'NONE', *, *, #20955, .F. ) ;
#98482 = ORIENTED_EDGE ( 'NONE', *, *, #59686, .T. ) ;
#98483 = CARTESIAN_POINT ( 'NONE',  ( -100.5248763468820528, -25.31387855574000412, 5.206551135935474584 ) ) ;
#98484 = ORIENTED_EDGE ( 'NONE', *, *, #86238, .F. ) ;
#98485 = CARTESIAN_POINT ( 'NONE',  ( 6.245503531335690361, -20.37428601906679759, -1.500000000000002220 ) ) ;
#98486 = ORIENTED_EDGE ( 'NONE', *, *, #58101, .T. ) ;
#98487 = CARTESIAN_POINT ( 'NONE',  ( -5.988734693054777125, -5.876774720514416295, 19.95737465391042065 ) ) ;
#98488 = CARTESIAN_POINT ( 'NONE',  ( -17.04133944854041616, 12.32129857345222845, -1.500000000000002220 ) ) ;
#98489 = DIRECTION ( 'NONE',  ( 0.000000000000000000, 0.000000000000000000, 1.000000000000000000 ) ) ;
#98490 = CARTESIAN_POINT ( 'NONE',  ( 16.14549698687068968, 15.95341496147077720, -1.500000000000002220 ) ) ;
#98491 = CARTESIAN_POINT ( 'NONE',  ( 14.61581676225028126, -3.316774720514426456, -27.35847991880135766 ) ) ;
#98492 = CARTESIAN_POINT ( 'NONE',  ( -65.62287095715005592, -29.50250243563736774, 8.947779886222143375 ) ) ;
#98493 = CARTESIAN_POINT ( 'NONE',  ( 15.10893391618534665, -15.86458014800626692, -1.500000000000002220 ) ) ;
#98494 = PLANE ( 'NONE',  #94914 ) ;
#98495 = ORIENTED_EDGE ( 'NONE', *, *, #97647, .T. ) ;
#98496 = CARTESIAN_POINT ( 'NONE',  ( -80.35919894935766195, -25.30543142107805465, 4.505481316334992492 ) ) ;
#98497 = EDGE_CURVE ( 'NONE', #36479, #23202, #97765, .T. ) ;
#98498 = VECTOR ( 'NONE', #7307, 1000.000000000000114 ) ;
#98499 = ORIENTED_EDGE ( 'NONE', *, *, #5597, .T. ) ;
#98500 = B_SPLINE_CURVE_WITH_KNOTS ( 'NONE', 3,
 ( #81829, #73716, #19427, #80836 ),
 .UNSPECIFIED., .F., .F.,
 ( 4, 4 ),
 ( 0.9504646280033649530, 0.9594710592754805978 ),
 .UNSPECIFIED. ) ;
#98501 = EDGE_CURVE ( 'NONE', #46605, #97072, #32816, .T. ) ;
#98502 = CARTESIAN_POINT ( 'NONE',  ( -84.62359700266976859, -24.66019654487200441, 8.947790411086119278 ) ) ;
#98503 = CARTESIAN_POINT ( 'NONE',  ( -130.5728709571500872, -25.30557784678704891, 3.856996771331003604 ) ) ;
#98504 = CARTESIAN_POINT ( 'NONE',  ( -30.59902020641925446, -24.82963700391604078, 1.633150109380534509 ) ) ;
#98505 = CARTESIAN_POINT ( 'NONE',  ( 6.361473516681357410, -20.28576754457002451, -1.500000000000002220 ) ) ;
#98506 = DIRECTION ( 'NONE',  ( -3.773278334453079618E-23, 0.9999999999976377785, 2.173523156925979975E-06 ) ) ;
#98507 = CARTESIAN_POINT ( 'NONE',  ( -26.92257395956520938, -24.75186024773817195, 2.526140358845352374 ) ) ;
#98508 = CARTESIAN_POINT ( 'NONE',  ( -85.58560984767410673, -24.73486907724918282, 1.287355809206962576 ) ) ;
#98509 = VECTOR ( 'NONE', #25475, 1000.000000000000000 ) ;
#98510 = CARTESIAN_POINT ( 'NONE',  ( -70.52287095715010423, -24.14321612903118108, -0.2833117244520866329 ) ) ;
#98511 = EDGE_CURVE ( 'NONE', #87661, #62785, #9787, .T. ) ;
#98512 = CARTESIAN_POINT ( 'NONE',  ( -79.62287095715007013, -23.95044443724992433, 10.65354141964649948 ) ) ;
#98513 = VERTEX_POINT ( 'NONE', #64293 ) ;
#98514 = DIRECTION ( 'NONE',  ( -3.773278334453080206E-23, 0.9999999999976377785, 2.173523156925979975E-06 ) ) ;
#98515 = CARTESIAN_POINT ( 'NONE',  ( 16.09843989366402539, -11.26760994518913428, 11.49999999999999645 ) ) ;
#98516 = CARTESIAN_POINT ( 'NONE',  ( -58.62287095715004881, -24.66019654487199020, 8.947790411086131712 ) ) ;
#98517 = VECTOR ( 'NONE', #67623, 1000.000000000000114 ) ;
#98518 = DIRECTION ( 'NONE',  ( 0.000000000000000000, 2.688821387764050602E-15, -1.000000000000000000 ) ) ;
#98519 = ORIENTED_EDGE ( 'NONE', *, *, #99643, .F. ) ;
#98520 = CARTESIAN_POINT ( 'NONE',  ( -88.63180305775179590, -24.15620529776628800, 10.23563542870660115 ) ) ;
#98521 = CARTESIAN_POINT ( 'NONE',  ( -40.62287095715005592, -23.47596703998600276, 11.44779298504227505 ) ) ;
#98522 = CARTESIAN_POINT ( 'NONE',  ( -25.56040553771592627, -24.91036900288112932, 5.683877138022538134 ) ) ;
#98523 = CARTESIAN_POINT ( 'NONE',  ( -31.62287095715005236, -29.50250786944525672, 11.44777988621624409 ) ) ;
#98524 = CARTESIAN_POINT ( 'NONE',  ( -18.32884136524465291, -7.267937366463995907, -1.500000000000002220 ) ) ;
#98525 = AXIS2_PLACEMENT_3D ( 'NONE', #38264, #55507, #69222 ) ;
#98526 = ORIENTED_EDGE ( 'NONE', *, *, #11340, .T. ) ;
#98527 = CARTESIAN_POINT ( 'NONE',  ( -27.96875734969026084, 3.316774720514426456, 0.7300228001186309656 ) ) ;
#98528 = CARTESIAN_POINT ( 'NONE',  ( -70.62287095715007013, -24.52232992886364116, 0.6492154411906061462 ) ) ;
#98529 = EDGE_CURVE ( 'NONE', #61311, #40045, #68645, .T. ) ;
#98530 = APPROVAL_STATUS ( 'not_yet_approved' ) ;
#98531 = VERTEX_POINT ( 'NONE', #97209 ) ;
#98532 = CARTESIAN_POINT ( 'NONE',  ( 8.991545460846682047, -0.9385453280025082279, 3.722136940144805450 ) ) ;
#98533 = DIRECTION ( 'NONE',  ( -0.000000000000000000, 1.000000000000000000, -0.000000000000000000 ) ) ;
#98534 = CARTESIAN_POINT ( 'NONE',  ( -55.58581373341920795, -24.63355581998385446, 0.9682620441943891043 ) ) ;
#98535 = CARTESIAN_POINT ( 'NONE',  ( -0.02075734969026423599, 6.376774720514426953, -28.03397719988137382 ) ) ;
#98536 = CARTESIAN_POINT ( 'NONE',  ( -31.62287095715005236, -24.50321055353803246, 9.387540953477538253 ) ) ;
#98537 = EDGE_CURVE ( 'NONE', #46703, #56978, #1686, .T. ) ;
#98538 = CARTESIAN_POINT ( 'NONE',  ( -115.6228709571500559, -29.50249982740957577, 7.747779886224967605 ) ) ;
#98539 = CARTESIAN_POINT ( 'NONE',  ( -85.62287095715007013, -25.00158670708909270, 2.256160236439165967 ) ) ;
#98540 = CARTESIAN_POINT ( 'NONE',  ( 10.22567584263966722, 17.17405255344276682, 11.49999999999998934 ) ) ;
#98541 = B_SPLINE_CURVE_WITH_KNOTS ( 'NONE', 3,
 ( #42767, #97037, #81313, #99012 ),
 .UNSPECIFIED., .F., .F.,
 ( 4, 4 ),
 ( 0.000000000000000000, 0.0001000000000000028644 ),
 .UNSPECIFIED. ) ;
#98542 = CARTESIAN_POINT ( 'NONE',  ( -125.6228709571500559, -24.83620972994593501, 8.398175272781356782 ) ) ;
#98543 = CARTESIAN_POINT ( 'NONE',  ( -0.02741748178391386140, -22.69505915253172645, 2.088213449219022078 ) ) ;
#98544 = ORIENTED_EDGE ( 'NONE', *, *, #23411, .T. ) ;
#98545 = EDGE_CURVE ( 'NONE', #62532, #39962, #66788, .T. ) ;
#98546 = CARTESIAN_POINT ( 'NONE',  ( -116.5228709571500616, -23.47596703998600631, 11.44779298504227860 ) ) ;
#98547 = CARTESIAN_POINT ( 'NONE',  ( 4.612744205187371271, -5.876774720514418071, 20.61169588237105188 ) ) ;
#98548 = ADVANCED_FACE ( 'NONE', ( #44433 ), #13459, .T. ) ;
#98549 = CARTESIAN_POINT ( 'NONE',  ( -119.6235011850299941, -24.65952944569305316, 1.056160979905713226 ) ) ;
#98550 = LINE ( 'NONE', #53401, #45905 ) ;
#98551 = LINE ( 'NONE', #12319, #51030 ) ;
#98552 = CARTESIAN_POINT ( 'NONE',  ( -39.55296486377296361, -23.96119346886879597, -0.6495511937832144644 ) ) ;
#98553 = DIRECTION ( 'NONE',  ( -3.773278334453079618E-23, 0.9999999999976377785, 2.173523156925979975E-06 ) ) ;
#98554 = B_SPLINE_CURVE_WITH_KNOTS ( 'NONE', 3,
 ( #24612, #78897, #71814, #85516 ),
 .UNSPECIFIED., .F., .F.,
 ( 4, 4 ),
 ( 1.387778780781445676E-17, 0.0001000000000000028508 ),
 .UNSPECIFIED. ) ;
#98555 = CARTESIAN_POINT ( 'NONE',  ( -51.53844848903055009, -25.26280016857193544, 4.526031668297421540 ) ) ;
#98556 = ORIENTED_EDGE ( 'NONE', *, *, #77018, .F. ) ;
#98557 = B_SPLINE_SURFACE_WITH_KNOTS ( 'NONE', 3, 3, ( 
 ( #87895, #89392, #2670, #19865 ),
 ( #49350, #33607, #50839, #12248 ),
 ( #64590, #25991, #80279, #74168 ),
 ( #4664, #41737, #96500, #6644 ),
 ( #76146, #53337, #14749, #21359 ),
 ( #31873, #21855, #74656, #36103 ),
 ( #8531, #75156, #52827, #91877 ) ),
 .UNSPECIFIED., .F., .F., .F.,
 ( 4, 3, 4 ),
 ( 4, 4 ),
 ( 0.7945040050992245861, 0.8970133687736505657, 0.9995227324480765452 ),
 ( 0.8397073785246207400, 0.8411077677278031572 ),
 .UNSPECIFIED. ) ;
#98558 = CARTESIAN_POINT ( 'NONE',  ( -34.62287095715005592, -24.34917612406837861, 0.1852690917426565997 ) ) ;
#98559 = DIRECTION ( 'NONE',  ( 0.9975640502598243087, -0.06975647374412546897, -0.000000000000000000 ) ) ;
#98560 = ORIENTED_EDGE ( 'NONE', *, *, #76160, .F. ) ;
#98561 = CARTESIAN_POINT ( 'NONE',  ( -8.208445925564873846, -18.52556626786687488, 11.49999999999998934 ) ) ;
#98562 = EDGE_CURVE ( 'NONE', #74504, #53799, #81, .T. ) ;
#98563 = CARTESIAN_POINT ( 'NONE',  ( -122.5214661034149373, -23.73766607897671221, -1.055555164236450461 ) ) ;
#98564 = DIRECTION ( 'NONE',  ( -0.000000000000000000, 1.000000000000000000, -0.000000000000000000 ) ) ;
#98565 = VECTOR ( 'NONE', #5838, 1000.000000000000000 ) ;
#98566 = LINE ( 'NONE', #12832, #49310 ) ;
#98567 = ORIENTED_EDGE ( 'NONE', *, *, #77490, .T. ) ;
#98568 = CARTESIAN_POINT ( 'NONE',  ( -94.92287095715005307, -23.47596703998600276, 11.44779298504227860 ) ) ;
#98569 = PLANE ( 'NONE',  #85912 ) ;
#98570 = CARTESIAN_POINT ( 'NONE',  ( 8.743921044546416610, -18.04861246754477477, -1.500000000000002220 ) ) ;
#98571 = CARTESIAN_POINT ( 'NONE',  ( 6.686094007546604878, -20.02240253118446844, 11.49999999999999645 ) ) ;
#98572 = DIRECTION ( 'NONE',  ( -3.773278334453079618E-23, 0.9999999999976377785, 2.173523156925979975E-06 ) ) ;
#98573 = B_SPLINE_CURVE_WITH_KNOTS ( 'NONE', 3,
 ( #46798, #78718, #72146, #92951, #23426, #85344 ),
 .UNSPECIFIED., .F., .F.,
 ( 4, 2, 4 ),
 ( 6.391158118964604309E-06, 0.001387004593080783327, 0.002767618028042601996 ),
 .UNSPECIFIED. ) ;
#98574 = CARTESIAN_POINT ( 'NONE',  ( -70.59200721846467275, -24.40133493613049964, 9.663955038902802386 ) ) ;
#98575 = CARTESIAN_POINT ( 'NONE',  ( 0.6065052782250800467, 22.08157775750015617, 11.49999999999998934 ) ) ;
#98576 = ADVANCED_FACE ( 'NONE', ( #20080 ), #29692, .F. ) ;
#98577 = CARTESIAN_POINT ( 'NONE',  ( -20.35906544237474236, -2.577633573104691322, 11.49999999999998934 ) ) ;
#98578 = DIRECTION ( 'NONE',  ( -1.000000000000000000, -3.773278334444166432E-23, -8.201307841325785021E-29 ) ) ;
#98579 = CARTESIAN_POINT ( 'NONE',  ( -34.55620429048339304, -23.47593901973091235, -1.443836447539013301 ) ) ;
#98580 = CARTESIAN_POINT ( 'NONE',  ( -69.62287095715005592, -24.64898659630528854, 1.056161002820824368 ) ) ;
#98581 = ORIENTED_EDGE ( 'NONE', *, *, #16120, .F. ) ;
#98582 = EDGE_CURVE ( 'NONE', #77754, #3492, #98871, .T. ) ;
#98583 = LINE ( 'NONE', #4754, #18652 ) ;
#98584 = CARTESIAN_POINT ( 'NONE',  ( -102.5562042904833788, -23.47596703998600631, 11.44779298504227683 ) ) ;
#98585 = VERTEX_POINT ( 'NONE', #5361 ) ;
#98586 = CIRCLE ( 'NONE', #32174, 2.999999999999999112 ) ;
#98587 = ORIENTED_EDGE ( 'NONE', *, *, #60765, .F. ) ;
#98588 = FACE_OUTER_BOUND ( 'NONE', #84715, .T. ) ;
#98589 = CARTESIAN_POINT ( 'NONE',  ( 7.480769230769231726, -6.376774720514420736, 20.77403846153845635 ) ) ;
#98590 = CARTESIAN_POINT ( 'NONE',  ( -76.62361881388403617, -24.65952944569303895, 1.056160979905700792 ) ) ;
#98591 = CARTESIAN_POINT ( 'NONE',  ( -20.44794078217315558, 2.270689272194197805, -1.500000000000002220 ) ) ;
#98592 = EDGE_CURVE ( 'NONE', #25509, #78484, #15443, .T. ) ;
#98593 = CARTESIAN_POINT ( 'NONE',  ( -18.50814150397365410, 11.09706937414969374, 11.49999999999999645 ) ) ;
#98594 = VERTEX_POINT ( 'NONE', #89600 ) ;
#98595 = PLANE ( 'NONE',  #61244 ) ;
#98596 = CARTESIAN_POINT ( 'NONE',  ( -129.6228709571500133, -23.73907113216991860, -1.053371485793220375 ) ) ;
#98597 = CARTESIAN_POINT ( 'NONE',  ( 9.556255610625576935, 20.19728179944524271, 11.49999999999998934 ) ) ;
#98598 = EDGE_CURVE ( 'NONE', #82135, #42245, #25943, .T. ) ;
#98599 = CARTESIAN_POINT ( 'NONE',  ( -79.76746806413464697, -25.27875036686598165, 6.852562602421008009 ) ) ;
#98600 = CARTESIAN_POINT ( 'NONE',  ( -84.60373966623234310, -23.48783264082476308, -1.443836473390094799 ) ) ;
#98601 = ORIENTED_EDGE ( 'NONE', *, *, #99846, .T. ) ;
#98602 = ADVANCED_FACE ( 'NONE', ( #36315 ), #89827, .T. ) ;
#98603 = LINE ( 'NONE', #45336, #48555 ) ;
#98604 = CARTESIAN_POINT ( 'NONE',  ( -8.499999999999987566, 19.99999999999999289, 2.100000000000000089 ) ) ;
#98605 = CIRCLE ( 'NONE', #54878, 1.149999999999998135 ) ;
#98606 = CARTESIAN_POINT ( 'NONE',  ( 20.66465755290784401, -3.126920214821775623, 11.49999999999998934 ) ) ;
#98607 = ORIENTED_EDGE ( 'NONE', *, *, #1964, .T. ) ;
#98609 = ORIENTED_EDGE ( 'NONE', *, *, #69460, .T. ) ;
#98608 = CARTESIAN_POINT ( 'NONE',  ( -67.54911902231192755, -24.15620529776628800, 10.23563542870660115 ) ) ;
#98610 = ORIENTED_EDGE ( 'NONE', *, *, #4247, .F. ) ;
#98611 = CARTESIAN_POINT ( 'NONE',  ( -50.80853080041594438, -25.30058970222920678, 4.652310615611309430 ) ) ;
#98612 = CARTESIAN_POINT ( 'NONE',  ( 9.660767377612277329, -18.76748907076374095, -1.500000000000002220 ) ) ;
#98613 = VERTEX_POINT ( 'NONE', #69756 ) ;
#98614 = CARTESIAN_POINT ( 'NONE',  ( -117.5198302432919633, -23.96119346886881019, -0.6495511937831994764 ) ) ;
#98615 = DIRECTION ( 'NONE',  ( 0.8219392559241306406, -0.08114015731558522904, -0.5637660281018079811 ) ) ;
#98616 = DIRECTION ( 'NONE',  ( 0.000000000000000000, 0.9999999999976377785, 2.173523156925979975E-06 ) ) ;
#98617 = CARTESIAN_POINT ( 'NONE',  ( -17.66201745896767505, 5.965225279485572685, -23.06272557202527906 ) ) ;
#98618 = CARTESIAN_POINT ( 'NONE',  ( 7.460332110455646593, -5.876774720514418071, 20.55293369838740247 ) ) ;
#98619 = CARTESIAN_POINT ( 'NONE',  ( -12.70408864715453667, 17.69581422525067183, -1.500000000000002220 ) ) ;
#98620 = FACE_OUTER_BOUND ( 'NONE', #69776, .T. ) ;
#98622 = VERTEX_POINT ( 'NONE', #85466 ) ;
#98621 = CARTESIAN_POINT ( 'NONE',  ( -15.13915969582853549, -16.40262476207453801, 11.49999999999999645 ) ) ;
#98623 = PLANE ( 'NONE',  #40511 ) ;
#98624 = CARTESIAN_POINT ( 'NONE',  ( -9.278253834636473130, -6.376774720514426953, 18.21871304725684482 ) ) ;
#98625 = DIRECTION ( 'NONE',  ( 0.000000000000000000, 0.000000000000000000, 1.000000000000000000 ) ) ;
#98626 = VERTEX_POINT ( 'NONE', #38296 ) ;
#98627 = VERTEX_POINT ( 'NONE', #61164 ) ;
#98628 = EDGE_LOOP ( 'NONE', ( #99914, #35917, #82249, #49606 ) ) ;
#98629 = CARTESIAN_POINT ( 'NONE',  ( -95.62287095715005592, -24.99156045073393173, 7.747789690856161648 ) ) ;
#98630 = LINE ( 'NONE', #6292, #87090 ) ;
#98631 = CARTESIAN_POINT ( 'NONE',  ( 8.376690734369038438, 12.50000000000004974, 0.000000000000000000 ) ) ;
#98632 = CARTESIAN_POINT ( 'NONE',  ( -13.43510958081001050, -13.94331287200543024, 11.49999999999998934 ) ) ;
#98633 = DIRECTION ( 'NONE',  ( -0.000000000000000000, -0.000000000000000000, -1.000000000000000000 ) ) ;
#98634 = ORIENTED_EDGE ( 'NONE', *, *, #43978, .T. ) ;
#98635 = AXIS2_PLACEMENT_3D ( 'NONE', #57787, #41058, #17210 ) ;
#98636 = CARTESIAN_POINT ( 'NONE',  ( -18.68671320864135765, 5.291888989699490509, 11.49999999999999645 ) ) ;
#98637 = CARTESIAN_POINT ( 'NONE',  ( -0.02075734969026423599, 5.965225279485572685, -0.08597719988137648983 ) ) ;
#98638 = AXIS2_PLACEMENT_3D ( 'NONE', #2265, #49443, #73271 ) ;
#98639 = B_SPLINE_CURVE_WITH_KNOTS ( 'NONE', 3,
 ( #31826, #93210, #69384, #92705, #55177, #23194 ),
 .UNSPECIFIED., .F., .F.,
 ( 4, 2, 4 ),
 ( 6.384118678620645382E-06, 0.001386860460828382357, 0.002767336802978144061 ),
 .UNSPECIFIED. ) ;
#98640 = ORIENTED_EDGE ( 'NONE', *, *, #25636, .T. ) ;
#98641 = CARTESIAN_POINT ( 'NONE',  ( -53.62287095715005592, -29.50247984919015209, -1.443849546365058689 ) ) ;
#98642 = CARTESIAN_POINT ( 'NONE',  ( 3.632744579681756569, -5.876774720514403860, 18.17103827887095946 ) ) ;
#98643 = CARTESIAN_POINT ( 'NONE',  ( -102.6228709571500843, -24.51283580621365132, 0.6167428607019762588 ) ) ;
#98644 = VECTOR ( 'NONE', #81528, 1000.000000000000114 ) ;
#98645 = CARTESIAN_POINT ( 'NONE',  ( -130.5728709571500588, -24.04668586515358797, 10.47594215909545312 ) ) ;
#98646 = CARTESIAN_POINT ( 'NONE',  ( -14.21210043416151159, 13.53504130633199765, 11.49999999999998934 ) ) ;
#98647 = CARTESIAN_POINT ( 'NONE',  ( -46.50019354166188634, -24.15543982623906771, -0.2315651400026683127 ) ) ;
#98648 = ORIENTED_EDGE ( 'NONE', *, *, #10014, .T. ) ;
#98649 = CARTESIAN_POINT ( 'NONE',  ( 21.55061338234859392, -0.003183148592148328428, -1.500000000000002220 ) ) ;
#98650 = AXIS2_PLACEMENT_3D ( 'NONE', #54016, #6824, #99654 ) ;
#98651 = CARTESIAN_POINT ( 'NONE',  ( -33.59406827596458811, -24.15620529776627379, 10.23563542870661536 ) ) ;
#98652 = CARTESIAN_POINT ( 'NONE',  ( -70.51930845923730828, -25.25639598314407408, 7.087032433890202654 ) ) ;
#98653 = CARTESIAN_POINT ( 'NONE',  ( -40.52195335486641881, -23.48783264082477018, -1.443836473390102793 ) ) ;
#98654 = CARTESIAN_POINT ( 'NONE',  ( -99.54260921963015107, -25.27473344898619700, 3.861216578678491995 ) ) ;
#98655 = CARTESIAN_POINT ( 'NONE',  ( -22.04953120734539240, -6.464106996104416858, -1.500000000000002220 ) ) ;
#98656 = B_SPLINE_CURVE_WITH_KNOTS ( 'NONE', 3,
 ( #65933, #49700, #88754, #96852, #80629, #65437 ),
 .UNSPECIFIED., .F., .F.,
 ( 4, 2, 4 ),
 ( 1.570887131794952276E-05, 0.001396322306279764325, 0.002776935741241578874 ),
 .UNSPECIFIED. ) ;
#98657 = ADVANCED_FACE ( 'NONE', ( #37806 ), #16450, .T. ) ;
#98658 = PERSON_AND_ORGANIZATION ( #70597, #27821 ) ;
#98659 = FACE_OUTER_BOUND ( 'NONE', #2705, .T. ) ;
#98660 = CARTESIAN_POINT ( 'NONE',  ( -88.92287095715005307, -23.47596703998600631, 11.44779298504227860 ) ) ;
#98661 = CARTESIAN_POINT ( 'NONE',  ( -10.68008619461380704, -17.10268970254769982, 11.49999999999999645 ) ) ;
#98662 = CARTESIAN_POINT ( 'NONE',  ( -45.62287095715004881, -24.51254535404255819, 9.355368623467651190 ) ) ;
#98663 = CYLINDRICAL_SURFACE ( 'NONE', #43441, 130.2784398600581710 ) ;
#98664 = AXIS2_PLACEMENT_3D ( 'NONE', #44054, #61293, #67401 ) ;
#98665 = DIRECTION ( 'NONE',  ( 0.000000000000000000, 0.9999999999976377785, 2.173523156925979975E-06 ) ) ;
#98666 = CARTESIAN_POINT ( 'NONE',  ( -53.62287095715005592, -29.50250786944525672, 11.44777988621624054 ) ) ;
#98667 = CARTESIAN_POINT ( 'NONE',  ( -38.58953762381673158, -24.64898659630528144, 1.056161002820817707 ) ) ;
#98668 = CARTESIAN_POINT ( 'NONE',  ( 7.211006999188390942, 18.53272205163514030, 11.49999999999998934 ) ) ;
#98670 = EDGE_CURVE ( 'NONE', #89848, #21078, #2176, .T. ) ;
#98669 = CARTESIAN_POINT ( 'NONE',  ( -82.62287095715005592, -24.64965695001468404, 8.947790433994182280 ) ) ;
#98671 = CARTESIAN_POINT ( 'NONE',  ( 18.46520180437041603, 7.126043738416648843, -1.500000000000002220 ) ) ;
#98672 = ADVANCED_FACE ( 'NONE', ( #77841 ), #74434, .T. ) ;
#98673 = CARTESIAN_POINT ( 'NONE',  ( -126.5905543067551946, -23.73791477778912551, 11.05961554403169878 ) ) ;
#98674 = EDGE_CURVE ( 'NONE', #87827, #38848, #74746, .T. ) ;
#98676 = EDGE_CURVE ( 'NONE', #4757, #78143, #21079, .T. ) ;
#98675 = UNCERTAINTY_MEASURE_WITH_UNIT (LENGTH_MEASURE( 1.000000000000000082E-05 ), #84581, 'distance_accuracy_value', 'NONE');
#98677 = CARTESIAN_POINT ( 'NONE',  ( 28.20688450243577705, 5.356774720514425603, -7.073367244511738150 ) ) ;
#98678 = DIRECTION ( 'NONE',  ( -1.000000000000000000, 0.000000000000000000, 1.333806637208504346E-15 ) ) ;
#98679 = CARTESIAN_POINT ( 'NONE',  ( -20.55277978778089576, -2.218614319624547360, 11.49999999999999645 ) ) ;
#98680 = DIRECTION ( 'NONE',  ( -2.352173255807804438E-16, 2.352173255807796056E-16, 1.000000000000000000 ) ) ;
#98681 = FACE_OUTER_BOUND ( 'NONE', #53365, .T. ) ;
#98682 = DIRECTION ( 'NONE',  ( 0.000000000000000000, 1.000000000000000000, -0.000000000000000000 ) ) ;
#98683 = VECTOR ( 'NONE', #64770, 1000.000000000000000 ) ;
#98684 = CARTESIAN_POINT ( 'NONE',  ( -19.63924127562733446, 11.44998032699685631, 11.49999999999999645 ) ) ;
#98685 = ORIENTED_EDGE ( 'NONE', *, *, #73662, .T. ) ;
#98686 = CARTESIAN_POINT ( 'NONE',  ( -46.62287095715003460, -23.96177878511308634, 10.65340807706330217 ) ) ;
#98687 = CARTESIAN_POINT ( 'NONE',  ( 29.76216731806157867, 5.356774720514427379, 26.42665638500616154 ) ) ;
#98688 = CARTESIAN_POINT ( 'NONE',  ( -9.895454706725905325, 17.58729670687104729, 11.49999999999998934 ) ) ;
#98689 = EDGE_CURVE ( 'NONE', #56235, #49308, #88073, .T. ) ;
#98690 = PLANE ( 'NONE',  #40298 ) ;
#98691 = DIRECTION ( 'NONE',  ( -0.000000000000000000, 1.000000000000000000, -0.000000000000000000 ) ) ;
#98692 = ORIENTED_EDGE ( 'NONE', *, *, #47865, .T. ) ;
#98693 = B_SPLINE_CURVE_WITH_KNOTS ( 'NONE', 3,
 ( #71244, #1733, #32672, #62135, #46902, #86957 ),
 .UNSPECIFIED., .F., .F.,
 ( 4, 2, 4 ),
 ( 0.000000000000000000, 0.001380901958385390930, 0.002761803916770781860 ),
 .UNSPECIFIED. ) ;
#98694 = B_SPLINE_CURVE_WITH_KNOTS ( 'NONE', 3,
 ( #99763, #45020, #44006, #74938 ),
 .UNSPECIFIED., .F., .F.,
 ( 4, 4 ),
 ( 0.000000000000000000, 9.999999999993348899E-05 ),
 .UNSPECIFIED. ) ;
#98695 = ORIENTED_EDGE ( 'NONE', *, *, #3203, .F. ) ;
#98696 = EDGE_CURVE ( 'NONE', #97749, #95734, #18960, .T. ) ;
#98697 = CARTESIAN_POINT ( 'NONE',  ( -29.49875734969025842, -5.965225279485572685, 15.62202280011862321 ) ) ;
#98698 = CARTESIAN_POINT ( 'NONE',  ( 5.898633191892585614, -22.09092271590295198, -1.500000000000002220 ) ) ;
#98699 = CARTESIAN_POINT ( 'NONE',  ( -29.62068022372628917, -23.40854978123364560, -1.443836171194816886 ) ) ;
#98700 = CARTESIAN_POINT ( 'NONE',  ( 21.48638754631891246, 1.654510534108022179, -1.500000000000002220 ) ) ;
#98701 = CARTESIAN_POINT ( 'NONE',  ( -59.62287095715004881, -29.50248528299804818, 1.056150453629034924 ) ) ;
#98702 = CARTESIAN_POINT ( 'NONE',  ( -3.108974358974355923, -6.376774720514427841, 21.75000000000001066 ) ) ;
#98703 = CARTESIAN_POINT ( 'NONE',  ( -21.23328875057882570, -7.520457577684837247, 11.49999999999999645 ) ) ;
#98704 = ORIENTED_EDGE ( 'NONE', *, *, #58109, .F. ) ;
#98705 = CARTESIAN_POINT ( 'NONE',  ( -43.52287095715004028, -24.34917612407033616, 0.1852690917477757548 ) ) ;
#98706 = CARTESIAN_POINT ( 'NONE',  ( 3.689792033372774060, 21.67897595795444587, 11.49999999999998934 ) ) ;
#98707 = EDGE_CURVE ( 'NONE', #44563, #82569, #23892, .T. ) ;
#98708 = LINE ( 'NONE', #30191, #80281 ) ;
#98709 = CARTESIAN_POINT ( 'NONE',  ( -99.62287095715005592, -29.50250243563736774, 8.947779886222138046 ) ) ;
#98710 = ORIENTED_EDGE ( 'NONE', *, *, #61400, .F. ) ;
#98711 = CARTESIAN_POINT ( 'NONE',  ( 4.782775879418006859, -6.376774720514406525, 18.83817099474236656 ) ) ;
#98712 = CARTESIAN_POINT ( 'NONE',  ( -90.51170739371271168, -24.15602025860896163, 10.28564288303535434 ) ) ;
#98713 = EDGE_LOOP ( 'NONE', ( #13749, #54348, #83245, #41576 ) ) ;
#98714 = PLANE ( 'NONE',  #72827 ) ;
#98715 = ORIENTED_EDGE ( 'NONE', *, *, #70596, .F. ) ;
#98716 = VECTOR ( 'NONE', #45803, 1000.000000000000000 ) ;
#98717 = VERTEX_POINT ( 'NONE', #34200 ) ;
#98718 = DIRECTION ( 'NONE',  ( 0.000000000000000000, -0.000000000000000000, -1.000000000000000000 ) ) ;
#98719 = CARTESIAN_POINT ( 'NONE',  ( -61.52287095715006160, -24.64898659630367916, 1.056161002820822592 ) ) ;
#98720 = CARTESIAN_POINT ( 'NONE',  ( -104.5976497916026915, -23.48786465467241413, 11.44779295918254469 ) ) ;
#98721 = CARTESIAN_POINT ( 'NONE',  ( 3.609400094169940676, -20.08663944828865766, -1.500000000000002220 ) ) ;
#98722 = EDGE_CURVE ( 'NONE', #20944, #55041, #40799, .T. ) ;
#98723 = ORIENTED_EDGE ( 'NONE', *, *, #30131, .T. ) ;
#98724 = CARTESIAN_POINT ( 'NONE',  ( -0.5315124411682757843, -5.876774720514411854, 19.46509473978807847 ) ) ;
#98725 = VECTOR ( 'NONE', #99969, 1000.000000000000000 ) ;
#98726 = CARTESIAN_POINT ( 'NONE',  ( -65.62287095715005592, -29.50249982740957577, 7.747779886224967605 ) ) ;
#98727 = EDGE_CURVE ( 'NONE', #18610, #41555, #83197, .T. ) ;
#98728 = CARTESIAN_POINT ( 'NONE',  ( 3.509873074917118085, 0.3587747205144265483, 29.15869884040363758 ) ) ;
#98729 = CARTESIAN_POINT ( 'NONE',  ( -51.52287095715006870, -24.64965694238407323, 8.947790433994203596 ) ) ;
#98730 = ORIENTED_EDGE ( 'NONE', *, *, #89843, .F. ) ;
#98731 = CARTESIAN_POINT ( 'NONE',  ( 30.93860345374796594, 0.6647747205144264315, 19.84760796525321780 ) ) ;
#98732 = AXIS2_PLACEMENT_3D ( 'NONE', #7357, #252, #23575 ) ;
#98733 = CARTESIAN_POINT ( 'NONE',  ( 12.40597316965629560, -5.152774720514427642, -26.28458722401733993 ) ) ;
#98734 = AXIS2_PLACEMENT_3D ( 'NONE', #76217, #95961, #18827 ) ;
#98735 = CARTESIAN_POINT ( 'NONE',  ( 17.18838054715250152, -11.71887806637979779, -1.500000000000002220 ) ) ;
#98736 = EDGE_CURVE ( 'NONE', #93999, #98531, #22733, .T. ) ;
#98737 = ORIENTED_EDGE ( 'NONE', *, *, #82755, .T. ) ;
#98739 = VERTEX_POINT ( 'NONE', #73262 ) ;
#98738 = CARTESIAN_POINT ( 'NONE',  ( 4.547289707988324103, -6.376774720514410077, 19.12266226838056582 ) ) ;
#98740 = VECTOR ( 'NONE', #54844, 1000.000000000000000 ) ;
#98741 = DIRECTION ( 'NONE',  ( 0.000000000000000000, 0.000000000000000000, 1.000000000000000000 ) ) ;
#98742 = VERTEX_POINT ( 'NONE', #86473 ) ;
#98743 = VERTEX_POINT ( 'NONE', #94585 ) ;
#98744 = DIRECTION ( 'NONE',  ( -3.773278334453079618E-23, 0.9999999999976377785, 2.173523156925979975E-06 ) ) ;
#98745 = PLANE ( 'NONE',  #67544 ) ;
#98746 = CARTESIAN_POINT ( 'NONE',  ( -52.62287095715005592, -24.66019654487199020, 8.947790411086135265 ) ) ;
#98747 = CARTESIAN_POINT ( 'NONE',  ( -61.62287095715004881, -24.64965695001468404, 8.947790433994185832 ) ) ;
#98749 = ORIENTED_EDGE ( 'NONE', *, *, #45493, .T. ) ;
#98748 = CARTESIAN_POINT ( 'NONE',  ( -21.57569705560537088, 4.917917830663471435, 11.49999999999999645 ) ) ;
#98750 = CARTESIAN_POINT ( 'NONE',  ( 30.93860345374796594, -0.6647747205144264315, 20.86760796525322093 ) ) ;
#98751 = CARTESIAN_POINT ( 'NONE',  ( 3.867644355387967359, 22.30990608135428488, -1.500000000000002220 ) ) ;
#98753 = EDGE_LOOP ( 'NONE', ( #71155, #79848, #50591, #97629 ) ) ;
#98752 = CARTESIAN_POINT ( 'NONE',  ( 8.160000000000000142, 8.793627758918228565, -2.994553991265763049 ) ) ;
#98754 = ORIENTED_EDGE ( 'NONE', *, *, #60696, .F. ) ;
#98755 = CARTESIAN_POINT ( 'NONE',  ( 8.071512145086499501, -1.028487854913504584, 5.500000000000000000 ) ) ;
#98756 = CARTESIAN_POINT ( 'NONE',  ( -7.184633862932894743, 18.80532529184710100, -1.500000000000002220 ) ) ;
#98757 = B_SPLINE_SURFACE_WITH_KNOTS ( 'NONE', 3, 1, ( 
 ( #6480, #98313 ),
 ( #67893, #89723 ),
 ( #52653, #28816 ),
 ( #20193, #51158 ),
 ( #43551, #68382 ) ),
 .UNSPECIFIED., .F., .F., .F.,
 ( 4, 1, 4 ),
 ( 2, 2 ),
 ( 0.000000000000000000, 0.5126593363417764060, 1.000000000000000000 ),
 ( 0.000000000000000000, 1.000000000000000000 ),
 .UNSPECIFIED. ) ;
#98758 = LINE ( 'NONE', #29250, #3603 ) ;
#98759 = ORIENTED_EDGE ( 'NONE', *, *, #43912, .F. ) ;
#98760 = CARTESIAN_POINT ( 'NONE',  ( -40.41373532093560073, -25.30507957900415050, 5.542204897518816509 ) ) ;
#98761 = CARTESIAN_POINT ( 'NONE',  ( 22.01400519847025450, -3.885951517071169370, -1.500000000000002220 ) ) ;
#98762 = ORIENTED_EDGE ( 'NONE', *, *, #99366, .T. ) ;
#98763 = ORIENTED_EDGE ( 'NONE', *, *, #38530, .T. ) ;
#98764 = CARTESIAN_POINT ( 'NONE',  ( -5.314757719055156038, -6.376774720514411854, 19.55912026249540858 ) ) ;
#98765 = CARTESIAN_POINT ( 'NONE',  ( -89.62287095715004170, -23.47596703998600631, 11.44779298504227860 ) ) ;
#98766 = CARTESIAN_POINT ( 'NONE',  ( -26.49992872176817826, -24.62748876299636436, 2.056831902527120004 ) ) ;
#98767 = CARTESIAN_POINT ( 'NONE',  ( -99.62287095715005592, -24.64898659630367916, 1.056161002820829697 ) ) ;
#98768 = CARTESIAN_POINT ( 'NONE',  ( 19.26631176993168282, 3.279242639417544236, -1.500000000000002220 ) ) ;
#98769 = DIRECTION ( 'NONE',  ( -0.9994733861282923959, 0.000000000000000000, -0.03244919754393515293 ) ) ;
#98770 = CARTESIAN_POINT ( 'NONE',  ( 11.86944616785735818, -17.87650476368427732, 11.49999999999998934 ) ) ;
#98771 = CARTESIAN_POINT ( 'NONE',  ( -25.81533462945560942, -24.92774974205095972, 3.045126989538161855 ) ) ;
#98772 = CARTESIAN_POINT ( 'NONE',  ( -108.6228709571500559, -29.50250243563736774, 8.947779886222136270 ) ) ;
#98773 = CARTESIAN_POINT ( 'NONE',  ( -115.5895376238167387, -24.99132157543166954, 2.256160258750668390 ) ) ;
#98774 = AXIS2_PLACEMENT_3D ( 'NONE', #31390, #8554, #62351 ) ;
#98775 = CARTESIAN_POINT ( 'NONE',  ( 17.58993269669914383, -14.52173041563253975, -1.500000000000002220 ) ) ;
#98776 = COORDINATED_UNIVERSAL_TIME_OFFSET ( 0, 0, .AHEAD. ) ;
#98777 = CARTESIAN_POINT ( 'NONE',  ( -96.62764419480109268, -24.35071581493543391, 9.817618358456023486 ) ) ;
#98778 = PLANE ( 'NONE',  #83041 ) ;
#98779 = CARTESIAN_POINT ( 'NONE',  ( 13.87436705529610492, 14.39054836566213780, 11.49999999999999645 ) ) ;
#98780 = CARTESIAN_POINT ( 'NONE',  ( -111.5895376238167245, -23.47593901973091235, -1.443836447538999312 ) ) ;
#98781 = EDGE_CURVE ( 'NONE', #7141, #91541, #14183, .T. ) ;
#98782 = AXIS2_PLACEMENT_3D ( 'NONE', #27724, #66805, #98718 ) ;
#98783 = EDGE_CURVE ( 'NONE', #59400, #65117, #91642, .T. ) ;
#98784 = DIRECTION ( 'NONE',  ( 1.000000000000000000, 3.773278334444167608E-23, 8.201307833595939069E-29 ) ) ;
#98785 = DIRECTION ( 'NONE',  ( 3.773278334444167020E-23, -1.000000000000000000, 0.000000000000000000 ) ) ;
#98786 = ORIENTED_EDGE ( 'NONE', *, *, #17875, .T. ) ;
#98787 = DIRECTION ( 'NONE',  ( 0.5656310827093757876, 0.8246584009594636333, 1.161164194647626634E-16 ) ) ;
#98788 = CARTESIAN_POINT ( 'NONE',  ( -100.4381051993576364, -25.12049752546738191, 2.832404795212222215 ) ) ;
#98789 = EDGE_CURVE ( 'NONE', #9886, #84887, #56548, .T. ) ;
#98790 = CARTESIAN_POINT ( 'NONE',  ( 10.83000837110471082, 18.85367679709202804, 11.49999999999998934 ) ) ;
#98791 = CARTESIAN_POINT ( 'NONE',  ( -29.49875734969025842, -5.965225279485572685, 17.86602280011862476 ) ) ;
#98792 = VECTOR ( 'NONE', #53474, 1000.000000000000000 ) ;
#98793 = CARTESIAN_POINT ( 'NONE',  ( 13.97609912898263573, 13.72534901313461653, -1.500000000000002220 ) ) ;
#98794 = EDGE_CURVE ( 'NONE', #908, #35380, #8082, .T. ) ;
#98795 = CARTESIAN_POINT ( 'NONE',  ( -99.77553290276979681, -25.16026440777957873, 6.940667289341870827 ) ) ;
#98797 = ORIENTED_EDGE ( 'NONE', *, *, #75302, .T. ) ;
#98796 = CIRCLE ( 'NONE', #38829, 130.2784398600581710 ) ;
#98798 = CONTEXT_DEPENDENT_SHAPE_REPRESENTATION ( #28460, #18225 ) ;
#98799 = VECTOR ( 'NONE', #33556, 1000.000000000000000 ) ;
#98800 = CARTESIAN_POINT ( 'NONE',  ( -40.62287095715005592, -23.47596703998600276, 11.44779298504227505 ) ) ;
#98801 = CARTESIAN_POINT ( 'NONE',  ( 3.552327343495968570, -6.376774720514427841, 21.81288606793570395 ) ) ;
#98802 = CARTESIAN_POINT ( 'NONE',  ( -1.764913036440812322, 20.45846032914734280, 11.49999999999999645 ) ) ;
#98803 = CARTESIAN_POINT ( 'NONE',  ( -83.62287095715007013, -24.66019654487199730, 8.947790411086126383 ) ) ;
#98804 = CARTESIAN_POINT ( 'NONE',  ( -42.55620429048337883, -24.66019654487199375, 8.947790411086135265 ) ) ;
#98805 = CIRCLE ( 'NONE', #93950, 1.050000000000000488 ) ;
#98806 = ADVANCED_FACE ( 'NONE', ( #74250 ), #21436, .T. ) ;
#98807 = ORIENTED_EDGE ( 'NONE', *, *, #16911, .T. ) ;
#98808 = LINE ( 'NONE', #76961, #15135 ) ;
#98809 = CARTESIAN_POINT ( 'NONE',  ( -84.52287095715006160, -29.50247984919015209, -1.443849546365053582 ) ) ;
#98810 = LINE ( 'NONE', #67880, #75975 ) ;
#98811 = CARTESIAN_POINT ( 'NONE',  ( 27.53860345374808105, -5.356774720496559894, 19.84760796525321425 ) ) ;
#98812 = EDGE_LOOP ( 'NONE', ( #82747, #40858, #63500, #54087 ) ) ;
#98813 = FACE_OUTER_BOUND ( 'NONE', #89123, .T. ) ;
#98814 = CARTESIAN_POINT ( 'NONE',  ( -12.06219892284564388, 19.56905390912838172, 11.49999999999999645 ) ) ;
#98815 = CARTESIAN_POINT ( 'NONE',  ( -18.67006117854901959, 13.05921059288911934, 11.49999999999998934 ) ) ;
#98816 = CARTESIAN_POINT ( 'NONE',  ( 32.45853543194704116, -0.3587747205144265483, 9.169203677920338080 ) ) ;
#98817 = B_SPLINE_CURVE_WITH_KNOTS ( 'NONE', 3,
 ( #31068, #29577, #69138, #14842 ),
 .UNSPECIFIED., .F., .F.,
 ( 4, 4 ),
 ( 0.000000000000000000, 0.0001000000000000028644 ),
 .UNSPECIFIED. ) ;
#98818 = CARTESIAN_POINT ( 'NONE',  ( -5.378122165843598701, -6.376774720514410077, 19.21968329462762526 ) ) ;
#98819 = CARTESIAN_POINT ( 'NONE',  ( -49.62291167701152261, -25.23900015727310020, 3.638722386798801445 ) ) ;
#98820 = CARTESIAN_POINT ( 'NONE',  ( -40.52287095715009002, -23.85229601348996198, 10.88205029486209874 ) ) ;
#98821 = CARTESIAN_POINT ( 'NONE',  ( -110.5518296883100362, -24.52300882791530512, 0.6510814631126329299 ) ) ;
#98822 = CARTESIAN_POINT ( 'NONE',  ( 21.74639208212181529, -2.611101805624240768, 11.49999999999998934 ) ) ;
#98823 = PLANE ( 'NONE',  #51103 ) ;
#98824 = CARTESIAN_POINT ( 'NONE',  ( -87.55130102961774696, -24.15620529776628445, 10.23563542870660292 ) ) ;
#98825 = CARTESIAN_POINT ( 'NONE',  ( 8.978253834636468866, -5.876774720514426953, 21.48128695274316158 ) ) ;
#98826 = CARTESIAN_POINT ( 'NONE',  ( -78.51253566907887205, -23.96119346886880308, -0.6495511937832113558 ) ) ;
#98827 = CARTESIAN_POINT ( 'NONE',  ( -103.5895376238167103, -24.65952944569305316, 1.056160979905702790 ) ) ;
#98828 = CARTESIAN_POINT ( 'NONE',  ( -86.62287095715004170, -24.64965695001468404, 8.947790433994180503 ) ) ;
#98829 = ORIENTED_EDGE ( 'NONE', *, *, #97562, .T. ) ;
#98830 = CARTESIAN_POINT ( 'NONE',  ( 11.41020680648336771, 16.95828056793917682, 11.49999999999998934 ) ) ;
#98831 = ORIENTED_EDGE ( 'NONE', *, *, #69011, .F. ) ;
#98832 = ORIENTED_EDGE ( 'NONE', *, *, #16073, .T. ) ;
#98833 = ORIENTED_EDGE ( 'NONE', *, *, #71117, .F. ) ;
#98834 = ORIENTED_EDGE ( 'NONE', *, *, #98918, .T. ) ;
#98835 = CARTESIAN_POINT ( 'NONE',  ( -16.13607370526515794, 16.44073208242836159, 11.49999999999998934 ) ) ;
#98836 = CARTESIAN_POINT ( 'NONE',  ( -35.52287095715006160, -23.85196035787604174, -0.8779234886343784128 ) ) ;
#98837 = CARTESIAN_POINT ( 'NONE',  ( -12.21837793623082113, -16.16665877782589433, -1.500000000000002220 ) ) ;
#98838 = ORIENTED_EDGE ( 'NONE', *, *, #68557, .F. ) ;
#98839 = CARTESIAN_POINT ( 'NONE',  ( -28.20653904363605236, -25.02819912641725963, 6.759032221908313431 ) ) ;
#98840 = CARTESIAN_POINT ( 'NONE',  ( -87.62287095715004170, -24.66019654487199020, 8.947790411086129936 ) ) ;
#98841 = EDGE_CURVE ( 'NONE', #21630, #63898, #59532, .T. ) ;
#98842 = CARTESIAN_POINT ( 'NONE',  ( -89.81226385320383088, -25.27367468601175204, 3.993462154588550916 ) ) ;
#98843 = CARTESIAN_POINT ( 'NONE',  ( -70.51358761491228222, -23.85016227208580730, -0.8807180028928335291 ) ) ;
#98845 = ORIENTED_EDGE ( 'NONE', *, *, #80426, .T. ) ;
#98844 = CARTESIAN_POINT ( 'NONE',  ( 21.40653236543258231, -1.377805879665675803, 11.49999999999999645 ) ) ;
#98846 = LINE ( 'NONE', #14108, #33840 ) ;
#98847 = CARTESIAN_POINT ( 'NONE',  ( -41.48142716432091248, -24.65952944569304606, 1.056160979905696351 ) ) ;
#98848 = EDGE_LOOP ( 'NONE', ( #34548, #44080, #99228, #51574 ) ) ;
#98849 = CARTESIAN_POINT ( 'NONE',  ( 2.909938941155331360, -20.50406750007545398, 11.49999999999998934 ) ) ;
#98851 = EDGE_CURVE ( 'NONE', #61485, #79708, #81863, .T. ) ;
#98850 = VECTOR ( 'NONE', #49452, 1000.000000000000114 ) ;
#98852 = B_SPLINE_CURVE_WITH_KNOTS ( 'NONE', 3,
 ( #13379, #100094, #76275, #44359 ),
 .UNSPECIFIED., .F., .F.,
 ( 4, 4 ),
 ( 0.01980006321810323308, 0.02880649449021864886 ),
 .UNSPECIFIED. ) ;
#98853 = ORIENTED_EDGE ( 'NONE', *, *, #55536, .T. ) ;
#98854 = CARTESIAN_POINT ( 'NONE',  ( -28.57182946747713359, -23.32753131072699304, -1.443835813551990865 ) ) ;
#98855 = ORIENTED_EDGE ( 'NONE', *, *, #60820, .F. ) ;
#98856 = CARTESIAN_POINT ( 'NONE',  ( 4.263585034174699473, -6.376774720514402972, 18.26968045024142739 ) ) ;
#98857 = AXIS2_PLACEMENT_3D ( 'NONE', #44327, #43329, #49955 ) ;
#98858 = ORIENTED_EDGE ( 'NONE', *, *, #80758, .T. ) ;
#98859 = CARTESIAN_POINT ( 'NONE',  ( -5.413507703253908510, 20.27406835261982465, -1.500000000000002220 ) ) ;
#98860 = CARTESIAN_POINT ( 'NONE',  ( 1.885617179787854036, 21.85875792104173598, 11.49999999999999645 ) ) ;
#98861 = LINE ( 'NONE', #13123, #977 ) ;
#98862 = VECTOR ( 'NONE', #65535, 1000.000000000000114 ) ;
#98863 = CARTESIAN_POINT ( 'NONE',  ( 22.10748686624256720, -4.471405416651531795, 11.49999999999998934 ) ) ;
#98864 = CARTESIAN_POINT ( 'NONE',  ( -16.09219062524700661, 13.46031615953476468, 11.49999999999998934 ) ) ;
#98865 = CARTESIAN_POINT ( 'NONE',  ( -111.5228709571500616, -24.64898659630368627, 1.056161002820831474 ) ) ;
#98866 = CARTESIAN_POINT ( 'NONE',  ( -96.62287095715005592, -29.50248528299804818, 1.056150453629042030 ) ) ;
#98867 = CARTESIAN_POINT ( 'NONE',  ( 6.251785340501501587, -6.376774720514424288, 21.46941214867599612 ) ) ;
#98868 = ORIENTED_EDGE ( 'NONE', *, *, #8595, .T. ) ;
#98869 = AXIS2_PLACEMENT_3D ( 'NONE', #18765, #89289, #47855 ) ;
#98870 = ORIENTED_EDGE ( 'NONE', *, *, #42845, .T. ) ;
#98871 = CIRCLE ( 'NONE', #56822, 129.7684398600581517 ) ;
#98872 = ORIENTED_EDGE ( 'NONE', *, *, #48098, .T. ) ;
#98873 = CARTESIAN_POINT ( 'NONE',  ( -66.64100815734259697, -23.96119346886880308, -0.6495511937832151306 ) ) ;
#98874 = B_SPLINE_CURVE_WITH_KNOTS ( 'NONE', 3,
 ( #95741, #25727, #56703, #19605, #26731, #51072, #27730, #10000, #18606, #2912, #96247, #66313, #50079, #33841, #42475, #88636 ),
 .UNSPECIFIED., .F., .F.,
 ( 4, 2, 2, 2, 2, 2, 2, 4 ),
 ( 7.059813062317230268E-18, 0.0002422919684164868688, 0.0004845839368329666903, 0.0009691678736659256827, 0.001211459842082404908, 0.001453751810498883808, 0.001696043778915362924, 0.001938335747331841824 ),
 .UNSPECIFIED. ) ;
#98875 = VECTOR ( 'NONE', #5297, 1000.000000000000114 ) ;
#98876 = CARTESIAN_POINT ( 'NONE',  ( -7.320277434469578459, 20.25297033093062282, -1.500000000000002220 ) ) ;
#98877 = AXIS2_PLACEMENT_3D ( 'NONE', #40446, #85603, #62288 ) ;
#98878 = DIRECTION ( 'NONE',  ( -0.000000000000000000, -0.000000000000000000, -1.000000000000000000 ) ) ;
#98879 = VERTEX_POINT ( 'NONE', #43804 ) ;
#98880 = CARTESIAN_POINT ( 'NONE',  ( 1.943494986365726485, -21.02143711168614004, -1.500000000000002220 ) ) ;
#98881 = DIRECTION ( 'NONE',  ( 0.000000000000000000, -1.000000000000000000, 0.000000000000000000 ) ) ;
#98882 = CARTESIAN_POINT ( 'NONE',  ( -130.2562042904833675, -23.47593901973090524, -1.443836447538995982 ) ) ;
#98883 = CARTESIAN_POINT ( 'NONE',  ( -83.55086462815660298, -24.15620529776628089, 10.23563542870660470 ) ) ;
#98884 = DIRECTION ( 'NONE',  ( 1.000000000000000000, 1.387778780781445429E-16, 0.000000000000000000 ) ) ;
#98885 = CARTESIAN_POINT ( 'NONE',  ( -99.30982394651951495, -25.19814257758587672, 3.382988130124507276 ) ) ;
#98886 = CARTESIAN_POINT ( 'NONE',  ( 2.303347834742990763, 21.97011321758780866, -1.500000000000002220 ) ) ;
#98887 = CARTESIAN_POINT ( 'NONE',  ( -30.48634990730260341, -23.47593902148418010, -1.443029787961928267 ) ) ;
#98888 = EDGE_LOOP ( 'NONE', ( #88786, #79040, #19616, #92334 ) ) ;
#98889 = CARTESIAN_POINT ( 'NONE',  ( -109.2061753004840057, -25.30575712527984678, 4.991482944917066789 ) ) ;
#98890 = CARTESIAN_POINT ( 'NONE',  ( -79.62287095715004170, -24.50216790748205042, 0.6166512839542579449 ) ) ;
#98891 = CARTESIAN_POINT ( 'NONE',  ( -57.62287095715004881, -29.50250243563736774, 8.947779886222145151 ) ) ;
#98892 = CARTESIAN_POINT ( 'NONE',  ( -100.5972946370290231, -23.85016227208580020, -0.8807180028928295323 ) ) ;
#98893 = CARTESIAN_POINT ( 'NONE',  ( -7.106217341473486826, 18.08270997100935418, -1.500000000000002220 ) ) ;
#98894 = CARTESIAN_POINT ( 'NONE',  ( 20.27498964588844643, 6.839650151297337999, 11.49999999999998934 ) ) ;
#98895 = CARTESIAN_POINT ( 'NONE',  ( -26.09764195947040477, -24.97014115428614289, 5.074844938448132226 ) ) ;
#98896 = CARTESIAN_POINT ( 'NONE',  ( -81.58953762381672448, -23.48786465467241058, 11.44779295918254647 ) ) ;
#98897 = CARTESIAN_POINT ( 'NONE',  ( -108.8968792378191921, -25.05712065398430966, 7.447789548358837663 ) ) ;
#98898 = LINE ( 'NONE', #5060, #11962 ) ;
#98899 = CARTESIAN_POINT ( 'NONE',  ( 20.48348528492645571, -9.684159049092739835, -1.500000000000002220 ) ) ;
#98900 = ORIENTED_EDGE ( 'NONE', *, *, #52589, .F. ) ;
#98901 = CARTESIAN_POINT ( 'NONE',  ( 27.53860345374808105, -5.356774720514427379, 1.647607965253214291 ) ) ;
#98902 = DIRECTION ( 'NONE',  ( 0.8788171126619707119, -0.4771587602595986910, 0.000000000000000000 ) ) ;
#98903 = CARTESIAN_POINT ( 'NONE',  ( 16.85830656838225039, -10.38424343889589707, 11.49999999999999645 ) ) ;
#98904 = ADVANCED_FACE ( 'NONE', ( #44311 ), #98569, .F. ) ;
#98905 = CARTESIAN_POINT ( 'NONE',  ( -6.660000000000001030, -10.15233964170348457, 0.003711184059992174607 ) ) ;
#98906 = ORIENTED_EDGE ( 'NONE', *, *, #6081, .F. ) ;
#98907 = LINE ( 'NONE', #14168, #21495 ) ;
#98908 = EDGE_CURVE ( 'NONE', #71598, #39801, #50313, .T. ) ;
#98909 = CARTESIAN_POINT ( 'NONE',  ( -87.62287095715004170, -23.47596703998600631, 11.44779298504227860 ) ) ;
#98910 = CARTESIAN_POINT ( 'NONE',  ( 9.069627533930374241, 19.64968329815391712, 11.49999999999998934 ) ) ;
#98911 = CARTESIAN_POINT ( 'NONE',  ( -27.30764964498456138, -24.78236438415111564, 7.550007144492702160 ) ) ;
#98912 = CARTESIAN_POINT ( 'NONE',  ( -4.539579955115475407, -18.87035741768621122, -1.500000000000002220 ) ) ;
#98913 = EDGE_CURVE ( 'NONE', #54223, #50219, #90770, .T. ) ;
#98914 = CARTESIAN_POINT ( 'NONE',  ( -80.52287095715006160, -23.48786465467241769, 11.44779295918254469 ) ) ;
#98915 = CARTESIAN_POINT ( 'NONE',  ( -129.5228709571501327, -24.33927499327856125, 9.819080762295810061 ) ) ;
#98916 = CARTESIAN_POINT ( 'NONE',  ( 1.944447714513537262, -19.71154682592685958, -1.500000000000002220 ) ) ;
#98917 = ORIENTED_EDGE ( 'NONE', *, *, #68126, .F. ) ;
#98918 = EDGE_CURVE ( 'NONE', #63342, #17304, #19953, .T. ) ;
#98919 = CARTESIAN_POINT ( 'NONE',  ( 19.78452974690265975, -4.759501717958375622, 11.49999999999999645 ) ) ;
#98920 = DIRECTION ( 'NONE',  ( -3.773278334444166432E-23, 1.000000000000000000, 0.000000000000000000 ) ) ;
#98921 = EDGE_CURVE ( 'NONE', #58188, #44485, #93964, .T. ) ;
#98922 = VECTOR ( 'NONE', #6892, 1000.000000000000114 ) ;
#98923 = CARTESIAN_POINT ( 'NONE',  ( 33.50227909998848475, -4.005981270903656188, -11.48786002470558643 ) ) ;
#98924 = EDGE_LOOP ( 'NONE', ( #36477, #23219, #69085, #93736 ) ) ;
#98925 = CARTESIAN_POINT ( 'NONE',  ( -102.5490346760724947, -24.51419770103155926, 9.386484678747178734 ) ) ;
#98926 = DIRECTION ( 'NONE',  ( -3.773278334444166432E-23, 1.000000000000000000, 0.000000000000000000 ) ) ;
#98927 = CARTESIAN_POINT ( 'NONE',  ( 0.000000000000000000, -2.056774720514426669, 4.299999999999999822 ) ) ;
#98928 = B_SPLINE_CURVE_WITH_KNOTS ( 'NONE', 3,
 ( #67510, #68998, #76592, #98431, #99922, #29426, #22305, #28935, #90835, #21308, #52279, #83215, #75592, #55293, #9098, #86223, #9600, #93834, #63917, #62395, #24320, #7596, #16706, #79101, #47674, #48173 ),
 .UNSPECIFIED., .F., .F.,
 ( 4, 2, 2, 2, 2, 2, 2, 2, 2, 2, 2, 2, 4 ),
 ( 2.071553103015771015E-05, 0.001703922715423791898, 0.002545526307620607151, 0.003387129899817422404, 0.004228733492014237656, 0.005070337084211053343, 0.006753544268604682113, 0.007595147860801496932, 0.008436751452998311751, 0.01011995863739193965, 0.01096156222958875708, 0.01180316582178557276, 0.01348637300617921107 ),
 .UNSPECIFIED. ) ;
#98929 = DIRECTION ( 'NONE',  ( -3.773278334453079030E-23, 0.9999999999976377785, 2.173523156925979128E-06 ) ) ;
#98930 = B_SPLINE_CURVE_WITH_KNOTS ( 'NONE', 3,
 ( #16603, #10002, #64831, #2404 ),
 .UNSPECIFIED., .F., .F.,
 ( 4, 4 ),
 ( 0.000000000000000000, 9.999999999998897304E-05 ),
 .UNSPECIFIED. ) ;
#98931 = B_SPLINE_CURVE_WITH_KNOTS ( 'NONE', 3,
 ( #26516, #88415, #58473, #5168 ),
 .UNSPECIFIED., .F., .F.,
 ( 4, 4 ),
 ( 0.000000000000000000, 1.000000000000000000 ),
 .UNSPECIFIED. ) ;
#98932 = CARTESIAN_POINT ( 'NONE',  ( -51.46188133747676119, -25.21125483986890004, 6.515194751273123863 ) ) ;
#98933 = CARTESIAN_POINT ( 'NONE',  ( -6.237196068801617699, -19.06703463882530158, 11.49999999999998934 ) ) ;
#98934 = EDGE_CURVE ( 'NONE', #1756, #12639, #29065, .T. ) ;
#98935 = DIRECTION ( 'NONE',  ( 6.220620959342031946E-15, 0.000000000000000000, -1.000000000000000000 ) ) ;
#98936 = VERTEX_POINT ( 'NONE', #74735 ) ;
#98937 = CARTESIAN_POINT ( 'NONE',  ( -93.58953762381672448, -24.66019654487199730, 8.947790411086121054 ) ) ;
#98938 = CARTESIAN_POINT ( 'NONE',  ( -2.657479817400386413, -22.66247145590962120, 11.49999999999999645 ) ) ;
#98939 = DIRECTION ( 'NONE',  ( 0.000000000000000000, 1.000000000000000000, -0.000000000000000000 ) ) ;
#98940 = CARTESIAN_POINT ( 'NONE',  ( 22.81105451610979173, -1.475225279485572916, -18.46691820600746681 ) ) ;
#98941 = DIRECTION ( 'NONE',  ( -2.327730190238738523E-16, -1.000000000000000000, 8.064610422320909082E-16 ) ) ;
#98942 = CARTESIAN_POINT ( 'NONE',  ( 6.179707021866671646, -5.876774720514425177, 21.45334750074374242 ) ) ;
#98943 = VECTOR ( 'NONE', #31506, 1000.000000000000000 ) ;
#98944 = PLANE ( 'NONE',  #94835 ) ;
#98945 = DIRECTION ( 'NONE',  ( -3.773278334453079030E-23, 0.9999999999976377785, 2.173523156925979128E-06 ) ) ;
#98946 = VERTEX_POINT ( 'NONE', #60038 ) ;
#98947 = CARTESIAN_POINT ( 'NONE',  ( 12.22771034161782566, -16.27230226814707947, 11.49999999999998934 ) ) ;
#98948 = ORIENTED_EDGE ( 'NONE', *, *, #50345, .T. ) ;
#98949 = ADVANCED_FACE ( 'NONE', ( #43312 ), #13831, .F. ) ;
#98950 = CARTESIAN_POINT ( 'NONE',  ( 14.22603995551189371, 18.00578905361294346, -1.500000000000002220 ) ) ;
#98951 = FACE_OUTER_BOUND ( 'NONE', #46468, .T. ) ;
#98952 = ORIENTED_EDGE ( 'NONE', *, *, #67777, .F. ) ;
#98953 = LINE ( 'NONE', #23322, #59096 ) ;
#98955 = ADVANCED_FACE ( 'NONE', ( #51420 ), #5586, .T. ) ;
#98954 = CARTESIAN_POINT ( 'NONE',  ( -72.52287095715007581, -29.50250786944525672, 11.44777988621623699 ) ) ;
#98956 = CARTESIAN_POINT ( 'NONE',  ( -40.62287095715007723, -24.82558206586143257, 1.605769216559447266 ) ) ;
#98958 = VERTEX_POINT ( 'NONE', #87233 ) ;
#98957 = CARTESIAN_POINT ( 'NONE',  ( -9.338289970059909351, 19.12570833482435617, 11.49999999999999645 ) ) ;
#98959 = ORIENTED_EDGE ( 'NONE', *, *, #50843, .T. ) ;
#98960 = CARTESIAN_POINT ( 'NONE',  ( 14.71430157977438924, -16.63553917435140406, -1.500000000000002220 ) ) ;
#98961 = CARTESIAN_POINT ( 'NONE',  ( -13.12974562303265813, -15.89414520977026513, -1.500000000000002220 ) ) ;
#98962 = ORIENTED_EDGE ( 'NONE', *, *, #94154, .T. ) ;
#98963 = VERTEX_POINT ( 'NONE', #99062 ) ;
#98964 = CARTESIAN_POINT ( 'NONE',  ( 6.429811694900724461, -6.376774720514426065, 21.48000018967326596 ) ) ;
#98965 = EDGE_CURVE ( 'NONE', #56669, #89809, #41882, .T. ) ;
#98966 = CARTESIAN_POINT ( 'NONE',  ( -39.98487219060604048, -25.13257598017197836, 2.899846256276811918 ) ) ;
#98967 = EDGE_LOOP ( 'NONE', ( #23332, #22069, #58953, #48875 ) ) ;
#98968 = ORIENTED_EDGE ( 'NONE', *, *, #12082, .T. ) ;
#98969 = CARTESIAN_POINT ( 'NONE',  ( 30.56047832681635867, 2.297196155479663826, 24.67598410064777070 ) ) ;
#98970 = CARTESIAN_POINT ( 'NONE',  ( -41.59371021311409322, -24.15620529776627379, 10.23563542870660825 ) ) ;
#98971 = CARTESIAN_POINT ( 'NONE',  ( 5.313885144808909722, 20.14914662543312929, -1.500000000000002220 ) ) ;
#98973 = EDGE_CURVE ( 'NONE', #63463, #36561, #26245, .T. ) ;
#98972 = CARTESIAN_POINT ( 'NONE',  ( 12.66963027563507005, -17.75133666976559255, 11.49999999999999645 ) ) ;
#98974 = CARTESIAN_POINT ( 'NONE',  ( -50.50582907151566303, -25.03335633882959144, 7.560799548800013703 ) ) ;
#98975 = CARTESIAN_POINT ( 'NONE',  ( -113.6228709571501412, -24.35013146730204525, 9.818937971375106599 ) ) ;
#98976 = CARTESIAN_POINT ( 'NONE',  ( -17.72129891523481149, -13.73837202384828515, 11.49999999999998934 ) ) ;
#98977 = DIRECTION ( 'NONE',  ( 0.000000000000000000, 0.000000000000000000, 1.000000000000000000 ) ) ;
#98978 = EDGE_LOOP ( 'NONE', ( #8255, #52875, #52603, #68947 ) ) ;
#98979 = CARTESIAN_POINT ( 'NONE',  ( -71.70647007306178011, -25.26304665851990094, 6.133561479734631838 ) ) ;
#98980 = FACE_OUTER_BOUND ( 'NONE', #5449, .T. ) ;
#98981 = ORIENTED_EDGE ( 'NONE', *, *, #22624, .F. ) ;
#98982 = ORIENTED_EDGE ( 'NONE', *, *, #48299, .F. ) ;
#98983 = AXIS2_PLACEMENT_3D ( 'NONE', #87048, #25141, #69831 ) ;
#98984 = DIRECTION ( 'NONE',  ( 3.773278334444167608E-23, -1.000000000000000000, 0.000000000000000000 ) ) ;
#98985 = CC_DESIGN_PERSON_AND_ORGANIZATION_ASSIGNMENT ( #700, #8820, ( #20704 ) ) ;
#98986 = ORIENTED_EDGE ( 'NONE', *, *, #84970, .F. ) ;
#98987 = CARTESIAN_POINT ( 'NONE',  ( 10.72677997844354536, -18.41129465587203740, -1.500000000000002220 ) ) ;
#98988 = ORIENTED_EDGE ( 'NONE', *, *, #26358, .F. ) ;
#98989 = CARTESIAN_POINT ( 'NONE',  ( 0.000000000000000000, -4.056774720514426669, 0.000000000000000000 ) ) ;
#98990 = CARTESIAN_POINT ( 'NONE',  ( -20.73700405699343463, 3.470425206167693233, -1.500000000000002220 ) ) ;
#98991 = CARTESIAN_POINT ( 'NONE',  ( -45.55620429048339304, -23.48783264082477373, -1.443836473390068820 ) ) ;
#98992 = CARTESIAN_POINT ( 'NONE',  ( 15.32675665358028283, -3.579156900695799060, -27.14457288197743878 ) ) ;
#98993 = CARTESIAN_POINT ( 'NONE',  ( -79.11611000704996854, -25.20074463982482982, 3.409327697717700278 ) ) ;
#98994 = CARTESIAN_POINT ( 'NONE',  ( -9.563806973793814947, 19.74097577964120376, -1.500000000000002220 ) ) ;
#98995 = CARTESIAN_POINT ( 'NONE',  ( -52.62287095715005592, -29.50250243563736774, 8.947779886222146928 ) ) ;
#98996 = ORIENTED_EDGE ( 'NONE', *, *, #72821, .T. ) ;
#98997 = CARTESIAN_POINT ( 'NONE',  ( -80.80267296708018421, -25.30788629407443935, 4.569020114890182782 ) ) ;
#98998 = CARTESIAN_POINT ( 'NONE',  ( -84.54195721757037063, -24.66019654487200441, 8.947790411086115725 ) ) ;
#98999 = VECTOR ( 'NONE', #12921, 1000.000000000000114 ) ;
#99000 = CARTESIAN_POINT ( 'NONE',  ( -130.5728709571501156, -25.30559561715419647, 6.147794833475638931 ) ) ;
#99001 = CARTESIAN_POINT ( 'NONE',  ( -0.1490749075164066184, -21.12010817310450861, 11.44779298504228038 ) ) ;
#99002 = CARTESIAN_POINT ( 'NONE',  ( 15.78869406909177897, -14.30566568001193950, -1.500000000000002220 ) ) ;
#99003 = CARTESIAN_POINT ( 'NONE',  ( -98.58873755195853050, -24.35071581493543746, 9.817618358456027039 ) ) ;
#99004 = CARTESIAN_POINT ( 'NONE',  ( -27.61766922344000363, -24.75185970960561122, 2.278554975841372787 ) ) ;
#99005 = CARTESIAN_POINT ( 'NONE',  ( -61.22287095715005023, -23.47596703998600276, 11.44779298504227860 ) ) ;
#99006 = CARTESIAN_POINT ( 'NONE',  ( -112.6228709571500559, -29.50248528299804818, 1.056150453629043584 ) ) ;
#99007 = CARTESIAN_POINT ( 'NONE',  ( -5.125883829288005344, 21.89707322345674712, -1.500000000000002220 ) ) ;
#99008 = CARTESIAN_POINT ( 'NONE',  ( -111.9725711586931283, -25.11552134530501590, 2.805129186380271644 ) ) ;
#99009 = VERTEX_POINT ( 'NONE', #1514 ) ;
#99010 = CARTESIAN_POINT ( 'NONE',  ( -100.4498239493576648, -25.04307398257883932, 7.563174194274490780 ) ) ;
#99011 = CARTESIAN_POINT ( 'NONE',  ( -12.94911239430987315, -14.73082512860577609, 11.49999999999999645 ) ) ;
#99012 = CARTESIAN_POINT ( 'NONE',  ( -95.52287095715011844, -23.48783264082477373, -1.443836473390086139 ) ) ;
#99013 = EDGE_CURVE ( 'NONE', #24726, #17192, #31952, .T. ) ;
#99015 = B_SPLINE_CURVE_WITH_KNOTS ( 'NONE', 3,
 ( #76339, #92566, #60652, #14445, #99666, #15444, #99181, #91079 ),
 .UNSPECIFIED., .F., .F.,
 ( 4, 2, 2, 4 ),
 ( -0.001224873891641429548, -0.0002244903592271130493, 0.0007758931731872034492, 0.002776660238015839915 ),
 .UNSPECIFIED. ) ;
#99014 = DIRECTION ( 'NONE',  ( -3.773278334453080206E-23, 0.9999999999976377785, 2.173523156925979975E-06 ) ) ;
#99016 = VERTEX_POINT ( 'NONE', #48188 ) ;
#99017 = CARTESIAN_POINT ( 'NONE',  ( -88.62596114253774715, -24.51419770103157703, 9.386484678747176957 ) ) ;
#99018 = CARTESIAN_POINT ( 'NONE',  ( -36.52287095715006870, -23.47596703998600631, 11.44779298504229281 ) ) ;
#99019 = CARTESIAN_POINT ( 'NONE',  ( -100.6373084487711225, -25.31439533618487303, 5.200261023079458589 ) ) ;
#99020 = CARTESIAN_POINT ( 'NONE',  ( -42.55620429048339304, -23.48783264082477729, -1.443836473390073705 ) ) ;
#99021 = CARTESIAN_POINT ( 'NONE',  ( -9.297559507673007317, 17.40068379117045083, 11.49999999999998934 ) ) ;
#99022 = ORIENTED_EDGE ( 'NONE', *, *, #93348, .F. ) ;
#99023 = EDGE_CURVE ( 'NONE', #13572, #29853, #61030, .T. ) ;
#99024 = LINE ( 'NONE', #4704, #5148 ) ;
#99025 = DIRECTION ( 'NONE',  ( 0.000000000000000000, -2.173523156925979552E-06, 0.9999999999976378895 ) ) ;
#99026 = ADVANCED_FACE ( 'NONE', ( #21933 ), #14328, .F. ) ;
#99027 = PERSON_AND_ORGANIZATION ( #70597, #27821 ) ;
#99028 = ORIENTED_EDGE ( 'NONE', *, *, #49638, .F. ) ;
#99029 = DIRECTION ( 'NONE',  ( 0.000000000000000000, -0.000000000000000000, -1.000000000000000000 ) ) ;
#99030 = DIRECTION ( 'NONE',  ( -0.9161084732596777025, -4.164321980682960499E-15, 0.4009304992412306978 ) ) ;
#99031 = CARTESIAN_POINT ( 'NONE',  ( -55.58902656714176516, -24.52300882791528736, 0.6510814631126286001 ) ) ;
#99032 = CARTESIAN_POINT ( 'NONE',  ( -118.5555942329009014, -23.96119346886881019, -0.6495511937832023630 ) ) ;
#99033 = CARTESIAN_POINT ( 'NONE',  ( -22.05275734969026047, 5.965225279485572685, 30.51402280011862089 ) ) ;
#99034 = CARTESIAN_POINT ( 'NONE',  ( -70.15650799851037789, -25.24515045258689483, 5.327551117306890127 ) ) ;
#99035 = DIRECTION ( 'NONE',  ( 0.000000000000000000, 0.000000000000000000, -1.000000000000000000 ) ) ;
#99036 = CARTESIAN_POINT ( 'NONE',  ( -19.95764006394758638, 0.7380318605572177004, -1.500000000000002220 ) ) ;
#99037 = EDGE_CURVE ( 'NONE', #41750, #37181, #3299, .T. ) ;
#99038 = B_SPLINE_CURVE_WITH_KNOTS ( 'NONE', 3,
 ( #48503, #63229, #55110, #79428 ),
 .UNSPECIFIED., .F., .F.,
 ( 4, 4 ),
 ( 0.6592456326193364413, 0.6602463796601018009 ),
 .UNSPECIFIED. ) ;
#99039 = CARTESIAN_POINT ( 'NONE',  ( 29.73860345376319714, 4.772774720514425972, -4.021250162519585558 ) ) ;
#99040 = CARTESIAN_POINT ( 'NONE',  ( -45.63256516684009512, -24.73531770709095312, 8.716586749053515604 ) ) ;
#99041 = ORIENTED_EDGE ( 'NONE', *, *, #41023, .F. ) ;
#99042 = DIRECTION ( 'NONE',  ( 0.000000000000000000, 0.000000000000000000, -1.000000000000000000 ) ) ;
#99043 = DIRECTION ( 'NONE',  ( -0.000000000000000000, -1.000000000000000000, -0.000000000000000000 ) ) ;
#99044 = CARTESIAN_POINT ( 'NONE',  ( -80.59162667163354854, -24.40133493613050319, 9.663955038902802386 ) ) ;
#99045 = CARTESIAN_POINT ( 'NONE',  ( -81.58953762381672448, -23.48783264082478794, -1.443836473390065711 ) ) ;
#99046 = CARTESIAN_POINT ( 'NONE',  ( -39.58114864661853005, -24.51314013834315730, 0.6176544820404118452 ) ) ;
#99047 = B_SPLINE_CURVE_WITH_KNOTS ( 'NONE', 3,
 ( #13700, #67512, #20812, #67025 ),
 .UNSPECIFIED., .F., .F.,
 ( 4, 4 ),
 ( 0.000000000000000000, 1.000000000000000000 ),
 .UNSPECIFIED. ) ;
#99048 = VECTOR ( 'NONE', #35298, 1000.000000000000000 ) ;
#99049 = CARTESIAN_POINT ( 'NONE',  ( -97.58953762381672448, -24.65952944569304961, 1.056160979905701902 ) ) ;
#99050 = CARTESIAN_POINT ( 'NONE',  ( -1.568769572606061535, -6.376774720514415407, 19.76359802465961835 ) ) ;
#99051 = CARTESIAN_POINT ( 'NONE',  ( 14.76093561896378148, 3.316774720514426456, -26.55548769130088971 ) ) ;
#99052 = CARTESIAN_POINT ( 'NONE',  ( -111.5228709571500616, -29.50250786944525672, 11.44777988621622988 ) ) ;
#99053 = VERTEX_POINT ( 'NONE', #91961 ) ;
#99054 = CARTESIAN_POINT ( 'NONE',  ( -17.45352675615719917, 10.31968153043333380, -1.500000000000002220 ) ) ;
#99055 = LINE ( 'NONE', #21928, #92220 ) ;
#99056 = CARTESIAN_POINT ( 'NONE',  ( -7.999999999999996447, -6.376774720514426953, 17.50000000000000000 ) ) ;
#99057 = FACE_OUTER_BOUND ( 'NONE', #56203, .T. ) ;
#99058 = VERTEX_POINT ( 'NONE', #22433 ) ;
#99060 = EDGE_CURVE ( 'NONE', #100399, #7123, #78140, .T. ) ;
#99059 = CARTESIAN_POINT ( 'NONE',  ( 25.83488407601163672, -4.132774720514426292, -11.31196583263650091 ) ) ;
#99061 = B_SPLINE_CURVE_WITH_KNOTS ( 'NONE', 3,
 ( #76570, #14681, #37028, #59373, #37528, #68973 ),
 .UNSPECIFIED., .F., .F.,
 ( 4, 2, 4 ),
 ( 1.570887131794952276E-05, 0.001396322306279766060, 0.002776935741241582344 ),
 .UNSPECIFIED. ) ;
#99062 = CARTESIAN_POINT ( 'NONE',  ( -9.940598223437573822, -5.876774720514426953, 18.21871304725684837 ) ) ;
#99063 = VECTOR ( 'NONE', #74697, 1000.000000000000114 ) ;
#99064 = CARTESIAN_POINT ( 'NONE',  ( -19.68739882612603864, 4.164723872966736629, -1.500000000000002220 ) ) ;
#99065 = CARTESIAN_POINT ( 'NONE',  ( 13.75562813033083742, -15.94169299924578453, 11.49999999999999645 ) ) ;
#99066 = APPROVAL_PERSON_ORGANIZATION ( #11439, #42673, #63756 ) ;
#99067 = DIRECTION ( 'NONE',  ( 0.000000000000000000, 0.000000000000000000, -1.000000000000000000 ) ) ;
#99068 = CARTESIAN_POINT ( 'NONE',  ( -22.03165466229905789, 1.424673820674137614, -1.500000000000002220 ) ) ;
#99069 = EDGE_CURVE ( 'NONE', #93197, #74266, #60027, .T. ) ;
#99070 = CARTESIAN_POINT ( 'NONE',  ( 20.13950599927006735, 4.067174238878714654, -1.500000000000002220 ) ) ;
#99071 = PLANE ( 'NONE',  #25234 ) ;
#99072 = EDGE_CURVE ( 'NONE', #16621, #39794, #35460, .T. ) ;
#99073 = LINE ( 'NONE', #51928, #100217 ) ;
#99074 = VERTEX_POINT ( 'NONE', #41578 ) ;
#99075 = DIRECTION ( 'NONE',  ( -3.773278334444166432E-23, 1.000000000000000000, 0.000000000000000000 ) ) ;
#99076 = EDGE_LOOP ( 'NONE', ( #72197, #91734, #62062, #42977 ) ) ;
#99077 = CARTESIAN_POINT ( 'NONE',  ( -99.40985337475474637, -25.19006306930774386, 3.256098372597241219 ) ) ;
#99078 = LINE ( 'NONE', #38684, #68029 ) ;
#99079 = ORIENTED_EDGE ( 'NONE', *, *, #22491, .F. ) ;
#99080 = ORIENTED_EDGE ( 'NONE', *, *, #46440, .T. ) ;
#99081 = LINE ( 'NONE', #77235, #90755 ) ;
#99082 = CARTESIAN_POINT ( 'NONE',  ( -120.6228709571500417, -29.50250786944525672, 11.44777988621622811 ) ) ;
#99083 = DIRECTION ( 'NONE',  ( 1.000000000000000000, 0.000000000000000000, -0.000000000000000000 ) ) ;
#99084 = CARTESIAN_POINT ( 'NONE',  ( 19.39950376024442846, -7.079068461131618584, -1.500000000000002220 ) ) ;
#99085 = CARTESIAN_POINT ( 'NONE',  ( -7.466173891270859286, -20.28576548065916541, 11.49999999999999645 ) ) ;
#99086 = ORIENTED_EDGE ( 'NONE', *, *, #32601, .F. ) ;
#99087 = LINE ( 'NONE', #58559, #79037 ) ;
#99088 = CARTESIAN_POINT ( 'NONE',  ( -23.62875734969026453, -6.143225279485574397, 23.50402280011862288 ) ) ;
#99089 = CARTESIAN_POINT ( 'NONE',  ( -0.4079105510268487000, 22.33655531192813370, 11.49999999999998934 ) ) ;
#99090 = B_SPLINE_CURVE_WITH_KNOTS ( 'NONE', 3,
 ( #13549, #36900, #30275, #68354 ),
 .UNSPECIFIED., .F., .F.,
 ( 4, 4 ),
 ( 0.000000000000000000, 9.999999999998897304E-05 ),
 .UNSPECIFIED. ) ;
#99091 = CARTESIAN_POINT ( 'NONE',  ( -93.52287095715006160, -24.50216790748204687, 0.6166512839542578339 ) ) ;
#99092 = CARTESIAN_POINT ( 'NONE',  ( -104.5562042904833930, -24.64898659630529210, 1.056161002820829919 ) ) ;
#99093 = VERTEX_POINT ( 'NONE', #25837 ) ;
#99094 = CARTESIAN_POINT ( 'NONE',  ( -43.52287095715007581, -23.47593901973090169, -1.443836447538997092 ) ) ;
#99095 = CARTESIAN_POINT ( 'NONE',  ( -35.47207274640775410, -24.83644354573578639, 8.397322867130093016 ) ) ;
#99096 = CARTESIAN_POINT ( 'NONE',  ( -15.12424899162716230, 14.39509690008720177, -1.500000000000002220 ) ) ;
#99097 = VERTEX_POINT ( 'NONE', #73028 ) ;
#99098 = EDGE_CURVE ( 'NONE', #40304, #67935, #11606, .T. ) ;
#99100 = ORIENTED_EDGE ( 'NONE', *, *, #86035, .F. ) ;
#99099 = CARTESIAN_POINT ( 'NONE',  ( -86.63934676394221412, -23.73766607897671221, -1.055555164236432697 ) ) ;
#99101 = VERTEX_POINT ( 'NONE', #56813 ) ;
#99102 = CIRCLE ( 'NONE', #27852, 84.48086791635432746 ) ;
#99103 = CARTESIAN_POINT ( 'NONE',  ( -109.5877440957333704, -24.51419770103157347, 9.386484678747171628 ) ) ;
#99104 = CARTESIAN_POINT ( 'NONE',  ( 17.61891135320703938, 11.69080507458975227, -1.500000000000002220 ) ) ;
#99105 = ORIENTED_EDGE ( 'NONE', *, *, #36422, .T. ) ;
#99106 = CARTESIAN_POINT ( 'NONE',  ( -117.5936837924626701, -23.48783264082477018, -1.443836473390081254 ) ) ;
#99107 = LINE ( 'NONE', #79154, #90376 ) ;
#99108 = CARTESIAN_POINT ( 'NONE',  ( 21.36706796925463792, 4.321743776461201669, 11.49999999999998934 ) ) ;
#99109 = CARTESIAN_POINT ( 'NONE',  ( -114.2228709571500644, -23.47596703998600276, 11.44779298504227683 ) ) ;
#99110 = B_SPLINE_CURVE_WITH_KNOTS ( 'NONE', 3,
 ( #76723, #38171, #59042, #92958, #10117, #32965 ),
 .UNSPECIFIED., .F., .F.,
 ( 4, 2, 4 ),
 ( 3.122786320239759279E-05, 0.002624795872137489043, 0.005218363881072580514 ),
 .UNSPECIFIED. ) ;
#99111 = CARTESIAN_POINT ( 'NONE',  ( -41.52287095715006870, -24.50216790748205042, 0.6166512839542425128 ) ) ;
#99112 = CARTESIAN_POINT ( 'NONE',  ( 7.370931459274800090, -5.876774720514417183, 20.26286690110499578 ) ) ;
#99113 = CARTESIAN_POINT ( 'NONE',  ( -8.443908442993951269, 20.02826104456839218, -1.500000000000002220 ) ) ;
#99114 = CARTESIAN_POINT ( 'NONE',  ( -71.27229073968156570, -25.24674082005258313, 4.988759856649874536 ) ) ;
#99116 = VERTEX_POINT ( 'NONE', #18230 ) ;
#99115 = CARTESIAN_POINT ( 'NONE',  ( -20.85237562250380350, -7.973873963886685345, 11.49999999999999645 ) ) ;
#99117 = CARTESIAN_POINT ( 'NONE',  ( -57.52287095715003318, -23.73934037231757088, 11.05740245334328797 ) ) ;
#99118 = DIRECTION ( 'NONE',  ( -1.000000000000000000, 0.000000000000000000, 0.000000000000000000 ) ) ;
#99119 = CARTESIAN_POINT ( 'NONE',  ( 31.81388842165050335, -4.825737335974109143, -4.598239840489335428 ) ) ;
#99120 = VERTEX_POINT ( 'NONE', #97351 ) ;
#99121 = EDGE_CURVE ( 'NONE', #96155, #100313, #29817, .T. ) ;
#99122 = ORIENTED_EDGE ( 'NONE', *, *, #66526, .T. ) ;
#99123 = ORIENTED_EDGE ( 'NONE', *, *, #74997, .F. ) ;
#99124 = EDGE_CURVE ( 'NONE', #69709, #19646, #80691, .T. ) ;
#99125 = CARTESIAN_POINT ( 'NONE',  ( -85.62287095715005592, -23.48786465467241413, 11.44779295918254114 ) ) ;
#99126 = CARTESIAN_POINT ( 'NONE',  ( -10.79823215447539653, -18.26288818932900071, -1.500000000000002220 ) ) ;
#99127 = CIRCLE ( 'NONE', #16558, 129.7684398600581517 ) ;
#99128 = DIRECTION ( 'NONE',  ( 9.453533929028921186E-17, -1.000000000000000000, -8.881784197001252323E-16 ) ) ;
#99129 = CARTESIAN_POINT ( 'NONE',  ( -79.46053308078880661, -25.03138219016592103, 7.192627279560748654 ) ) ;
#99130 = CARTESIAN_POINT ( 'NONE',  ( -59.52287095715004739, -24.66019654487199375, 8.947790411086128159 ) ) ;
#99131 = CARTESIAN_POINT ( 'NONE',  ( 5.331146515430939203, -5.876774720514419847, 20.91308853528358469 ) ) ;
#99132 = CARTESIAN_POINT ( 'NONE',  ( -2.960655606634402748, -19.13016773636607581, 11.49999999999998934 ) ) ;
#99133 = CARTESIAN_POINT ( 'NONE',  ( -31.52287095715006870, -24.35013146730202394, 9.818937971375110152 ) ) ;
#99134 = ORIENTED_EDGE ( 'NONE', *, *, #100163, .T. ) ;
#99135 = CARTESIAN_POINT ( 'NONE',  ( 18.36381783059253081, 6.383776564742674964, 11.49999999999999645 ) ) ;
#99136 = DIRECTION ( 'NONE',  ( -4.522247983293619802E-39, -2.173523156893721996E-06, 0.9999999999976377785 ) ) ;
#99137 = EDGE_CURVE ( 'NONE', #18000, #50597, #29203, .T. ) ;
#99138 = EDGE_LOOP ( 'NONE', ( #1300, #42225, #68814, #97558 ) ) ;
#99139 = DIRECTION ( 'NONE',  ( -1.000000000000000000, 0.000000000000000000, 0.000000000000000000 ) ) ;
#99140 = CARTESIAN_POINT ( 'NONE',  ( -20.77875734969026311, 6.143225279485574397, 29.49402280011862487 ) ) ;
#99141 = CARTESIAN_POINT ( 'NONE',  ( -64.92287095715006728, -23.47596703998600631, 11.44779298504227860 ) ) ;
#99142 = CARTESIAN_POINT ( 'NONE',  ( 26.73860345374794889, -5.236829402159759894, -5.783717876163293248 ) ) ;
#99143 = AXIS2_PLACEMENT_3D ( 'NONE', #48033, #95199, #94691 ) ;
#99144 = CARTESIAN_POINT ( 'NONE',  ( 10.60981200654714307, 16.52409317135366607, 11.49999999999998934 ) ) ;
#99145 = CARTESIAN_POINT ( 'NONE',  ( 3.421177667410919110, -0.3587747205144265483, 28.69411518427638441 ) ) ;
#99147 = VERTEX_POINT ( 'NONE', #41072 ) ;
#99146 = LOCAL_TIME ( 0, 54, 15.00000000000000000, #16925 ) ;
#99148 = CARTESIAN_POINT ( 'NONE',  ( -4.138935798035190849, -21.16376344109877294, 11.49999999999998934 ) ) ;
#99149 = CARTESIAN_POINT ( 'NONE',  ( -33.48940092244485101, -24.35071581493542325, 9.817618358456039473 ) ) ;
#99150 = CARTESIAN_POINT ( 'NONE',  ( -96.62287095715005592, -23.48783264082478794, -1.443836473390061936 ) ) ;
#99151 = CARTESIAN_POINT ( 'NONE',  ( -81.62287095715005592, -24.64965695001468404, 8.947790433994182280 ) ) ;
#99152 = CARTESIAN_POINT ( 'NONE',  ( -99.67151487672813914, -25.27473290596300615, 3.611381105655242063 ) ) ;
#99153 = CARTESIAN_POINT ( 'NONE',  ( 15.83906049732654608, 16.74391201645830662, -1.500000000000002220 ) ) ;
#99154 = EDGE_CURVE ( 'NONE', #16993, #90405, #42083, .T. ) ;
#99155 = EDGE_CURVE ( 'NONE', #45368, #26606, #34954, .T. ) ;
#99156 = CALENDAR_DATE ( 2026, 9, 10 ) ;
#99157 = CARTESIAN_POINT ( 'NONE',  ( -93.63081067970922788, -24.15543982623907482, -0.2315651400026620677 ) ) ;
#99158 = CARTESIAN_POINT ( 'NONE',  ( -50.70307649397453531, -25.30285855287542773, 4.744951912546983230 ) ) ;
#99159 = CARTESIAN_POINT ( 'NONE',  ( 19.84801528777503776, 3.447069022702595742, 11.49999999999999645 ) ) ;
#99160 = CARTESIAN_POINT ( 'NONE',  ( -45.62287095715004881, -24.99156045073392463, 7.747789690856161648 ) ) ;
#99161 = CARTESIAN_POINT ( 'NONE',  ( -91.52287095715003318, -23.48783264082477018, -1.443836473390089248 ) ) ;
#99162 = LINE ( 'NONE', #5827, #32791 ) ;
#99163 = DIRECTION ( 'NONE',  ( 0.000000000000000000, 0.9999999999976377785, 2.173523156925979975E-06 ) ) ;
#99164 = DIRECTION ( 'NONE',  ( 0.000000000000000000, -1.000000000000000000, 0.000000000000000000 ) ) ;
#99165 = CARTESIAN_POINT ( 'NONE',  ( 17.57725459251073019, -9.329341740261039462, -1.500000000000002220 ) ) ;
#99166 = EDGE_CURVE ( 'NONE', #65146, #78876, #2513, .T. ) ;
#99167 = CARTESIAN_POINT ( 'NONE',  ( -97.58953762381672448, -23.48786465467241058, 11.44779295918254114 ) ) ;
#99168 = CARTESIAN_POINT ( 'NONE',  ( 9.697495225759652726, 17.24774500829319734, -1.500000000000002220 ) ) ;
#99169 = FACE_OUTER_BOUND ( 'NONE', #37538, .T. ) ;
#99170 = ADVANCED_FACE ( 'NONE', ( #80125 ), #3514, .T. ) ;
#99171 = CARTESIAN_POINT ( 'NONE',  ( -1.036876607668611117, -6.376774720514417183, 20.14881673916291405 ) ) ;
#99172 = FACE_OUTER_BOUND ( 'NONE', #53640, .T. ) ;
#99173 = CARTESIAN_POINT ( 'NONE',  ( 11.79242832063081892, -16.95861370568002613, 11.49999999999999645 ) ) ;
#99174 = CARTESIAN_POINT ( 'NONE',  ( -56.58953762381672448, -23.47593901973091235, -1.443836447539007972 ) ) ;
#99175 = DIRECTION ( 'NONE',  ( -3.773278334453079030E-23, 0.9999999999976377785, 2.173523156925979128E-06 ) ) ;
#99176 = DIRECTION ( 'NONE',  ( 0.000000000000000000, -2.173523156925980399E-06, 0.9999999999976378895 ) ) ;
#99177 = CARTESIAN_POINT ( 'NONE',  ( 12.23086119556625206, 19.17791753167082192, 11.49999999999999645 ) ) ;
#99178 = AXIS2_PLACEMENT_3D ( 'NONE', #78025, #48111, #94265 ) ;
#99179 = ORIENTED_EDGE ( 'NONE', *, *, #72302, .T. ) ;
#99180 = B_SPLINE_SURFACE_WITH_KNOTS ( 'NONE', 3, 3, ( 
 ( #95560, #42787, #73719, #19430 ),
 ( #33153, #18434, #4214, #26042 ),
 ( #57016, #96553, #34667, #11326 ),
 ( #64138, #35168, #86940, #88454 ),
 ( #26555, #10321, #95058, #49905 ),
 ( #17937, #80839, #65139, #48391 ),
 ( #42303, #71731, #56515, #50395 ) ),
 .UNSPECIFIED., .F., .F., .F.,
 ( 4, 3, 4 ),
 ( 4, 4 ),
 ( 0.3495694201722119865, 0.5199403837404874551, 0.6903113473087629792 ),
 ( 0.4867129260185943385, 0.5164839350294436748 ),
 .UNSPECIFIED. ) ;
#99181 = CARTESIAN_POINT ( 'NONE',  ( -60.62287095715002039, -23.85196035786901803, -0.8779234886474974742 ) ) ;
#99182 = CARTESIAN_POINT ( 'NONE',  ( -2.243088942307695177, -6.376774720514408301, 19.14743589743590491 ) ) ;
#99183 = CARTESIAN_POINT ( 'NONE',  ( -20.08517628505838815, -1.856936949192496300, 11.49999999999998934 ) ) ;
#99184 = CARTESIAN_POINT ( 'NONE',  ( 8.971512145086503409, -1.000000000000000000, -3.746884140868835367 ) ) ;
#99185 = CARTESIAN_POINT ( 'NONE',  ( -41.45979626101074444, -25.28633313991813480, 4.315766560440735589 ) ) ;
#99186 = ORIENTED_EDGE ( 'NONE', *, *, #8611, .T. ) ;
#99187 = ORIENTED_EDGE ( 'NONE', *, *, #3732, .F. ) ;
#99188 = EDGE_CURVE ( 'NONE', #32699, #77487, #10617, .T. ) ;
#99189 = DIRECTION ( 'NONE',  ( 0.000000000000000000, 0.000000000000000000, 1.000000000000000000 ) ) ;
#99190 = CARTESIAN_POINT ( 'NONE',  ( 22.67525425759127344, 3.225002893152739247, 11.49999999999998934 ) ) ;
#99191 = CARTESIAN_POINT ( 'NONE',  ( -49.62287095715005592, -29.50247984919015209, -1.443849546365058689 ) ) ;
#99192 = CARTESIAN_POINT ( 'NONE',  ( 16.53012286974688294, -13.99140274789385252, -1.500000000000002220 ) ) ;
#99193 = DIRECTION ( 'NONE',  ( -3.773278334444167608E-23, 1.000000000000000000, 0.000000000000000000 ) ) ;
#99194 = CARTESIAN_POINT ( 'NONE',  ( -114.6228709571500559, -24.64898659630528854, 1.056161002820831474 ) ) ;
#99195 = VECTOR ( 'NONE', #40772, 1000.000000000000114 ) ;
#99196 = CARTESIAN_POINT ( 'NONE',  ( -5.518977837361389582, -20.17201009624758257, 11.49999999999999645 ) ) ;
#99197 = VERTEX_POINT ( 'NONE', #96353 ) ;
#99198 = CARTESIAN_POINT ( 'NONE',  ( -27.83139521413862028, -24.79471210469401043, 2.282574248019634933 ) ) ;
#99199 = AXIS2_PLACEMENT_3D ( 'NONE', #53032, #98682, #61645 ) ;
#99200 = CARTESIAN_POINT ( 'NONE',  ( -1.351711525931510449, 21.94731587555429186, 11.49999999999998934 ) ) ;
#99201 = CARTESIAN_POINT ( 'NONE',  ( -105.5477487753952488, -24.83644354573579349, 8.397322867130096569 ) ) ;
#99202 = CARTESIAN_POINT ( 'NONE',  ( -41.46538131673724337, -25.29087121120879544, 3.231378520143959765 ) ) ;
#99204 = ORIENTED_EDGE ( 'NONE', *, *, #57848, .T. ) ;
#99203 = ADVANCED_FACE ( 'NONE', ( #27344 ), #57805, .F. ) ;
#99205 = DIRECTION ( 'NONE',  ( 0.7512896232465894331, 0.000000000000000000, 0.6599726524652348436 ) ) ;
#99206 = DIRECTION ( 'NONE',  ( 0.6451914333552788428, 0.000000000000000000, 0.7640209514960704107 ) ) ;
#99207 = EDGE_LOOP ( 'NONE', ( #12850, #73252, #73536, #42724 ) ) ;
#99208 = CARTESIAN_POINT ( 'NONE',  ( -72.51140272759705852, -23.96169478059712787, 10.65365249895718414 ) ) ;
#99209 = ORIENTED_EDGE ( 'NONE', *, *, #70987, .T. ) ;
#99210 = ORIENTED_EDGE ( 'NONE', *, *, #27558, .F. ) ;
#99211 = CARTESIAN_POINT ( 'NONE',  ( -59.55620429048340725, -23.47593901973091235, -1.443836447539007972 ) ) ;
#99212 = CARTESIAN_POINT ( 'NONE',  ( -117.5895376238167103, -24.64965694238408034, 8.947790433994645909 ) ) ;
#99213 = CARTESIAN_POINT ( 'NONE',  ( -36.55286501431240254, -23.96119346886880308, -0.6495511937832127991 ) ) ;
#99214 = CARTESIAN_POINT ( 'NONE',  ( -10.82153711268468932, 17.32902648900640230, -1.500000000000002220 ) ) ;
#99215 = EDGE_LOOP ( 'NONE', ( #57222, #15726, #11470, #37220 ) ) ;
#99216 = CARTESIAN_POINT ( 'NONE',  ( -2.243088942307695621, -5.876774720514409189, 19.14743589743590846 ) ) ;
#99217 = CARTESIAN_POINT ( 'NONE',  ( -30.59367615247571237, -24.87212640336024805, 1.420893871182736579 ) ) ;
#99219 = CARTESIAN_POINT ( 'NONE',  ( -2.449489742783178770, -1.473225279485573358, 2.499999999999999556 ) ) ;
#99218 = AXIS2_PLACEMENT_3D ( 'NONE', #41894, #72839, #39874 ) ;
#99220 = CARTESIAN_POINT ( 'NONE',  ( -28.62287095715004881, -24.49675894734168580, 8.947790415257339092 ) ) ;
#99221 = ORIENTED_EDGE ( 'NONE', *, *, #30452, .F. ) ;
#99222 = FACE_OUTER_BOUND ( 'NONE', #83664, .T. ) ;
#99223 = CARTESIAN_POINT ( 'NONE',  ( -29.81002072791678614, -24.63645409607815395, 5.237832512065683233 ) ) ;
#99224 = CC_DESIGN_APPROVAL ( #75393, ( #14993 ) ) ;
#99225 = CARTESIAN_POINT ( 'NONE',  ( 7.312689604342500260, -19.48077458720139532, -1.500000000000002220 ) ) ;
#99226 = ORIENTED_EDGE ( 'NONE', *, *, #87757, .F. ) ;
#99228 = ORIENTED_EDGE ( 'NONE', *, *, #99013, .T. ) ;
#99227 = DIRECTION ( 'NONE',  ( 1.000000000000000000, 0.000000000000000000, 0.000000000000000000 ) ) ;
#99229 = EDGE_CURVE ( 'NONE', #40606, #31854, #73520, .T. ) ;
#99230 = VECTOR ( 'NONE', #22263, 1000.000000000000000 ) ;
#99231 = CARTESIAN_POINT ( 'NONE',  ( -28.62287095715004881, -23.31957264754183967, 11.44779298504227860 ) ) ;
#99232 = EDGE_LOOP ( 'NONE', ( #2011, #43234, #20137, #59981 ) ) ;
#99233 = VERTEX_POINT ( 'NONE', #58303 ) ;
#99234 = DIRECTION ( 'NONE',  ( -1.000000000000000000, -0.000000000000000000, -0.000000000000000000 ) ) ;
#99235 = CARTESIAN_POINT ( 'NONE',  ( -55.62287095715004881, -24.62285846362214770, 9.038163152653524435 ) ) ;
#99236 = DIRECTION ( 'NONE',  ( 0.000000000000000000, -1.000000000000000000, 0.000000000000000000 ) ) ;
#99237 = AXIS2_PLACEMENT_3D ( 'NONE', #25251, #57722, #65353 ) ;
#99238 = FACE_OUTER_BOUND ( 'NONE', #79869, .T. ) ;
#99239 = CARTESIAN_POINT ( 'NONE',  ( -91.58953762381672448, -23.47593901973091235, -1.443836447539002865 ) ) ;
#99240 = CARTESIAN_POINT ( 'NONE',  ( 0.7051282051282083962, -6.376774720514427841, 21.75000000000000000 ) ) ;
#99242 = ORIENTED_EDGE ( 'NONE', *, *, #63430, .T. ) ;
#99241 = CARTESIAN_POINT ( 'NONE',  ( 7.527104757430762128, -20.84474501729809859, 11.49999999999999645 ) ) ;
#99243 = B_SPLINE_CURVE_WITH_KNOTS ( 'NONE', 3,
 ( #2328, #33257, #94659, #47998 ),
 .UNSPECIFIED., .F., .F.,
 ( 4, 4 ),
 ( 0.000000000000000000, 0.0001000000000000028644 ),
 .UNSPECIFIED. ) ;
#99244 = DIRECTION ( 'NONE',  ( -3.773278334453080206E-23, 0.9999999999976377785, 2.173523156925979975E-06 ) ) ;
#99245 = CARTESIAN_POINT ( 'NONE',  ( 5.572475817582897228, 21.94689365879375131, 11.49999999999998934 ) ) ;
#99246 = EDGE_CURVE ( 'NONE', #64205, #56116, #89241, .T. ) ;
#99247 = ADVANCED_FACE ( 'NONE', ( #21211 ), #13685, .T. ) ;
#99248 = EDGE_CURVE ( 'NONE', #14217, #7016, #83109, .T. ) ;
#99250 = VERTEX_POINT ( 'NONE', #59291 ) ;
#99249 = CARTESIAN_POINT ( 'NONE',  ( -92.52287095715006160, -23.48783264083452593, -1.443836473374927820 ) ) ;
#99251 = ORIENTED_EDGE ( 'NONE', *, *, #87582, .T. ) ;
#99252 = EDGE_CURVE ( 'NONE', #88761, #17738, #29831, .T. ) ;
#99253 = CARTESIAN_POINT ( 'NONE',  ( -80.77089339228673737, -25.31559268691879794, 4.999327289942788966 ) ) ;
#99254 = B_SPLINE_CURVE_WITH_KNOTS ( 'NONE', 3,
 ( #70604, #53885, #84817, #31533, #63011, #16812 ),
 .UNSPECIFIED., .F., .F.,
 ( 4, 2, 4 ),
 ( 0.000000000000000000, 0.001380764517853249468, 0.002761529035706498936 ),
 .UNSPECIFIED. ) ;
#99255 = VECTOR ( 'NONE', #14275, 1000.000000000000000 ) ;
#99256 = CARTESIAN_POINT ( 'NONE',  ( 1.915021276000606454, 20.04344799065331628, -1.500000000000002220 ) ) ;
#99257 = CARTESIAN_POINT ( 'NONE',  ( -78.62287095715005592, -24.50321055353805022, 9.387540953477522265 ) ) ;
#99258 = ORIENTED_EDGE ( 'NONE', *, *, #20821, .T. ) ;
#99259 = CARTESIAN_POINT ( 'NONE',  ( -94.52287095715006160, -29.50247984919015209, -1.443849546365051806 ) ) ;
#99260 = CARTESIAN_POINT ( 'NONE',  ( 3.885606641962014329, -21.97303888676646721, -1.500000000000002220 ) ) ;
#99261 = ADVANCED_FACE ( 'NONE', ( #82617 ), #44064, .T. ) ;
#99262 = EDGE_CURVE ( 'NONE', #61766, #39981, #60802, .T. ) ;
#99263 = VERTEX_POINT ( 'NONE', #91722 ) ;
#99264 = ORIENTED_EDGE ( 'NONE', *, *, #30405, .F. ) ;
#99265 = CARTESIAN_POINT ( 'NONE',  ( -101.5468792378191978, -25.16257303515140009, 6.236250857614320076 ) ) ;
#99266 = CARTESIAN_POINT ( 'NONE',  ( -119.6228709571500701, -23.48786465467241769, 11.44779295918253759 ) ) ;
#99267 = LINE ( 'NONE', #29765, #76542 ) ;
#99268 = DIRECTION ( 'NONE',  ( -0.000000000000000000, -1.000000000000000000, 0.000000000000000000 ) ) ;
#99269 = CARTESIAN_POINT ( 'NONE',  ( -15.82668884360736961, -5.965225279485572685, 42.07822029717483758 ) ) ;
#99270 = CARTESIAN_POINT ( 'NONE',  ( 0.4223197742854877812, 19.52780805513575402, 11.49999999999998934 ) ) ;
#99271 = CIRCLE ( 'NONE', #58803, 3.349999999999998757 ) ;
#99272 = DIRECTION ( 'NONE',  ( 0.000000000000000000, 2.173523156925980399E-06, -0.9999999999976378895 ) ) ;
#99273 = CARTESIAN_POINT ( 'NONE',  ( -7.042111407433782055, -20.27750348750624099, 11.49999999999998934 ) ) ;
#99274 = CARTESIAN_POINT ( 'NONE',  ( -25.53440485667337612, -24.92775324654290969, 4.657482463092957659 ) ) ;
#99275 = PLANE ( 'NONE',  #69101 ) ;
#99276 = CARTESIAN_POINT ( 'NONE',  ( -10.34999999999999254, 3.299745742347187193E-16, 2.100000000000000977 ) ) ;
#99277 = CARTESIAN_POINT ( 'NONE',  ( 21.14566350062385780, -8.679158401671109857, -1.500000000000002220 ) ) ;
#99278 = EDGE_CURVE ( 'NONE', #25716, #6738, #62530, .T. ) ;
#99279 = CALENDAR_DATE ( 2026, 9, 10 ) ;
#99280 = CARTESIAN_POINT ( 'NONE',  ( -39.52287095715009002, -24.33832256527049154, 0.1851278514138551823 ) ) ;
#99281 = CARTESIAN_POINT ( 'NONE',  ( -29.58953762381674579, -24.57075707507987161, 1.056161308047962377 ) ) ;
#99282 = CARTESIAN_POINT ( 'NONE',  ( 18.80801646011137507, -6.797914457553222434, 11.49999999999999645 ) ) ;
#99283 = CARTESIAN_POINT ( 'NONE',  ( 14.76093561896379214, 3.316774720514426456, -28.39148769130089889 ) ) ;
#99284 = CARTESIAN_POINT ( 'NONE',  ( -123.6228709571500417, -24.33832256526968862, 0.1851278514119932828 ) ) ;
#99285 = DIRECTION ( 'NONE',  ( 0.000000000000000000, 0.9999999999976377785, 2.173523156925979975E-06 ) ) ;
#99286 = ORIENTED_EDGE ( 'NONE', *, *, #27112, .T. ) ;
#99287 = PLANE ( 'NONE',  #42894 ) ;
#99288 = CARTESIAN_POINT ( 'NONE',  ( -65.52287095715006160, -23.85229601348996553, 10.88205029486209341 ) ) ;
#99289 = EDGE_CURVE ( 'NONE', #21767, #61568, #55178, .T. ) ;
#99290 = CARTESIAN_POINT ( 'NONE',  ( 2.995010171738120786, 21.53247193037183038, -1.500000000000002220 ) ) ;
#99291 = CARTESIAN_POINT ( 'NONE',  ( -60.55620429048339304, -25.00158670708908915, 2.256160236439166855 ) ) ;
#99292 = CARTESIAN_POINT ( 'NONE',  ( 19.52168601723349894, 1.684101417132040979, -1.500000000000002220 ) ) ;
#99293 = CARTESIAN_POINT ( 'NONE',  ( -34.52287095715006160, -24.65952944569303895, 1.056160979905690134 ) ) ;
#99294 = ADVANCED_FACE ( 'NONE', ( #75994 ), #43659, .T. ) ;
#99295 = VECTOR ( 'NONE', #95940, 1000.000000000000114 ) ;
#99296 = ADVANCED_FACE ( 'NONE', ( #46071 ), #8994, .T. ) ;
#99297 = ORIENTED_EDGE ( 'NONE', *, *, #80237, .T. ) ;
#99298 = PERSON_AND_ORGANIZATION_ROLE ( 'classification_officer' ) ;
#99299 = LOCAL_TIME ( 0, 54, 15.00000000000000000, #85573 ) ;
#99300 = CARTESIAN_POINT ( 'NONE',  ( 5.949073730962466833, -5.965225279485572685, -27.94053387008862188 ) ) ;
#99301 = CARTESIAN_POINT ( 'NONE',  ( 2.989331223418256744, -5.876774720514424288, 21.46569930292093886 ) ) ;
#99302 = CARTESIAN_POINT ( 'NONE',  ( 12.01435098137705637, -16.61664908515649941, 11.49999999999999645 ) ) ;
#99303 = CARTESIAN_POINT ( 'NONE',  ( -56.52287095715008292, -24.66019654487199375, 8.947790411086122830 ) ) ;
#99304 = CARTESIAN_POINT ( 'NONE',  ( -10.75273025779354263, -6.376774720514426953, 16.96478738960562893 ) ) ;
#99305 = AXIS2_PLACEMENT_3D ( 'NONE', #38399, #840, #71362 ) ;
#99306 = ADVANCED_FACE ( 'NONE', ( #48071 ), #100317, .F. ) ;
#99307 = ORIENTED_EDGE ( 'NONE', *, *, #4434, .F. ) ;
#99308 = CARTESIAN_POINT ( 'NONE',  ( 15.97264540888995299, -3.316774720514426456, -27.93485543958162154 ) ) ;
#99309 = DIRECTION ( 'NONE',  ( -0.000000000000000000, -1.000000000000000000, -0.000000000000000000 ) ) ;
#99310 = CARTESIAN_POINT ( 'NONE',  ( -116.5939909856900982, -23.48786465467241769, 11.44779295918253759 ) ) ;
#99311 = DIRECTION ( 'NONE',  ( -3.773278334453079618E-23, 0.9999999999976377785, 2.173523156925979975E-06 ) ) ;
#99312 = CARTESIAN_POINT ( 'NONE',  ( 32.80655795465876423, 4.354682733740601108, -4.311478614910781992 ) ) ;
#99313 = CARTESIAN_POINT ( 'NONE',  ( 21.10734164270438029, -9.282589649079691085, 11.49999999999999645 ) ) ;
#99314 = CARTESIAN_POINT ( 'NONE',  ( 17.57702471007113232, 14.52005670271990034, 11.49999999999998934 ) ) ;
#99315 = CARTESIAN_POINT ( 'NONE',  ( -110.5904850311403180, -24.40133493613049964, 9.663955038902800609 ) ) ;
#99316 = B_SPLINE_SURFACE_WITH_KNOTS ( 'NONE', 3, 3, ( 
 ( #63869, #26276, #17662, #57252 ),
 ( #10547, #26777, #48634, #65866 ),
 ( #18654, #72462, #80559, #81063 ),
 ( #10049, #95785, #42018, #71966 ),
 ( #72962, #11543, #88682, #42517 ),
 ( #95291, #25775, #2955, #34391 ),
 ( #65368, #3949, #96785, #58237 ) ),
 .UNSPECIFIED., .F., .F., .F.,
 ( 4, 3, 4 ),
 ( 4, 4 ),
 ( 0.7945040050992241421, 0.8970133687736505657, 0.9995227324480768782 ),
 ( 0.9397327963690478292, 0.9411793639427116220 ),
 .UNSPECIFIED. ) ;
#99317 = CARTESIAN_POINT ( 'NONE',  ( 30.45304879119406039, -4.772774720514425972, -10.07140455160086390 ) ) ;
#99318 = CARTESIAN_POINT ( 'NONE',  ( 10.86264264036872440, 0.3587747205144257157, -28.05717073575603138 ) ) ;
#99319 = DIRECTION ( 'NONE',  ( -3.773278334453080206E-23, 0.9999999999976377785, 2.173523156925979975E-06 ) ) ;
#99320 = CARTESIAN_POINT ( 'NONE',  ( -103.9228709571500531, -23.47596703998600631, 11.44779298504227860 ) ) ;
#99321 = CARTESIAN_POINT ( 'NONE',  ( 15.24057855588860377, 15.72025634131890470, -1.500000000000002220 ) ) ;
#99322 = CARTESIAN_POINT ( 'NONE',  ( 7.343377932919765705, -5.876774720514422512, 21.31293098237466310 ) ) ;
#99323 = CARTESIAN_POINT ( 'NONE',  ( -87.50251410887271675, -24.66019654487200441, 8.947790411086112172 ) ) ;
#99324 = DIRECTION ( 'NONE',  ( -0.000000000000000000, 1.000000000000000000, -0.000000000000000000 ) ) ;
#99325 = DIRECTION ( 'NONE',  ( -3.773278334453079618E-23, 0.9999999999976377785, 2.173523156925979975E-06 ) ) ;
#99326 = DIRECTION ( 'NONE',  ( 0.000000000000000000, 0.000000000000000000, -1.000000000000000000 ) ) ;
#99327 = CARTESIAN_POINT ( 'NONE',  ( -107.6228709571500701, -23.47596703998600631, 11.44779298504227860 ) ) ;
#99328 = ORIENTED_EDGE ( 'NONE', *, *, #42788, .T. ) ;
#99329 = CARTESIAN_POINT ( 'NONE',  ( -7.302954156136775232, -19.11528491071161540, -1.500000000000002220 ) ) ;
#99330 = EDGE_LOOP ( 'NONE', ( #72527, #2482, #29927, #20338 ) ) ;
#99331 = VERTEX_POINT ( 'NONE', #30834 ) ;
#99332 = ORIENTED_EDGE ( 'NONE', *, *, #71874, .T. ) ;
#99333 = VERTEX_POINT ( 'NONE', #70908 ) ;
#99334 = CARTESIAN_POINT ( 'NONE',  ( 21.10734164270438029, -9.282589649079691085, 11.49999999999998934 ) ) ;
#99335 = CARTESIAN_POINT ( 'NONE',  ( -61.60404008566307965, -23.73766607897669800, -1.055555164236459120 ) ) ;
#99336 = CARTESIAN_POINT ( 'NONE',  ( 16.63042848490962555, -11.55671354112608817, -1.500000000000002220 ) ) ;
#99337 = CIRCLE ( 'NONE', #73436, 129.7684398600581517 ) ;
#99338 = VERTEX_POINT ( 'NONE', #93223 ) ;
#99339 = CARTESIAN_POINT ( 'NONE',  ( -27.14488594699098201, -24.92687995790785038, 3.118813907533751983 ) ) ;
#99340 = CARTESIAN_POINT ( 'NONE',  ( -41.86252025446345471, -25.30041590689949160, 4.388877412580752591 ) ) ;
#99341 = CARTESIAN_POINT ( 'NONE',  ( -128.5228709571500758, -23.47596703998600631, 11.44779298504227683 ) ) ;
#99342 = CARTESIAN_POINT ( 'NONE',  ( -99.62961828089473215, -24.15620529776628445, 10.23563542870660115 ) ) ;
#99344 = ORIENTED_EDGE ( 'NONE', *, *, #82517, .T. ) ;
#99343 = CARTESIAN_POINT ( 'NONE',  ( 5.397486108853063236, 20.74927772461418485, 11.49999999999999645 ) ) ;
#99345 = PLANE ( 'NONE',  #69475 ) ;
#99347 = AXIS2_PLACEMENT_3D ( 'NONE', #94689, #24669, #71869 ) ;
#99346 = FACE_OUTER_BOUND ( 'NONE', #27380, .T. ) ;
#99348 = ORIENTED_EDGE ( 'NONE', *, *, #724, .F. ) ;
#99349 = CARTESIAN_POINT ( 'NONE',  ( -13.38394104848841693, -15.81244124602197765, 11.49999999999998934 ) ) ;
#99351 = EDGE_LOOP ( 'NONE', ( #77126, #83011, #17274, #43706 ) ) ;
#99350 = CARTESIAN_POINT ( 'NONE',  ( 22.81105451610979173, 1.477225279485574028, -18.46691820600746681 ) ) ;
#99352 = EDGE_CURVE ( 'NONE', #61563, #30238, #43136, .T. ) ;
#99353 = LINE ( 'NONE', #30348, #87513 ) ;
#99354 = ORIENTED_EDGE ( 'NONE', *, *, #30978, .T. ) ;
#99355 = EDGE_CURVE ( 'NONE', #74013, #8750, #32334, .T. ) ;
#99356 = CARTESIAN_POINT ( 'NONE',  ( 4.782775879418006859, -5.876774720514404748, 18.83817099474236656 ) ) ;
#99357 = EDGE_LOOP ( 'NONE', ( #9535, #74552, #91143, #45817 ) ) ;
#99358 = EDGE_CURVE ( 'NONE', #19622, #37096, #84266, .T. ) ;
#99359 = CARTESIAN_POINT ( 'NONE',  ( 16.22650188657148362, -14.79325693486936188, 11.49999999999999645 ) ) ;
#99360 = EDGE_CURVE ( 'NONE', #50678, #66840, #51582, .T. ) ;
#99361 = CARTESIAN_POINT ( 'NONE',  ( -37.66610885914807483, -23.48786465467240703, 11.44779295918255180 ) ) ;
#99362 = CARTESIAN_POINT ( 'NONE',  ( 1.861690257272737847, 22.46465895387273903, 11.49999999999998934 ) ) ;
#99363 = ADVANCED_FACE ( 'NONE', ( #84617 ), #63815, .F. ) ;
#99364 = CARTESIAN_POINT ( 'NONE',  ( 4.154569570224219355, 20.57273982587956240, 11.49999999999998934 ) ) ;
#99365 = FACE_OUTER_BOUND ( 'NONE', #59606, .T. ) ;
#99366 = EDGE_CURVE ( 'NONE', #53195, #58571, #1894, .T. ) ;
#99367 = AXIS2_PLACEMENT_3D ( 'NONE', #72497, #65901, #10581 ) ;
#99368 = CARTESIAN_POINT ( 'NONE',  ( 4.621320343559262689, 12.74999999999999645, 0.000000000000000000 ) ) ;
#99369 = ORIENTED_EDGE ( 'NONE', *, *, #9467, .T. ) ;
#99370 = ORIENTED_EDGE ( 'NONE', *, *, #17258, .T. ) ;
#99371 = ORIENTED_EDGE ( 'NONE', *, *, #27384, .T. ) ;
#99372 = CARTESIAN_POINT ( 'NONE',  ( -128.6228709571500417, -24.66019654487200441, 8.947790411086121054 ) ) ;
#99373 = CARTESIAN_POINT ( 'NONE',  ( -20.49900048275977227, -6.559984590058941301, -1.500000000000002220 ) ) ;
#99374 = VECTOR ( 'NONE', #64147, 1000.000000000000114 ) ;
#99375 = CARTESIAN_POINT ( 'NONE',  ( -105.5228709571500900, -24.14406661686766142, 10.28769366194078216 ) ) ;
#99376 = ORIENTED_EDGE ( 'NONE', *, *, #52896, .F. ) ;
#99377 = CARTESIAN_POINT ( 'NONE',  ( -20.67868931609407213, -4.308284118179648736, 11.49999999999998934 ) ) ;
#99378 = DIRECTION ( 'NONE',  ( -1.000000000000000000, 0.000000000000000000, 0.000000000000000000 ) ) ;
#99379 = CARTESIAN_POINT ( 'NONE',  ( -64.59268794064412589, -24.15543982623906771, -0.2315651400026674800 ) ) ;
#99380 = CARTESIAN_POINT ( 'NONE',  ( -130.5728709571500588, -23.47593901973090524, -1.443836447538995982 ) ) ;
#99381 = CARTESIAN_POINT ( 'NONE',  ( 11.41483471809167405, 3.316774720514427344, -27.05170832580397189 ) ) ;
#99382 = CARTESIAN_POINT ( 'NONE',  ( -56.52287095715006870, -24.64965694238407323, 8.947790433994201820 ) ) ;
#99383 = CARTESIAN_POINT ( 'NONE',  ( 13.49617185221842952, 17.62045156095830123, -1.500000000000002220 ) ) ;
#99384 = CIRCLE ( 'NONE', #41096, 1.836000000000002075 ) ;
#99385 = CARTESIAN_POINT ( 'NONE',  ( -81.51736153681817143, -23.73791477778911840, 11.05961554403170943 ) ) ;
#99386 = B_SPLINE_CURVE_WITH_KNOTS ( 'NONE', 3,
 ( #74978, #98820, #98316, #13580, #37929, #44549, #100300, #38429 ),
 .UNSPECIFIED., .F., .F.,
 ( 4, 2, 2, 4 ),
 ( 6.391158118955161585E-06, 0.002007136338672919646, 0.003007508928949900393, 0.004007881519226880705 ),
 .UNSPECIFIED. ) ;
#99387 = EDGE_CURVE ( 'NONE', #100167, #37824, #68466, .T. ) ;
#99388 = VERTEX_POINT ( 'NONE', #50561 ) ;
#99389 = FACE_OUTER_BOUND ( 'NONE', #59616, .T. ) ;
#99390 = CARTESIAN_POINT ( 'NONE',  ( 12.40597316965629560, 5.152774720514427642, -26.28458722401733993 ) ) ;
#99391 = CARTESIAN_POINT ( 'NONE',  ( -41.86995616089613748, -25.27955781699870741, 4.210709737955789400 ) ) ;
#99392 = CARTESIAN_POINT ( 'NONE',  ( -100.5618440256851329, -23.48783264082477018, -1.443836473390090580 ) ) ;
#99393 = EDGE_CURVE ( 'NONE', #44655, #61715, #35345, .T. ) ;
#99394 = CARTESIAN_POINT ( 'NONE',  ( -11.39837868854680814, -15.77482985264681403, -1.500000000000002220 ) ) ;
#99395 = CARTESIAN_POINT ( 'NONE',  ( 8.370372042246325250, 19.68514866842044242, -1.500000000000002220 ) ) ;
#99396 = PLANE ( 'NONE',  #88770 ) ;
#99397 = DIRECTION ( 'NONE',  ( 0.000000000000000000, -2.173523156925980399E-06, 0.9999999999976378895 ) ) ;
#99398 = CARTESIAN_POINT ( 'NONE',  ( -72.52287095715010423, -23.72773821059536914, 11.05748984161097503 ) ) ;
#99399 = CARTESIAN_POINT ( 'NONE',  ( 4.621320343559255583, 11.49999999999999645, 0.000000000000000000 ) ) ;
#99400 = CARTESIAN_POINT ( 'NONE',  ( 15.43685675143394498, -16.52047792065556564, -1.500000000000002220 ) ) ;
#99401 = B_SPLINE_SURFACE_WITH_KNOTS ( 'NONE', 3, 3, ( 
 ( #31272, #55633, #95181, #24653 ),
 ( #77929, #39390, #54624, #17048 ),
 ( #79448, #48015, #85558, #70344 ),
 ( #12434, #49020, #79951, #20052 ),
 ( #10437, #74340, #57633, #96187 ),
 ( #97180, #28170, #50507, #11441 ),
 ( #65264, #42905, #95682, #43404 ) ),
 .UNSPECIFIED., .F., .F., .F.,
 ( 4, 3, 4 ),
 ( 4, 4 ),
 ( 0.0004766839783816290664, 0.1029713700210892202, 0.2054660560637968092 ),
 ( 0.7696897931818312832, 0.7710576511941856781 ),
 .UNSPECIFIED. ) ;
#99402 = ORIENTED_EDGE ( 'NONE', *, *, #52288, .T. ) ;
#99403 = CARTESIAN_POINT ( 'NONE',  ( -128.5228709571500758, -24.65952944569305316, 1.056160979905707675 ) ) ;
#99404 = DIRECTION ( 'NONE',  ( 1.000000000000000000, 0.000000000000000000, 0.000000000000000000 ) ) ;
#99405 = CARTESIAN_POINT ( 'NONE',  ( 9.171884637996585710, -17.55225146786146695, 11.49999999999999645 ) ) ;
#99406 = CARTESIAN_POINT ( 'NONE',  ( 12.66784028006542151, 2.682774720514427003, -27.12025593822526304 ) ) ;
#99407 = ORIENTED_EDGE ( 'NONE', *, *, #61396, .F. ) ;
#99408 = CARTESIAN_POINT ( 'NONE',  ( -59.52287095715009002, -23.47593901973090524, -1.443836447538997092 ) ) ;
#99409 = CARTESIAN_POINT ( 'NONE',  ( -80.62287095715005592, -29.50250786944525672, 11.44777988621623521 ) ) ;
#99410 = CARTESIAN_POINT ( 'NONE',  ( 3.837509532605410278, -21.31939230324424628, 11.49999999999998934 ) ) ;
#99411 = CARTESIAN_POINT ( 'NONE',  ( -27.16293832639682293, -24.78279603735616732, 7.495382070342732739 ) ) ;
#99412 = CARTESIAN_POINT ( 'NONE',  ( 19.38287969867323213, 0.6573286442255052986, -1.500000000000002220 ) ) ;
#99413 = DIRECTION ( 'NONE',  ( -0.000000000000000000, -1.000000000000000000, -0.000000000000000000 ) ) ;
#99414 = CARTESIAN_POINT ( 'NONE',  ( -129.5228709571501042, -23.72773821059536914, 11.05748984161097503 ) ) ;
#99415 = EDGE_CURVE ( 'NONE', #15961, #46809, #3408, .T. ) ;
#99416 = CARTESIAN_POINT ( 'NONE',  ( 1.944447714513537262, -19.71154682592685958, 11.49999999999998934 ) ) ;
#99417 = ORIENTED_EDGE ( 'NONE', *, *, #100274, .F. ) ;
#99418 = AXIS2_PLACEMENT_3D ( 'NONE', #81002, #19590, #66295 ) ;
#99419 = CARTESIAN_POINT ( 'NONE',  ( 16.59675031405745571, -11.69241480613374407, 11.49999999999999645 ) ) ;
#99420 = CARTESIAN_POINT ( 'NONE',  ( -80.64006940006906632, -24.15503026093913164, -0.2815557561904567518 ) ) ;
#99421 = EDGE_CURVE ( 'NONE', #33854, #35854, #28554, .T. ) ;
#99422 = CARTESIAN_POINT ( 'NONE',  ( 6.316142118701270292, 1.335431525194935798, 19.26533332368850182 ) ) ;
#99423 = VERTEX_POINT ( 'NONE', #58185 ) ;
#99424 = CARTESIAN_POINT ( 'NONE',  ( -102.5574997761123939, -23.73791477778911840, 11.05961554403170410 ) ) ;
#99425 = CARTESIAN_POINT ( 'NONE',  ( 30.93860345374796594, 5.515143950957555496, 14.99689261510125249 ) ) ;
#99426 = CARTESIAN_POINT ( 'NONE',  ( -49.53270844027763786, -25.25214452993709813, 5.057855935191842178 ) ) ;
#99427 = B_SPLINE_CURVE_WITH_KNOTS ( 'NONE', 3,
 ( #92559, #77326, #53527, #77820 ),
 .UNSPECIFIED., .F., .F.,
 ( 4, 4 ),
 ( 1.387778780781445521E-17, 9.999999999997510880E-05 ),
 .UNSPECIFIED. ) ;
#99428 = CARTESIAN_POINT ( 'NONE',  ( -47.55620429048340014, -23.47593901973091235, -1.443836447539009749 ) ) ;
#99429 = CARTESIAN_POINT ( 'NONE',  ( 24.50000000000000000, -0.9000000000000000222, -1.103411337323757957 ) ) ;
#99430 = CARTESIAN_POINT ( 'NONE',  ( 4.397486433803790007, -19.56896378179033036, 11.49999999999998934 ) ) ;
#99431 = DIRECTION ( 'NONE',  ( -0.000000000000000000, 1.000000000000000000, -0.000000000000000000 ) ) ;
#99432 = ORIENTED_EDGE ( 'NONE', *, *, #77465, .T. ) ;
#99433 = CARTESIAN_POINT ( 'NONE',  ( -15.87499999999997868, 0.000000000000000000, 0.000000000000000000 ) ) ;
#99434 = CARTESIAN_POINT ( 'NONE',  ( 18.56524475492553705, -13.42312393814442650, 11.49999999999999645 ) ) ;
#99435 = CARTESIAN_POINT ( 'NONE',  ( -102.5228709571500616, -23.72747288104470442, -1.053458166803225016 ) ) ;
#99436 = FACE_OUTER_BOUND ( 'NONE', #19016, .T. ) ;
#99437 = CARTESIAN_POINT ( 'NONE',  ( -59.62287095715003460, -23.72747288104441665, -1.053458166803663332 ) ) ;
#99438 = DIRECTION ( 'NONE',  ( 3.773278334444167608E-23, -1.000000000000000000, 0.000000000000000000 ) ) ;
#99439 = CARTESIAN_POINT ( 'NONE',  ( -28.98875734969026041, -5.965225279485572685, 17.86602280011862476 ) ) ;
#99440 = AXIS2_PLACEMENT_3D ( 'NONE', #35413, #96798, #11553 ) ;
#99441 = DIRECTION ( 'NONE',  ( 1.000000000000000000, 0.000000000000000000, 0.000000000000000000 ) ) ;
#99442 = ORIENTED_EDGE ( 'NONE', *, *, #27688, .T. ) ;
#99443 = CARTESIAN_POINT ( 'NONE',  ( -11.21218820807429140, -16.99972530465495169, -1.500000000000002220 ) ) ;
#99444 = VECTOR ( 'NONE', #45514, 1000.000000000000000 ) ;
#99445 = ORIENTED_EDGE ( 'NONE', *, *, #51790, .T. ) ;
#99446 = CARTESIAN_POINT ( 'NONE',  ( 22.74528686061176685, 3.085755641335488964, 11.49999999999998934 ) ) ;
#99447 = CARTESIAN_POINT ( 'NONE',  ( -115.5562042904833788, -23.48786465467242124, 11.44779295918253759 ) ) ;
#99448 = VERTEX_POINT ( 'NONE', #17612 ) ;
#99449 = CARTESIAN_POINT ( 'NONE',  ( -95.62287095715005592, -29.50248528299804818, 1.056150453629042030 ) ) ;
#99450 = CARTESIAN_POINT ( 'NONE',  ( -67.52287095715006160, -24.64965694238407323, 8.947790433994200043 ) ) ;
#99451 = CARTESIAN_POINT ( 'NONE',  ( -96.62287095715009855, -24.33832256526969928, 0.1851278514119889529 ) ) ;
#99453 = ORIENTED_EDGE ( 'NONE', *, *, #63162, .F. ) ;
#99452 = CARTESIAN_POINT ( 'NONE',  ( -4.730540317195566224, 20.75322969461001676, 11.49999999999999645 ) ) ;
#99454 = ORIENTED_EDGE ( 'NONE', *, *, #61005, .F. ) ;
#99455 = CARTESIAN_POINT ( 'NONE',  ( 8.998109643811913472, -20.30750954041392120, -1.500000000000002220 ) ) ;
#99456 = CARTESIAN_POINT ( 'NONE',  ( -3.087264924507187924, 20.40197043678811539, 11.49999999999998934 ) ) ;
#99457 = ORIENTED_EDGE ( 'NONE', *, *, #79417, .F. ) ;
#99458 = ORIENTED_EDGE ( 'NONE', *, *, #56785, .F. ) ;
#99459 = EDGE_CURVE ( 'NONE', #67442, #95555, #5559, .T. ) ;
#99460 = CARTESIAN_POINT ( 'NONE',  ( -109.2582164645601779, -25.31627313540426627, 5.068133679678900272 ) ) ;
#99461 = CARTESIAN_POINT ( 'NONE',  ( -55.22287095715006444, -23.47596703998600276, 11.44779298504227860 ) ) ;
#99462 = ORIENTED_EDGE ( 'NONE', *, *, #31686, .F. ) ;
#99463 = ADVANCED_FACE ( 'NONE', ( #48584 ), #42962, .T. ) ;
#99464 = ORIENTED_EDGE ( 'NONE', *, *, #81631, .T. ) ;
#99465 = DIRECTION ( 'NONE',  ( -0.000000000000000000, -1.000000000000000000, -0.000000000000000000 ) ) ;
#99466 = CARTESIAN_POINT ( 'NONE',  ( -124.6228709571500559, -29.50250786944525672, 11.44777988621622811 ) ) ;
#99467 = CARTESIAN_POINT ( 'NONE',  ( 19.25983760003161294, 7.974354923662064998, -1.500000000000002220 ) ) ;
#99468 = CARTESIAN_POINT ( 'NONE',  ( 0.2638585030419089428, -21.76204025362994798, 11.49999999999999645 ) ) ;
#99469 = VECTOR ( 'NONE', #66166, 1000.000000000000114 ) ;
#99470 = EDGE_CURVE ( 'NONE', #42504, #37822, #83008, .T. ) ;
#99471 = CARTESIAN_POINT ( 'NONE',  ( -51.61612386428029708, -25.12985818678743399, 7.066459036000934724 ) ) ;
#99472 = CARTESIAN_POINT ( 'NONE',  ( 32.98733314340959311, -5.965225279485572685, 2.074222136288530027 ) ) ;
#99473 = CARTESIAN_POINT ( 'NONE',  ( -6.716530693746936898, -21.44081863256500142, -1.500000000000002220 ) ) ;
#99474 = EDGE_CURVE ( 'NONE', #17843, #16362, #88133, .T. ) ;
#99475 = CARTESIAN_POINT ( 'NONE',  ( -50.64790834543075704, -25.31296758314977779, 4.705120360976434490 ) ) ;
#99476 = ORIENTED_EDGE ( 'NONE', *, *, #18024, .F. ) ;
#99477 = CARTESIAN_POINT ( 'NONE',  ( -50.52287095715006160, -24.63345952396255001, 9.038047939301510070 ) ) ;
#99478 = CARTESIAN_POINT ( 'NONE',  ( -57.52287095715005449, -24.65952944569304606, 1.056160979905695463 ) ) ;
#99479 = CIRCLE ( 'NONE', #15026, 1.835999999999931465 ) ;
#99480 = ADVANCED_FACE ( 'NONE', ( #89128 ), #76907, .T. ) ;
#99481 = EDGE_LOOP ( 'NONE', ( #93006, #94840, #82322, #48665 ) ) ;
#99482 = ADVANCED_FACE ( 'NONE', ( #37827 ), #46154, .T. ) ;
#99483 = VERTEX_POINT ( 'NONE', #13483 ) ;
#99484 = FACE_OUTER_BOUND ( 'NONE', #75852, .T. ) ;
#99485 = ORIENTED_EDGE ( 'NONE', *, *, #48715, .F. ) ;
#99486 = CARTESIAN_POINT ( 'NONE',  ( -19.99249555334884221, 7.427959064407942513, -1.500000000000002220 ) ) ;
#99487 = EDGE_LOOP ( 'NONE', ( #33956, #22568, #18043, #97448 ) ) ;
#99488 = CARTESIAN_POINT ( 'NONE',  ( -5.941268476065055815, -5.876774720514417183, 20.11414146978959749 ) ) ;
#99489 = CARTESIAN_POINT ( 'NONE',  ( -19.58807393344005376, -7.628504261335002923, -1.500000000000002220 ) ) ;
#99490 = CARTESIAN_POINT ( 'NONE',  ( -30.48115194396658012, -24.75308503270343152, 1.363670884829966123 ) ) ;
#99491 = CARTESIAN_POINT ( 'NONE',  ( -41.46611000704998418, -25.28892616455412323, 4.188173659901108792 ) ) ;
#99492 = DIRECTION ( 'NONE',  ( -0.7682573101345366862, 0.000000000000000000, 0.6401411605457395515 ) ) ;
#99493 = CARTESIAN_POINT ( 'NONE',  ( 21.66556372666567754, 3.824538051775513647, -1.500000000000002220 ) ) ;
#99494 = CARTESIAN_POINT ( 'NONE',  ( -87.51096306996832652, -24.15543982623908192, -0.2315651400026449980 ) ) ;
#99495 = EDGE_LOOP ( 'NONE', ( #69019, #34133, #62800, #40101 ) ) ;
#99496 = PLANE ( 'NONE',  #80841 ) ;
#99497 = CARTESIAN_POINT ( 'NONE',  ( -84.54456340005228299, -24.51419770103157347, 9.386484678747175181 ) ) ;
#99498 = PLANE ( 'NONE',  #66813 ) ;
#99499 = CARTESIAN_POINT ( 'NONE',  ( -0.008164624327092516801, -22.94430252198347375, 6.147794833475636267 ) ) ;
#99500 = CARTESIAN_POINT ( 'NONE',  ( 10.72677997844354536, -18.41129465587203740, 11.49999999999998934 ) ) ;
#99501 = CARTESIAN_POINT ( 'NONE',  ( -98.59115901530434201, -24.15620529776628800, 10.23563542870660292 ) ) ;
#99502 = DIRECTION ( 'NONE',  ( -0.6559908753439240847, -0.4874460344622444929, -0.5762571777883070956 ) ) ;
#99503 = CARTESIAN_POINT ( 'NONE',  ( -122.6228709571500559, -24.65952944569305316, 1.056160979905706343 ) ) ;
#99504 = FACE_OUTER_BOUND ( 'NONE', #58742, .T. ) ;
#99505 = CARTESIAN_POINT ( 'NONE',  ( -21.66288588771858770, -5.991481186202806342, -1.500000000000002220 ) ) ;
#99506 = CARTESIAN_POINT ( 'NONE',  ( 0.2450472757604422180, -5.405843919193447533, -9.000000000000000000 ) ) ;
#99507 = ORIENTED_EDGE ( 'NONE', *, *, #16946, .F. ) ;
#99508 = LINE ( 'NONE', #84292, #32024 ) ;
#99509 = CARTESIAN_POINT ( 'NONE',  ( 19.59400933563812330, 0.1774559437341752532, 11.49999999999999645 ) ) ;
#99510 = CARTESIAN_POINT ( 'NONE',  ( -125.6228709571500559, -24.83602698348162363, 1.605859176311269954 ) ) ;
#99511 = CARTESIAN_POINT ( 'NONE',  ( -76.52287095715007581, -24.64965694238408034, 8.947790433994198267 ) ) ;
#99512 = VERTEX_POINT ( 'NONE', #89623 ) ;
#99513 = CARTESIAN_POINT ( 'NONE',  ( -69.45716761675758733, -25.30512913829650401, 5.118693047570955557 ) ) ;
#99514 = CARTESIAN_POINT ( 'NONE',  ( -124.5120848053583131, -25.40067164642711361, 5.394116434732633358 ) ) ;
#99515 = CARTESIAN_POINT ( 'NONE',  ( -124.5541588009910470, -24.66019654487200441, 8.947790411086108620 ) ) ;
#99516 = DIRECTION ( 'NONE',  ( 1.000000000000000000, -0.000000000000000000, 0.000000000000000000 ) ) ;
#99517 = CARTESIAN_POINT ( 'NONE',  ( -17.00503767097633556, -9.977476526402845991, -1.500000000000002220 ) ) ;
#99518 = ORIENTED_EDGE ( 'NONE', *, *, #8115, .T. ) ;
#99519 = DIRECTION ( 'NONE',  ( 0.000000000000000000, 0.000000000000000000, -1.000000000000000000 ) ) ;
#99520 = EDGE_CURVE ( 'NONE', #54808, #75788, #43459, .T. ) ;
#99521 = VECTOR ( 'NONE', #97811, 1000.000000000000114 ) ;
#99522 = APPROVAL_ROLE ( '' ) ;
#99523 = ADVANCED_FACE ( 'NONE', ( #20102 ), #5383, .T. ) ;
#99524 = ORIENTED_EDGE ( 'NONE', *, *, #67091, .T. ) ;
#99525 = DIRECTION ( 'NONE',  ( 0.000000000000000000, 1.000000000000000000, 0.000000000000000000 ) ) ;
#99526 = CARTESIAN_POINT ( 'NONE',  ( -1.371775545366004545, -6.376774720514413630, 20.39230070883894186 ) ) ;
#99527 = CARTESIAN_POINT ( 'NONE',  ( -55.52866950233528343, -24.92564183028978775, 1.928384488918253092 ) ) ;
#99528 = CARTESIAN_POINT ( 'NONE',  ( -99.33721417192995773, -25.03145088751183422, 7.148561016989910755 ) ) ;
#99529 = CARTESIAN_POINT ( 'NONE',  ( 5.328346181807287252, -6.376774720514418959, 20.81670806933143680 ) ) ;
#99530 = DIRECTION ( 'NONE',  ( 1.046287966022745640E-14, 0.000000000000000000, -1.000000000000000000 ) ) ;
#99531 = CARTESIAN_POINT ( 'NONE',  ( 27.53860345374808105, -1.477225279485574028, 19.84760796525321780 ) ) ;
#99532 = CARTESIAN_POINT ( 'NONE',  ( -12.72357806474857966, 15.40231687525621318, 11.49999999999998934 ) ) ;
#99533 = VECTOR ( 'NONE', #58796, 1000.000000000000114 ) ;
#99534 = CARTESIAN_POINT ( 'NONE',  ( -32.50560601784287229, -24.86181184613565165, 1.747789954104514987 ) ) ;
#99535 = CARTESIAN_POINT ( 'NONE',  ( -45.48403108558225227, -24.63419186844611630, 9.035850630976932862 ) ) ;
#99536 = ORIENTED_EDGE ( 'NONE', *, *, #84962, .T. ) ;
#99537 = CARTESIAN_POINT ( 'NONE',  ( 6.431460800610004469, -5.356774720514426491, -25.38187206382939465 ) ) ;
#99538 = DIRECTION ( 'NONE',  ( -3.773278334453079030E-23, 0.9999999999976377785, 2.173523156925979128E-06 ) ) ;
#99539 = CARTESIAN_POINT ( 'NONE',  ( 4.712727796232550226, 6.376774720514426953, -25.55789472434992859 ) ) ;
#99540 = CARTESIAN_POINT ( 'NONE',  ( -20.27875734969026311, -4.543225279485573864, 21.75402280011862644 ) ) ;
#99541 = CARTESIAN_POINT ( 'NONE',  ( -128.5228709571500758, -29.50248528299804818, 1.056150453629047137 ) ) ;
#99542 = EDGE_CURVE ( 'NONE', #57842, #3242, #32146, .T. ) ;
#99543 = CARTESIAN_POINT ( 'NONE',  ( -2.070328576748420524, -5.876774720514410077, 19.46575348430201657 ) ) ;
#99544 = CARTESIAN_POINT ( 'NONE',  ( -79.62287095715011276, -24.51387760970725083, 9.387446482453428942 ) ) ;
#99545 = CARTESIAN_POINT ( 'NONE',  ( -112.6228709571500559, -24.64898659630368272, 1.056161002820831474 ) ) ;
#99546 = ORIENTED_EDGE ( 'NONE', *, *, #5396, .T. ) ;
#99547 = CARTESIAN_POINT ( 'NONE',  ( 0.7435384974594729801, 20.27106041150680937, 11.49999999999998934 ) ) ;
#99548 = CARTESIAN_POINT ( 'NONE',  ( -76.62287095715007013, -23.47596703998600631, 11.44779298504227860 ) ) ;
#99549 = PLANE ( 'NONE',  #19341 ) ;
#99550 = B_SPLINE_CURVE_WITH_KNOTS ( 'NONE', 3,
 ( #69674, #45345, #23981, #54953, #84389, #16371, #61071, #30600 ),
 .UNSPECIFIED., .F., .F.,
 ( 4, 2, 2, 4 ),
 ( 0.000000000000000000, 0.002001079623178217588, 0.003001619434767328985, 0.004002159246356440381 ),
 .UNSPECIFIED. ) ;
#99551 = DIRECTION ( 'NONE',  ( 0.000000000000000000, -1.000000000000000000, 0.000000000000000000 ) ) ;
#99552 = ORIENTED_EDGE ( 'NONE', *, *, #70633, .T. ) ;
#99553 = CARTESIAN_POINT ( 'NONE',  ( -0.7395115731254252589, 18.09566585216508727, -8.999999999999998224 ) ) ;
#99554 = DIRECTION ( 'NONE',  ( 0.000000000000000000, 0.000000000000000000, 1.000000000000000000 ) ) ;
#99555 = CARTESIAN_POINT ( 'NONE',  ( 6.436487395234643749, 19.08016507665710648, -1.500000000000002220 ) ) ;
#99556 = CARTESIAN_POINT ( 'NONE',  ( 21.06685942672242362, 1.161445541649065882, 11.49999999999999645 ) ) ;
#99557 = VECTOR ( 'NONE', #76442, 1000.000000000000000 ) ;
#99558 = LINE ( 'NONE', #48192, #7691 ) ;
#99559 = CARTESIAN_POINT ( 'NONE',  ( -11.88820881604258339, -18.65297325734525913, 11.49999999999998934 ) ) ;
#99560 = CARTESIAN_POINT ( 'NONE',  ( -20.49763986188970932, -1.003951800832726615, -1.500000000000002220 ) ) ;
#99561 = CARTESIAN_POINT ( 'NONE',  ( -41.62287095715006302, -24.65952944569303895, 1.056160979905692576 ) ) ;
#99562 = CARTESIAN_POINT ( 'NONE',  ( -60.51214155151011198, -23.85016227208580375, -0.8807180028928355275 ) ) ;
#99563 = VERTEX_POINT ( 'NONE', #44452 ) ;
#99564 = DIRECTION ( 'NONE',  ( 0.000000000000000000, -0.9999999999976377785, -2.173523156925979975E-06 ) ) ;
#99565 = ORIENTED_EDGE ( 'NONE', *, *, #30701, .F. ) ;
#99566 = CARTESIAN_POINT ( 'NONE',  ( -35.52287095715008292, -23.85229601348997264, 10.88205029486209696 ) ) ;
#99567 = B_SPLINE_SURFACE_WITH_KNOTS ( 'NONE', 3, 3, ( 
 ( #15224, #20826, #44186, #60422 ),
 ( #37566, #21822, #52298, #60917 ),
 ( #91846, #28951, #52798, #29443 ),
 ( #53801, #51802, #76607, #38060 ),
 ( #30453, #83733, #36066, #75122 ),
 ( #44688, #14213, #6113, #61417 ),
 ( #67529, #84230, #5615, #67040 ) ),
 .UNSPECIFIED., .F., .F., .F.,
 ( 4, 3, 4 ),
 ( 4, 4 ),
 ( 0.7945040050992234759, 0.8970133687736497885, 0.9995227324480761011 ),
 ( 0.5296285832068964305, 0.5308858194615871939 ),
 .UNSPECIFIED. ) ;
#99568 = CARTESIAN_POINT ( 'NONE',  ( -87.55620429048337883, -24.66019654487199730, 8.947790411086126383 ) ) ;
#99569 = VERTEX_POINT ( 'NONE', #74393 ) ;
#99570 = ORIENTED_EDGE ( 'NONE', *, *, #94608, .F. ) ;
#99571 = ORIENTED_EDGE ( 'NONE', *, *, #97937, .T. ) ;
#99572 = DIRECTION ( 'NONE',  ( -3.773278334453079030E-23, 0.9999999999976377785, 2.173523156925979128E-06 ) ) ;
#99573 = CARTESIAN_POINT ( 'NONE',  ( -40.62287095715005592, -23.48783264082478084, -1.443836473390072817 ) ) ;
#99574 = CARTESIAN_POINT ( 'NONE',  ( -68.55932689068598052, -23.73791477778911840, 11.05961554403170943 ) ) ;
#99575 = CARTESIAN_POINT ( 'NONE',  ( -20.25002411749221665, -3.895867502427604379, -1.500000000000002220 ) ) ;
#99576 = CARTESIAN_POINT ( 'NONE',  ( -15.70146493180990888, -14.86199287721409590, 11.49999999999999645 ) ) ;
#99577 = ORIENTED_EDGE ( 'NONE', *, *, #24926, .T. ) ;
#99578 = EDGE_CURVE ( 'NONE', #87143, #17038, #98214, .T. ) ;
#99579 = CARTESIAN_POINT ( 'NONE',  ( -100.5228709571500616, -23.47596703998600631, 11.44779298504228215 ) ) ;
#99580 = CARTESIAN_POINT ( 'NONE',  ( -60.62287095715007013, -24.82558206586144323, 1.605769216559442158 ) ) ;
#99581 = CARTESIAN_POINT ( 'NONE',  ( -13.97600220251353953, -17.46790257487896270, -1.500000000000002220 ) ) ;
#99582 = LINE ( 'NONE', #36219, #61055 ) ;
#99583 = CARTESIAN_POINT ( 'NONE',  ( 1.754398552524170762, 17.92127466780477718, 9.000000000000000000 ) ) ;
#99584 = ORIENTED_EDGE ( 'NONE', *, *, #99948, .T. ) ;
#99585 = CARTESIAN_POINT ( 'NONE',  ( -100.5548270777744335, -25.31262531776226510, 4.733991798650357019 ) ) ;
#99586 = CARTESIAN_POINT ( 'NONE',  ( 6.727764423076923350, -6.376774720514413630, 19.76442307692307665 ) ) ;
#99587 = ADVANCED_FACE ( 'NONE', ( #75379 ), #28259, .T. ) ;
#99588 = CARTESIAN_POINT ( 'NONE',  ( -20.36979505965413395, -4.774807507659313721, -1.500000000000002220 ) ) ;
#99589 = EDGE_CURVE ( 'NONE', #52189, #50219, #32200, .T. ) ;
#99590 = VERTEX_POINT ( 'NONE', #30202 ) ;
#99591 = VECTOR ( 'NONE', #52783, 1000.000000000000227 ) ;
#99593 = EDGE_LOOP ( 'NONE', ( #80785, #53999, #69311, #75542 ) ) ;
#99592 = CARTESIAN_POINT ( 'NONE',  ( -67.55389080268135160, -23.96169478059713853, 10.65365249895717881 ) ) ;
#99594 = EDGE_LOOP ( 'NONE', ( #20106, #71109, #26835, #48225, #32877, #61815, #68660, #68311, #49386, #576, #50909, #70423, #69551, #42840 ) ) ;
#99595 = CARTESIAN_POINT ( 'NONE',  ( -109.6276321201155923, -24.15620529776628800, 10.23563542870660115 ) ) ;
#99596 = CARTESIAN_POINT ( 'NONE',  ( -21.01389645921736360, -2.595061309317715281, -1.500000000000002220 ) ) ;
#99597 = VERTEX_POINT ( 'NONE', #69275 ) ;
#99598 = CARTESIAN_POINT ( 'NONE',  ( -117.5924212553219661, -23.73766607897670511, -1.055555164236445798 ) ) ;
#99599 = DIRECTION ( 'NONE',  ( 0.000000000000000000, -2.173523156925980399E-06, 0.9999999999976378895 ) ) ;
#99600 = CARTESIAN_POINT ( 'NONE',  ( 1.472770742059883897, 21.73951962378590963, 11.49999999999998934 ) ) ;
#99601 = DIRECTION ( 'NONE',  ( -1.000000000000000000, -3.773278334444167608E-23, -8.201307833595939069E-29 ) ) ;
#99602 = CARTESIAN_POINT ( 'NONE',  ( -41.52287095715006160, -23.94994826722564696, -0.6494450866342750261 ) ) ;
#99603 = CARTESIAN_POINT ( 'NONE',  ( -84.52287095715006160, -24.64965694238406613, 8.947790433994198267 ) ) ;
#99604 = CARTESIAN_POINT ( 'NONE',  ( 21.72137571921558319, 1.130696696492564213, -1.500000000000002220 ) ) ;
#99605 = CARTESIAN_POINT ( 'NONE',  ( -41.58953762381673158, -24.64898659630367561, 1.056161002820379391 ) ) ;
#99607 = ORIENTED_EDGE ( 'NONE', *, *, #70209, .F. ) ;
#99606 = CARTESIAN_POINT ( 'NONE',  ( 15.82088602905085750, -15.72875506571707760, 11.49999999999999645 ) ) ;
#99608 = EDGE_CURVE ( 'NONE', #44325, #8909, #52642, .T. ) ;
#99609 = LINE ( 'NONE', #45358, #29121 ) ;
#99610 = CARTESIAN_POINT ( 'NONE',  ( -85.53959221982877636, -24.92592662359561473, 8.075495903018000021 ) ) ;
#99611 = CARTESIAN_POINT ( 'NONE',  ( -65.05438548721848235, -6.475225279485573360, 0.7300228001186309656 ) ) ;
#99612 = ORIENTED_EDGE ( 'NONE', *, *, #68946, .T. ) ;
#99613 = B_SPLINE_CURVE_WITH_KNOTS ( 'NONE', 3,
 ( #54617, #15536, #24647, #8934 ),
 .UNSPECIFIED., .F., .F.,
 ( 4, 4 ),
 ( 0.000000000000000000, 0.001096191829319139886 ),
 .UNSPECIFIED. ) ;
#99614 = VECTOR ( 'NONE', #62940, 1000.000000000000114 ) ;
#99615 = EDGE_LOOP ( 'NONE', ( #2391, #76745, #1226, #22265 ) ) ;
#99616 = EDGE_LOOP ( 'NONE', ( #16011, #32347, #2393, #50061 ) ) ;
#99617 = CARTESIAN_POINT ( 'NONE',  ( -124.5562042904834215, -24.66019654487200441, 8.947790411086121054 ) ) ;
#99618 = CARTESIAN_POINT ( 'NONE',  ( 18.56724428474754518, 10.22298014144217859, 11.49999999999998934 ) ) ;
#99619 = LINE ( 'NONE', #30120, #100022 ) ;
#99620 = CARTESIAN_POINT ( 'NONE',  ( -80.18401481691103072, -25.03138293780579460, 7.536603307588053191 ) ) ;
#99621 = CARTESIAN_POINT ( 'NONE',  ( -59.55620429048338593, -24.66019654487199730, 8.947790411086135265 ) ) ;
#99622 = DIRECTION ( 'NONE',  ( -3.773278334453080206E-23, 0.9999999999976377785, 2.173523156925979975E-06 ) ) ;
#99623 = CARTESIAN_POINT ( 'NONE',  ( -5.843762028675351772, -18.45606589188993141, 11.49999999999998934 ) ) ;
#99624 = CARTESIAN_POINT ( 'NONE',  ( 22.02124265030973760, -4.543225279485573864, 13.95402280011862395 ) ) ;
#99625 = EDGE_LOOP ( 'NONE', ( #51866, #37961, #78382, #76650 ) ) ;
#99626 = CARTESIAN_POINT ( 'NONE',  ( -14.39514105012195344, 13.04300321504834947, 11.49999999999999645 ) ) ;
#99627 = CARTESIAN_POINT ( 'NONE',  ( 22.62151214508649844, 3.754503130929783804E-15, -1.700000000000000178 ) ) ;
#99628 = ORIENTED_EDGE ( 'NONE', *, *, #417, .F. ) ;
#99629 = CARTESIAN_POINT ( 'NONE',  ( -78.52287095715006160, -23.47596703998600631, 11.44779298504228571 ) ) ;
#99630 = PLANE ( 'NONE',  #54696 ) ;
#99631 = CARTESIAN_POINT ( 'NONE',  ( -5.366453405989236813, -14.50000000000000178, 11.24599928863593767 ) ) ;
#99632 = ADVANCED_FACE ( 'NONE', ( #9365 ), #61546, .T. ) ;
#99633 = CARTESIAN_POINT ( 'NONE',  ( 6.560884470684795744, 18.50665934316380756, -1.500000000000002220 ) ) ;
#99634 = CARTESIAN_POINT ( 'NONE',  ( -41.34727404100192416, -25.27806037341403211, 4.610739018140001200 ) ) ;
#99635 = ORIENTED_EDGE ( 'NONE', *, *, #18155, .F. ) ;
#99636 = AXIS2_PLACEMENT_3D ( 'NONE', #65763, #65271, #4838 ) ;
#99637 = CARTESIAN_POINT ( 'NONE',  ( 19.30674495121141376, 9.566621930910674365, 11.49999999999998934 ) ) ;
#99638 = B_SPLINE_CURVE_WITH_KNOTS ( 'NONE', 3,
 ( #92969, #54427, #85360, #87369 ),
 .UNSPECIFIED., .F., .F.,
 ( 4, 4 ),
 ( 0.8604003152822103928, 0.8694067465543262596 ),
 .UNSPECIFIED. ) ;
#99639 = CARTESIAN_POINT ( 'NONE',  ( -33.55275594712417586, -23.96169478059712432, 10.65365249895719124 ) ) ;
#99640 = DIRECTION ( 'NONE',  ( -0.000000000000000000, 1.000000000000000000, -0.000000000000000000 ) ) ;
#99641 = DIRECTION ( 'NONE',  ( 0.000000000000000000, -0.000000000000000000, -1.000000000000000000 ) ) ;
#99642 = CARTESIAN_POINT ( 'NONE',  ( -20.21456430084473155, -11.12997698910670152, -1.500000000000002220 ) ) ;
#99643 = EDGE_CURVE ( 'NONE', #72422, #29962, #19915, .T. ) ;
#99644 = COORDINATED_UNIVERSAL_TIME_OFFSET ( 0, 0, .AHEAD. ) ;
#99645 = CARTESIAN_POINT ( 'NONE',  ( -74.55620429048340725, -23.47596703998600276, 11.44779298504227683 ) ) ;
#99646 = LINE ( 'NONE', #14919, #18315 ) ;
#99647 = CARTESIAN_POINT ( 'NONE',  ( -2.706554608146168217, 19.95013100808389339, 11.49999999999999645 ) ) ;
#99648 = CARTESIAN_POINT ( 'NONE',  ( -126.5228709571499763, -23.48783264082477018, -1.443836473390082142 ) ) ;
#99649 = DIRECTION ( 'NONE',  ( -1.000000000000000000, 0.000000000000000000, 0.000000000000000000 ) ) ;
#99650 = CARTESIAN_POINT ( 'NONE',  ( -110.3346797185884327, -25.18492896333868813, 3.293943116708551777 ) ) ;
#99651 = CARTESIAN_POINT ( 'NONE',  ( -28.62287095715004881, -29.50250786944455328, 11.44777956126000618 ) ) ;
#99652 = CARTESIAN_POINT ( 'NONE',  ( -110.3346797185884327, -25.18425582661724249, 3.293943118171629880 ) ) ;
#99653 = CARTESIAN_POINT ( 'NONE',  ( -4.768723929037996356, 19.30091236029735668, 11.49999999999998934 ) ) ;
#99654 = DIRECTION ( 'NONE',  ( 0.000000000000000000, 0.000000000000000000, 1.000000000000000000 ) ) ;
#99655 = CARTESIAN_POINT ( 'NONE',  ( 17.61170953066113398, -8.936083093766256980, -1.500000000000002220 ) ) ;
#99656 = CARTESIAN_POINT ( 'NONE',  ( -56.54793356327564169, -24.15543982623907127, -0.2315651400026670359 ) ) ;
#99657 = DESIGN_CONTEXT ( 'detailed design', #87445, 'design' ) ;
#99658 = CARTESIAN_POINT ( 'NONE',  ( -39.04530173637052570, -25.29116805862484796, 4.154356755045506056 ) ) ;
#99659 = CARTESIAN_POINT ( 'NONE',  ( -66.58953762381672448, -23.47593901973091235, -1.443836447539006196 ) ) ;
#99660 = CARTESIAN_POINT ( 'NONE',  ( -20.51892249978613236, 2.527598752449112585, 11.49999999999999645 ) ) ;
#99661 = CARTESIAN_POINT ( 'NONE',  ( -128.6228709571500417, -24.64965695001469115, 8.947790433994173398 ) ) ;
#99662 = CC_DESIGN_PERSON_AND_ORGANIZATION_ASSIGNMENT ( #21645, #74936, ( #87801 ) ) ;
#99663 = CARTESIAN_POINT ( 'NONE',  ( -35.62287095715005592, -23.47596703998600276, 11.44779298504227505 ) ) ;
#99664 = CARTESIAN_POINT ( 'NONE',  ( 20.21490908150494192, 10.32750977814155391, 11.49999999999999645 ) ) ;
#99665 = ORIENTED_EDGE ( 'NONE', *, *, #85496, .T. ) ;
#99666 = CARTESIAN_POINT ( 'NONE',  ( -60.62287095715003460, -24.52232992886363760, 0.6492154411906152500 ) ) ;
#99667 = CARTESIAN_POINT ( 'NONE',  ( -69.37510736016693613, -25.21906335291104995, 6.451581876237428403 ) ) ;
#99668 = CARTESIAN_POINT ( 'NONE',  ( 5.087728227403598424, 19.53446797131710611, -1.500000000000002220 ) ) ;
#99669 = CARTESIAN_POINT ( 'NONE',  ( -63.64183085114759564, -23.96119346886879953, -0.6495511937832106897 ) ) ;
#99670 = VECTOR ( 'NONE', #49477, 1000.000000000000000 ) ;
#99671 = CARTESIAN_POINT ( 'NONE',  ( -52.52287095715005449, -24.33927499327855770, 9.819080762295818943 ) ) ;
#99672 = EDGE_CURVE ( 'NONE', #27395, #29076, #72071, .T. ) ;
#99673 = ORIENTED_EDGE ( 'NONE', *, *, #49923, .T. ) ;
#99674 = CIRCLE ( 'NONE', #52704, 1.000000000000000000 ) ;
#99675 = VERTEX_POINT ( 'NONE', #26604 ) ;
#99676 = LINE ( 'NONE', #46413, #93863 ) ;
#99677 = CARTESIAN_POINT ( 'NONE',  ( 22.85676281555306844, 1.471244944367766649, 11.49999999999998934 ) ) ;
#99678 = CARTESIAN_POINT ( 'NONE',  ( -50.75699389676201889, -25.27420573916653623, 3.343798433542797710 ) ) ;
#99679 = CARTESIAN_POINT ( 'NONE',  ( 1.064956243273112557, 21.61254047163424019, -1.500000000000002220 ) ) ;
#99680 = CARTESIAN_POINT ( 'NONE',  ( -1.044871794871793602, -6.376774720514418959, 20.44941907051282115 ) ) ;
#99681 = DIRECTION ( 'NONE',  ( 0.000000000000000000, -0.9999999999976377785, -2.173523156925979975E-06 ) ) ;
#99682 = CARTESIAN_POINT ( 'NONE',  ( 0.8369575198195864374, -20.89415947959451003, 11.49999999999999645 ) ) ;
#99683 = VERTEX_POINT ( 'NONE', #80386 ) ;
#99684 = CARTESIAN_POINT ( 'NONE',  ( -68.94292010565295925, -25.31612680529077508, 6.048223976952783687 ) ) ;
#99685 = CARTESIAN_POINT ( 'NONE',  ( -6.199593828526920092, 21.14725108817225419, -1.500000000000002220 ) ) ;
#99686 = CARTESIAN_POINT ( 'NONE',  ( -105.5930580087945145, -24.15602025860896163, 10.28564288303535967 ) ) ;
#99687 = CARTESIAN_POINT ( 'NONE',  ( -28.57615893954310238, -24.79700241673980088, 7.256892281947859402 ) ) ;
#99688 = ORIENTED_EDGE ( 'NONE', *, *, #58068, .T. ) ;
#99689 = CARTESIAN_POINT ( 'NONE',  ( 4.115763745420833786, -6.376774720514402972, 18.20859014712428348 ) ) ;
#99690 = CARTESIAN_POINT ( 'NONE',  ( -90.54141365085332893, -24.92592662359561118, 8.075495903017998245 ) ) ;
#99691 = ORIENTED_EDGE ( 'NONE', *, *, #98026, .T. ) ;
#99692 = PLANE ( 'NONE',  #85771 ) ;
#99693 = ORIENTED_EDGE ( 'NONE', *, *, #62081, .F. ) ;
#99694 = EDGE_LOOP ( 'NONE', ( #95106, #64935, #64611, #30360 ) ) ;
#99695 = ADVANCED_FACE ( 'NONE', ( #49957 ), #41842, .T. ) ;
#99696 = CARTESIAN_POINT ( 'NONE',  ( -71.51121550292000961, -23.96169478059713498, 10.65365249895718058 ) ) ;
#99697 = DIRECTION ( 'NONE',  ( 0.000000000000000000, 0.000000000000000000, -1.000000000000000000 ) ) ;
#99698 = CARTESIAN_POINT ( 'NONE',  ( -36.49045368110912335, -24.34968618360933235, 0.1864209137778783110 ) ) ;
#99699 = CARTESIAN_POINT ( 'NONE',  ( 19.18951349294833264, 7.196795126939715459, -1.500000000000002220 ) ) ;
#99700 = ORIENTED_EDGE ( 'NONE', *, *, #84459, .F. ) ;
#99701 = CARTESIAN_POINT ( 'NONE',  ( -3.108425644221024520, -6.376774720514415407, 20.25188360057253334 ) ) ;
#99702 = CARTESIAN_POINT ( 'NONE',  ( -30.60993385648455956, -24.45056191361606679, 9.787827635114014768 ) ) ;
#99703 = CARTESIAN_POINT ( 'NONE',  ( -89.81226385320383088, -25.22391155068715207, 6.409327647370969494 ) ) ;
#99704 = CARTESIAN_POINT ( 'NONE',  ( 20.70802603420765564, 8.137917507125113303, -1.500000000000002220 ) ) ;
#99705 = DIRECTION ( 'NONE',  ( 0.000000000000000000, -1.000000000000000000, 0.000000000000000000 ) ) ;
#99706 = CARTESIAN_POINT ( 'NONE',  ( -8.035485827249791768, 10.29661271514167709, -0.9008368852918171577 ) ) ;
#99707 = ORIENTED_EDGE ( 'NONE', *, *, #15754, .T. ) ;
#99708 = CARTESIAN_POINT ( 'NONE',  ( -8.160000000000000142, 7.891155995661686795, 5.788828319098143993 ) ) ;
#99709 = CARTESIAN_POINT ( 'NONE',  ( -64.58953762381672448, -23.48786465467241413, 11.44779295918254824 ) ) ;
#99710 = AXIS2_PLACEMENT_3D ( 'NONE', #58643, #43428, #9592 ) ;
#99711 = EDGE_CURVE ( 'NONE', #46308, #47247, #1784, .T. ) ;
#99712 = CARTESIAN_POINT ( 'NONE',  ( 5.171613189315443115, 20.13430294385436881, 11.49999999999998934 ) ) ;
#99713 = EDGE_CURVE ( 'NONE', #66710, #28190, #87664, .T. ) ;
#99714 = ORIENTED_EDGE ( 'NONE', *, *, #6286, .T. ) ;
#99716 = ORIENTED_EDGE ( 'NONE', *, *, #12202, .F. ) ;
#99715 = CARTESIAN_POINT ( 'NONE',  ( 26.73860345374794534, 1.682774720514426114, -1.352392034746782823 ) ) ;
#99717 = B_SPLINE_CURVE_WITH_KNOTS ( 'NONE', 3,
 ( #7872, #84994, #79379, #15478 ),
 .UNSPECIFIED., .F., .F.,
 ( 4, 4 ),
 ( 0.000000000000000000, 0.0001000000000000028644 ),
 .UNSPECIFIED. ) ;
#99718 = CARTESIAN_POINT ( 'NONE',  ( -98.52287095715010423, -24.35013146730204525, 9.818937971375097717 ) ) ;
#99719 = ORIENTED_EDGE ( 'NONE', *, *, #70155, .T. ) ;
#99720 = EDGE_LOOP ( 'NONE', ( #84491, #40366 ) ) ;
#99721 = FACE_OUTER_BOUND ( 'NONE', #97617, .T. ) ;
#99722 = CARTESIAN_POINT ( 'NONE',  ( 6.660000000000001030, 0.000000000000000000, 0.000000000000000000 ) ) ;
#99723 =( REPRESENTATION_RELATIONSHIP ('NONE','NONE', #96270, #22430 ) REPRESENTATION_RELATIONSHIP_WITH_TRANSFORMATION ( #45036 )SHAPE_REPRESENTATION_RELATIONSHIP( ) );
#99724 = DIRECTION ( 'NONE',  ( 0.000000000000000000, 0.000000000000000000, 1.000000000000000000 ) ) ;
#99725 = CARTESIAN_POINT ( 'NONE',  ( -40.62287095715005592, -23.48786465467240347, 11.44779295918255180 ) ) ;
#99726 = CARTESIAN_POINT ( 'NONE',  ( -109.0201204086170037, -25.24933767340982271, 3.731844282071034691 ) ) ;
#99727 = CARTESIAN_POINT ( 'NONE',  ( 26.37445894957760473, -2.682774720514426559, -11.69480419648520986 ) ) ;
#99729 = EDGE_LOOP ( 'NONE', ( #90123, #74752, #88554, #14633 ) ) ;
#99728 = CARTESIAN_POINT ( 'NONE',  ( -0.9539927174334467130, 22.11892580961223587, 11.49999999999999645 ) ) ;
#99730 = ADVANCED_FACE ( 'NONE', ( #79376 ), #19474, .F. ) ;
#99731 = CARTESIAN_POINT ( 'NONE',  ( -11.16000000000000014, -10.15233964170348457, 0.003711184059992174607 ) ) ;
#99732 = CARTESIAN_POINT ( 'NONE',  ( 10.43192878459595185, 20.09917060401269850, -1.500000000000002220 ) ) ;
#99734 = ORIENTED_EDGE ( 'NONE', *, *, #20535, .T. ) ;
#99733 = CARTESIAN_POINT ( 'NONE',  ( -29.18816247444169676, -25.16187336171572397, 5.952578768344731763 ) ) ;
#99735 = ORIENTED_EDGE ( 'NONE', *, *, #70466, .T. ) ;
#99736 = CARTESIAN_POINT ( 'NONE',  ( 5.550000000000006040, -14.50000000000000178, 24.00000000000000000 ) ) ;
#99737 = VECTOR ( 'NONE', #26347, 1000.000000000000000 ) ;
#99738 = CARTESIAN_POINT ( 'NONE',  ( 9.271505649751263789, 17.87650053469100087, -1.500000000000002220 ) ) ;
#99739 = CARTESIAN_POINT ( 'NONE',  ( -88.52287095715009002, -23.48783264082477018, -1.443836473390089692 ) ) ;
#99740 = ORIENTED_EDGE ( 'NONE', *, *, #61418, .F. ) ;
#99741 = CARTESIAN_POINT ( 'NONE',  ( 15.99960863614631101, -3.577630190450212577, -27.91116951066581819 ) ) ;
#99742 = CARTESIAN_POINT ( 'NONE',  ( -7.140196579304709523, 21.16591527347414115, -1.500000000000002220 ) ) ;
#99743 = AXIS2_PLACEMENT_3D ( 'NONE', #59470, #67100, #98005 ) ;
#99744 = VECTOR ( 'NONE', #23001, 1000.000000000000114 ) ;
#99745 = ORIENTED_EDGE ( 'NONE', *, *, #34686, .F. ) ;
#99746 = ORIENTED_EDGE ( 'NONE', *, *, #12661, .F. ) ;
#99747 = FACE_OUTER_BOUND ( 'NONE', #93408, .T. ) ;
#99748 = FACE_OUTER_BOUND ( 'NONE', #84614, .T. ) ;
#99749 = CARTESIAN_POINT ( 'NONE',  ( -80.71555671556204459, -25.29701806042628576, 4.545855233347295687 ) ) ;
#99750 = CARTESIAN_POINT ( 'NONE',  ( -57.58953762381671027, -24.64965694238406968, 8.947790433994660120 ) ) ;
#99751 = CIRCLE ( 'NONE', #21962, 7.652410033082760243 ) ;
#99752 = LINE ( 'NONE', #51617, #37437 ) ;
#99753 = CARTESIAN_POINT ( 'NONE',  ( 19.50827032651345405, -1.201405007418623994, 11.49999999999998934 ) ) ;
#99754 = LINE ( 'NONE', #42651, #13342 ) ;
#99755 = CARTESIAN_POINT ( 'NONE',  ( -4.253298834618286506, 21.06115358058179154, -1.500000000000002220 ) ) ;
#99756 = CARTESIAN_POINT ( 'NONE',  ( -2.220741593810419801, -5.876774720514410077, 19.46247113826587238 ) ) ;
#99757 = DIRECTION ( 'NONE',  ( 0.000000000000000000, 0.000000000000000000, -1.000000000000000000 ) ) ;
#99758 = CARTESIAN_POINT ( 'NONE',  ( -129.5228709571500758, -23.73934037231757443, 11.05740245334327732 ) ) ;
#99759 = CARTESIAN_POINT ( 'NONE',  ( -18.82434810282327220, -12.99595988342530362, -1.500000000000002220 ) ) ;
#99760 = EDGE_CURVE ( 'NONE', #2589, #64840, #71782, .T. ) ;
#99761 = APPROVAL_ROLE ( '' ) ;
#99762 = CARTESIAN_POINT ( 'NONE',  ( -96.63278406345585836, -23.96169478059713498, 10.65365249895717881 ) ) ;
#99763 = CARTESIAN_POINT ( 'NONE',  ( -125.6228709571500275, -23.48783264082479505, -1.443836473390057273 ) ) ;
#99764 = CARTESIAN_POINT ( 'NONE',  ( 18.23660095519748481, -8.086948576924280374, 11.49999999999999645 ) ) ;
#99765 = DIRECTION ( 'NONE',  ( 0.000000000000000000, 0.000000000000000000, 1.000000000000000000 ) ) ;
#99766 = CARTESIAN_POINT ( 'NONE',  ( -74.56445734505570044, -23.48786465467241058, 11.44779295918254824 ) ) ;
#99767 = CYLINDRICAL_SURFACE ( 'NONE', #92612, 1.500000000000000666 ) ;
#99768 = ORIENTED_EDGE ( 'NONE', *, *, #91640, .F. ) ;
#99769 = PLANE ( 'NONE',  #81775 ) ;
#99770 = FACE_OUTER_BOUND ( 'NONE', #47683, .T. ) ;
#99771 = CARTESIAN_POINT ( 'NONE',  ( -19.66401359581072583, -9.230316601043258018, -1.500000000000002220 ) ) ;
#99772 = FACE_OUTER_BOUND ( 'NONE', #56296, .T. ) ;
#99773 = CARTESIAN_POINT ( 'NONE',  ( -14.26233628608129855, 13.40890954296891024, -1.500000000000002220 ) ) ;
#99774 = CARTESIAN_POINT ( 'NONE',  ( -34.52287095715008292, -24.51283580621449687, 0.6167428607045372102 ) ) ;
#99775 = CARTESIAN_POINT ( 'NONE',  ( -121.6228709571500417, -29.50248528299804818, 1.056150453629045360 ) ) ;
#99776 = DATE_TIME_ROLE ( 'classification_date' ) ;
#99777 = CARTESIAN_POINT ( 'NONE',  ( -91.63754774048484819, -23.73791477778911840, 11.05961554403170410 ) ) ;
#99778 = CARTESIAN_POINT ( 'NONE',  ( 2.880689065218799083, -5.876774720514426065, 21.31732089891691828 ) ) ;
#99779 = CARTESIAN_POINT ( 'NONE',  ( 6.429960413904108663, -19.47341730443774921, 11.49999999999999645 ) ) ;
#99780 = CARTESIAN_POINT ( 'NONE',  ( -94.52287095715007581, -23.47593901973090524, -1.443836447538996648 ) ) ;
#99781 = CARTESIAN_POINT ( 'NONE',  ( 13.91401389203221406, -5.965225279485572685, 158.0376437107427137 ) ) ;
#99782 = EDGE_CURVE ( 'NONE', #78754, #14881, #45473, .T. ) ;
#99783 = B_SPLINE_CURVE_WITH_KNOTS ( 'NONE', 3,
 ( #16412, #63624, #2716, #9813 ),
 .UNSPECIFIED., .F., .F.,
 ( 4, 4 ),
 ( 0.000000000000000000, 9.999999999998900014E-05 ),
 .UNSPECIFIED. ) ;
#99784 = EDGE_LOOP ( 'NONE', ( #54157, #62672, #24809, #88900 ) ) ;
#99785 = CARTESIAN_POINT ( 'NONE',  ( -109.3647183699074077, -25.28795728176566726, 4.344563986793225752 ) ) ;
#99786 = CARTESIAN_POINT ( 'NONE',  ( -40.35585260198725877, -25.18430871971380469, 3.296897012306942987 ) ) ;
#99787 = CARTESIAN_POINT ( 'NONE',  ( -125.5909824311810468, -23.85049219812686516, 10.88485053497526778 ) ) ;
#99788 = PLANE ( 'NONE',  #32095 ) ;
#99789 = EDGE_CURVE ( 'NONE', #30682, #34154, #11865, .T. ) ;
#99790 = CARTESIAN_POINT ( 'NONE',  ( -85.52287095715006160, -24.92579138211019085, 1.929029949965661794 ) ) ;
#99791 = CARTESIAN_POINT ( 'NONE',  ( -42.62287095715004881, -24.64965695001467694, 8.947790433994187609 ) ) ;
#99792 = ADVANCED_FACE ( 'NONE', ( #96115 ), #50438, .T. ) ;
#99793 = EDGE_CURVE ( 'NONE', #84765, #98477, #32705, .T. ) ;
#99794 = VECTOR ( 'NONE', #78124, 1000.000000000000000 ) ;
#99795 = CARTESIAN_POINT ( 'NONE',  ( 18.43541038833219758, -13.85303862407246811, 11.49999999999999645 ) ) ;
#99796 = CARTESIAN_POINT ( 'NONE',  ( -12.44792101662413408, -19.12764231104124946, -1.500000000000002220 ) ) ;
#99797 = CARTESIAN_POINT ( 'NONE',  ( -125.5228709571500616, -25.00158670708909980, 2.256160236439166411 ) ) ;
#99798 = CARTESIAN_POINT ( 'NONE',  ( -75.52287095715006160, -24.99156044556120548, 7.747789690856173195 ) ) ;
#99799 = CARTESIAN_POINT ( 'NONE',  ( -86.52287095715007581, -24.50321055353806088, 9.387540953477524042 ) ) ;
#99800 = EDGE_CURVE ( 'NONE', #2671, #44074, #75617, .T. ) ;
#99801 = CARTESIAN_POINT ( 'NONE',  ( -42.52287095715005449, -23.47596703998600631, 11.44779298504229281 ) ) ;
#99802 = CARTESIAN_POINT ( 'NONE',  ( -110.5871110012158454, -24.83618233451450763, 1.606449574219537935 ) ) ;
#99803 = CARTESIAN_POINT ( 'NONE',  ( 18.32745805453730981, -11.99952526121574259, -1.500000000000002220 ) ) ;
#99804 = CARTESIAN_POINT ( 'NONE',  ( -5.755030174389611730, -6.376774720514411854, 19.56655654527324728 ) ) ;
#99805 = CIRCLE ( 'NONE', #47985, 3.060000000000000053 ) ;
#99806 = LINE ( 'NONE', #30313, #20360 ) ;
#99807 = CARTESIAN_POINT ( 'NONE',  ( -77.62287095715007013, -23.48783264082478794, -1.443836473390065933 ) ) ;
#99808 = CARTESIAN_POINT ( 'NONE',  ( -78.58812948176218072, -24.34968618360933945, 0.1864209137778830849 ) ) ;
#99809 = CARTESIAN_POINT ( 'NONE',  ( -88.62287095715004170, -29.50248528299804818, 1.056150453629040253 ) ) ;
#99810 = EDGE_LOOP ( 'NONE', ( #9878, #73064, #33344, #55339, #76120 ) ) ;
#99811 = VECTOR ( 'NONE', #3041, 1000.000000000000000 ) ;
#99812 = CARTESIAN_POINT ( 'NONE',  ( 14.46511082492616573, -14.46070965572739730, -1.500000000000002220 ) ) ;
#99813 = ORIENTED_EDGE ( 'NONE', *, *, #55909, .F. ) ;
#99814 = AXIS2_PLACEMENT_3D ( 'NONE', #84809, #30020, #83308 ) ;
#99815 = EDGE_LOOP ( 'NONE', ( #53868, #3479, #70396, #38547 ) ) ;
#99816 = VERTEX_POINT ( 'NONE', #34219 ) ;
#99817 = ORIENTED_EDGE ( 'NONE', *, *, #84728, .T. ) ;
#99818 = EDGE_CURVE ( 'NONE', #50118, #96754, #27099, .T. ) ;
#99819 = CARTESIAN_POINT ( 'NONE',  ( -22.63574357292403860, -4.499050354539342322, 11.49999999999998934 ) ) ;
#99820 = CARTESIAN_POINT ( 'NONE',  ( 7.160000000000000142, 3.920813812768718080E-16, 6.788828319098143105 ) ) ;
#99821 = CARTESIAN_POINT ( 'NONE',  ( 18.82434097252966154, -7.598309640217090433, -1.500000000000002220 ) ) ;
#99822 = AXIS2_PLACEMENT_3D ( 'NONE', #51870, #17295, #567 ) ;
#99823 = ORIENTED_EDGE ( 'NONE', *, *, #93055, .T. ) ;
#99824 = CARTESIAN_POINT ( 'NONE',  ( -26.09015812629794695, -24.66927170924689960, 7.636915180611342002 ) ) ;
#99825 = CARTESIAN_POINT ( 'NONE',  ( -41.80358701677449318, -25.31074848354002782, 4.649732148862797843 ) ) ;
#99826 = VECTOR ( 'NONE', #79481, 1000.000000000000000 ) ;
#99827 = CARTESIAN_POINT ( 'NONE',  ( -31.62287095715005236, -29.50247984919015209, -1.443849546365062242 ) ) ;
#99828 = CARTESIAN_POINT ( 'NONE',  ( -99.51175462723297471, -24.35071581493543746, 9.817618358456025263 ) ) ;
#99830 = ORIENTED_EDGE ( 'NONE', *, *, #26757, .F. ) ;
#99829 = CARTESIAN_POINT ( 'NONE',  ( -4.378498130703003532, 20.98420022172975763, 11.49999999999999645 ) ) ;
#99831 = CARTESIAN_POINT ( 'NONE',  ( -126.6228709571500559, -24.64898659630529565, 1.056161002820834804 ) ) ;
#99832 = CARTESIAN_POINT ( 'NONE',  ( -61.50411378425246767, -24.15620529776627734, 10.23563542870660825 ) ) ;
#99833 = VERTEX_POINT ( 'NONE', #90490 ) ;
#99834 = B_SPLINE_CURVE_WITH_KNOTS ( 'NONE', 3,
 ( #79855, #94078, #56547, #55540 ),
 .UNSPECIFIED., .F., .F.,
 ( 4, 4 ),
 ( 0.000000000000000000, 1.000000000000000000 ),
 .UNSPECIFIED. ) ;
#99835 = CARTESIAN_POINT ( 'NONE',  ( -13.38394104848841693, -15.81244124602197765, -1.500000000000002220 ) ) ;
#99836 = ADVANCED_FACE ( 'NONE', ( #83366 ), #97599, .F. ) ;
#99837 = ORIENTED_EDGE ( 'NONE', *, *, #93052, .T. ) ;
#99839 = ORIENTED_EDGE ( 'NONE', *, *, #90655, .T. ) ;
#99838 = DIRECTION ( 'NONE',  ( 0.000000000000000000, -1.000000000000000000, 0.000000000000000000 ) ) ;
#99840 = EDGE_CURVE ( 'NONE', #57944, #86101, #27605, .T. ) ;
#99841 = CARTESIAN_POINT ( 'NONE',  ( -84.62287095715004170, -24.65952944569304606, 1.056160979905699460 ) ) ;
#99842 = EDGE_LOOP ( 'NONE', ( #45600, #33177, #93524, #666 ) ) ;
#99843 = CARTESIAN_POINT ( 'NONE',  ( -55.52287095715006870, -24.82576562948882071, 8.398263436605676091 ) ) ;
#99844 = CARTESIAN_POINT ( 'NONE',  ( -65.53039227110043896, -25.00158670708910691, 2.256160236439222366 ) ) ;
#99845 = CARTESIAN_POINT ( 'NONE',  ( -21.51515180086577317, 4.489188270810763548, 11.49999999999999645 ) ) ;
#99846 = EDGE_CURVE ( 'NONE', #420, #84514, #61098, .T. ) ;
#99847 = LINE ( 'NONE', #61328, #28488 ) ;
#99848 = CARTESIAN_POINT ( 'NONE',  ( 21.16815136333514502, -7.790938087775149512, -1.500000000000002220 ) ) ;
#99849 = VECTOR ( 'NONE', #45876, 1000.000000000000000 ) ;
#99850 = B_SPLINE_CURVE_WITH_KNOTS ( 'NONE', 3,
 ( #82875, #59565, #5261, #91485 ),
 .UNSPECIFIED., .F., .F.,
 ( 4, 4 ),
 ( 6.938893903907228378E-18, 9.999999999999591193E-05 ),
 .UNSPECIFIED. ) ;
#99851 = CARTESIAN_POINT ( 'NONE',  ( -3.838044578953509145, 20.63102806057878880, 11.49999999999998934 ) ) ;
#99852 = EDGE_CURVE ( 'NONE', #22614, #17829, #84381, .T. ) ;
#99853 = DIRECTION ( 'NONE',  ( 0.9762960071199348056, 0.2164396139380966033, -0.000000000000000000 ) ) ;
#99854 = CARTESIAN_POINT ( 'NONE',  ( 6.110660513271839456, -6.376774720514422512, 21.43053473047838509 ) ) ;
#99855 = VERTEX_POINT ( 'NONE', #20466 ) ;
#99856 = ADVANCED_FACE ( 'NONE', ( #58554 ), #91476, .F. ) ;
#99857 = EDGE_LOOP ( 'NONE', ( #22620, #20233, #23110, #68072 ) ) ;
#99858 = EDGE_LOOP ( 'NONE', ( #62806, #74770, #58534, #15098 ) ) ;
#99859 = DIRECTION ( 'NONE',  ( 1.000000000000000000, 4.986391167143583514E-16, 0.000000000000000000 ) ) ;
#99860 = CARTESIAN_POINT ( 'NONE',  ( -0.7226137440361984909, -21.50112622129444162, -1.500000000000002220 ) ) ;
#99861 = CARTESIAN_POINT ( 'NONE',  ( -105.5228709571500616, -24.99156044556202971, 7.747789690856173195 ) ) ;
#99862 = VERTEX_POINT ( 'NONE', #28589 ) ;
#99863 = CARTESIAN_POINT ( 'NONE',  ( -13.19772682967519195, -16.48504770976277101, 11.49999999999998934 ) ) ;
#99864 = CARTESIAN_POINT ( 'NONE',  ( 10.75273025779354263, -5.876774720514426953, 16.96478738960562893 ) ) ;
#99865 = CARTESIAN_POINT ( 'NONE',  ( 7.089543269230769162, -5.876774720514413630, 19.75741185897435415 ) ) ;
#99866 = FACE_OUTER_BOUND ( 'NONE', #92737, .T. ) ;
#99867 = CARTESIAN_POINT ( 'NONE',  ( -118.5228709571500758, -23.47593901973090524, -1.443836447538996204 ) ) ;
#99868 = CARTESIAN_POINT ( 'NONE',  ( -70.34217863391401693, -25.30972802343782035, 4.286149581475303449 ) ) ;
#99869 = CARTESIAN_POINT ( 'NONE',  ( 0.7503028313155074569, 22.12739137992853955, -1.500000000000002220 ) ) ;
#99870 = CARTESIAN_POINT ( 'NONE',  ( -71.65049672173245199, -23.48783264082476663, -1.443836473390092578 ) ) ;
#99871 = VERTEX_POINT ( 'NONE', #81881 ) ;
#99872 = CARTESIAN_POINT ( 'NONE',  ( -51.52812418322009336, -25.24860062847332287, 5.264378554598589943 ) ) ;
#99873 = CARTESIAN_POINT ( 'NONE',  ( -67.55620429048339304, -24.64898659630528854, 1.056161002820824368 ) ) ;
#99874 = CARTESIAN_POINT ( 'NONE',  ( -43.62287095715003460, -24.51283580621364777, 0.6167428607019733722 ) ) ;
#99875 = VECTOR ( 'NONE', #64253, 1000.000000000000227 ) ;
#99876 = CARTESIAN_POINT ( 'NONE',  ( -41.86667701670297248, -25.27373279006357265, 4.118129000631158831 ) ) ;
#99877 = CARTESIAN_POINT ( 'NONE',  ( 17.17441491540288823, 9.109037055621362455, -1.500000000000002220 ) ) ;
#99878 = CARTESIAN_POINT ( 'NONE',  ( -19.99122433398336440, 7.574256484821010105, 11.49999999999998934 ) ) ;
#99879 = CARTESIAN_POINT ( 'NONE',  ( -62.64801611461953712, -23.73766607897669445, -1.055555164236454901 ) ) ;
#99880 = CARTESIAN_POINT ( 'NONE',  ( 0.3910256410256394144, -5.876774720514412742, 19.63681891025641235 ) ) ;
#99881 = CARTESIAN_POINT ( 'NONE',  ( -72.52287095715007581, -24.64965694238575011, 8.947790433994200043 ) ) ;
#99882 = CARTESIAN_POINT ( 'NONE',  ( -128.6228709571500417, -23.47593901973091235, -1.443836447538995760 ) ) ;
#99883 = CARTESIAN_POINT ( 'NONE',  ( -22.46375958613465684, 3.124547546656453179, -1.500000000000002220 ) ) ;
#99884 = VECTOR ( 'NONE', #3099, 1000.000000000000114 ) ;
#99885 = AXIS2_PLACEMENT_3D ( 'NONE', #21101, #14488, #60690 ) ;
#99886 = FACE_OUTER_BOUND ( 'NONE', #53931, .T. ) ;
#99887 = CARTESIAN_POINT ( 'NONE',  ( -62.62287095715004881, -23.48786465467241058, 11.44779295918254824 ) ) ;
#99888 = CARTESIAN_POINT ( 'NONE',  ( -6.431973572030615038, 18.70533856667250916, 11.49999999999999645 ) ) ;
#99889 = VECTOR ( 'NONE', #16983, 1000.000000000000114 ) ;
#99890 = CYLINDRICAL_SURFACE ( 'NONE', #33425, 21.24999999999998579 ) ;
#99891 = ORIENTED_EDGE ( 'NONE', *, *, #51604, .F. ) ;
#99892 = FACE_OUTER_BOUND ( 'NONE', #53591, .T. ) ;
#99893 = LINE ( 'NONE', #84688, #65865 ) ;
#99894 = CARTESIAN_POINT ( 'NONE',  ( 13.31326451270642330, 17.06472021985377552, -1.500000000000002220 ) ) ;
#99895 = CARTESIAN_POINT ( 'NONE',  ( -66.52287095715006160, -24.65952944569304606, 1.056160979905697239 ) ) ;
#99897 = AXIS2_PLACEMENT_3D ( 'NONE', #4482, #88713, #20182 ) ;
#99896 = CARTESIAN_POINT ( 'NONE',  ( 18.80106323769845389, 4.952424739525837616, -1.500000000000002220 ) ) ;
#99898 = CARTESIAN_POINT ( 'NONE',  ( -80.52287095715001897, -24.63345952396254646, 9.038047939301504741 ) ) ;
#99899 = CARTESIAN_POINT ( 'NONE',  ( -129.5228709571500758, -24.64965694238408034, 8.947790433994189385 ) ) ;
#99900 = CARTESIAN_POINT ( 'NONE',  ( 0.4224338394261131779, -19.80333402765648998, 11.49999999999998934 ) ) ;
#99901 = ORIENTED_EDGE ( 'NONE', *, *, #94325, .F. ) ;
#99902 = CARTESIAN_POINT ( 'NONE',  ( -5.305567426876419468, 19.62801697144059787, 11.49999999999999645 ) ) ;
#99903 = PLANE ( 'NONE',  #71581 ) ;
#99904 = CARTESIAN_POINT ( 'NONE',  ( 33.55975867735808293, -4.270419025147598191, -12.32584534477734728 ) ) ;
#99905 = EDGE_CURVE ( 'NONE', #14044, #28727, #15069, .T. ) ;
#99906 = ORIENTED_EDGE ( 'NONE', *, *, #65627, .F. ) ;
#99907 = CARTESIAN_POINT ( 'NONE',  ( -30.59326697242301663, -24.88273649812090582, 8.549170486301877148 ) ) ;
#99908 = PLANE ( 'NONE',  #25007 ) ;
#99909 = CARTESIAN_POINT ( 'NONE',  ( 22.81105451610979173, 6.475225279485573360, -19.61691820600746539 ) ) ;
#99910 = CARTESIAN_POINT ( 'NONE',  ( -40.60173077338293268, -24.15602025860895097, 10.28564288303536856 ) ) ;
#99911 = DIRECTION ( 'NONE',  ( -3.773278334444166432E-23, 1.000000000000000000, 0.000000000000000000 ) ) ;
#99912 = CARTESIAN_POINT ( 'NONE',  ( -20.04763853020464737, 0.9818187932333496404, -1.500000000000002220 ) ) ;
#99913 = CARTESIAN_POINT ( 'NONE',  ( -1.675486951385420475, 10.82748519320431591, 0.000000000000000000 ) ) ;
#99914 = ORIENTED_EDGE ( 'NONE', *, *, #49725, .T. ) ;
#99915 = ADVANCED_FACE ( 'NONE', ( #82375 ), #12848, .T. ) ;
#99916 = CARTESIAN_POINT ( 'NONE',  ( -24.55517127435777169, -5.965225279485592225, -15.44180958690142802 ) ) ;
#99917 = CIRCLE ( 'NONE', #18889, 1.529999999999999805 ) ;
#99918 = EDGE_CURVE ( 'NONE', #73552, #53085, #86606, .T. ) ;
#99919 = ADVANCED_FACE ( 'NONE', ( #30078 ), #51772, .T. ) ;
#99920 = CARTESIAN_POINT ( 'NONE',  ( -17.76840699843883442, -14.40508365592194195, 11.49999999999999645 ) ) ;
#99921 = CARTESIAN_POINT ( 'NONE',  ( -22.42851769774927817, -3.676000928666301792, 11.49999999999998934 ) ) ;
#99922 = CARTESIAN_POINT ( 'NONE',  ( -30.47287095715008221, -24.47801986434321719, 0.5914027130429533319 ) ) ;
#99923 = CARTESIAN_POINT ( 'NONE',  ( 0.4325450954222598288, 0.000000000000000000, 0.000000000000000000 ) ) ;
#99924 = CARTESIAN_POINT ( 'NONE',  ( -38.55292283764729433, -23.96169478059712432, 10.65365249895718591 ) ) ;
#99925 = ADVANCED_FACE ( 'NONE', ( #15848 ), #23446, .F. ) ;
#99926 = CIRCLE ( 'NONE', #86973, 2.249999999999998668 ) ;
#99927 = CARTESIAN_POINT ( 'NONE',  ( 5.696197030082937651, -5.876774720514422512, 21.05387829558662816 ) ) ;
#99928 = B_SPLINE_CURVE_WITH_KNOTS ( 'NONE', 3,
 ( #33094, #79760, #2162, #18369, #41216, #95493, #10255, #72168 ),
 .UNSPECIFIED., .F., .F.,
 ( 4, 2, 2, 4 ),
 ( 6.391158118962919560E-06, 0.002007136338688543433, 0.003007508928973333037, 0.004007881519258123075 ),
 .UNSPECIFIED. ) ;
#99929 = CARTESIAN_POINT ( 'NONE',  ( 6.431189903846153300, -5.876774720514424288, 20.08974358974358765 ) ) ;
#99930 = CARTESIAN_POINT ( 'NONE',  ( -96.62287095715005592, -24.66019654487199730, 8.947790411086124607 ) ) ;
#99931 = ORIENTED_EDGE ( 'NONE', *, *, #45777, .F. ) ;
#99932 = CARTESIAN_POINT ( 'NONE',  ( 19.36038471569032993, -6.267470172042458820, -1.500000000000002220 ) ) ;
#99933 = ORIENTED_EDGE ( 'NONE', *, *, #99278, .T. ) ;
#99934 = EDGE_CURVE ( 'NONE', #80888, #41589, #22944, .T. ) ;
#99935 = CARTESIAN_POINT ( 'NONE',  ( -7.281717392095591102, 21.80608952751712692, 11.49999999999998934 ) ) ;
#99936 = DIRECTION ( 'NONE',  ( 0.000000000000000000, -1.000000000000000000, 0.000000000000000000 ) ) ;
#99937 = ORIENTED_EDGE ( 'NONE', *, *, #84588, .T. ) ;
#99938 = CARTESIAN_POINT ( 'NONE',  ( -101.5115365805468031, -25.23057817895866961, 6.352079517346162163 ) ) ;
#99939 = AXIS2_PLACEMENT_3D ( 'NONE', #9160, #69061, #16273 ) ;
#99940 = FACE_OUTER_BOUND ( 'NONE', #74686, .T. ) ;
#99941 = EDGE_CURVE ( 'NONE', #91196, #41110, #17597, .T. ) ;
#99942 = CARTESIAN_POINT ( 'NONE',  ( -51.65968679752383252, -23.48786465467241413, 11.44779295918254824 ) ) ;
#99944 = EDGE_LOOP ( 'NONE', ( #21754, #17888, #53930, #69636, #7582 ) ) ;
#99943 = CARTESIAN_POINT ( 'NONE',  ( 1.624102159173431259, 21.17561035156254334, 11.49999999999999645 ) ) ;
#99945 = ORIENTED_EDGE ( 'NONE', *, *, #66075, .T. ) ;
#99946 = CARTESIAN_POINT ( 'NONE',  ( 0.7529269182969693386, -22.20201975079678647, -1.500000000000002220 ) ) ;
#99947 = CARTESIAN_POINT ( 'NONE',  ( -11.82494684808912844, 16.90534455221803967, -1.500000000000002220 ) ) ;
#99948 = EDGE_CURVE ( 'NONE', #98585, #12105, #69144, .T. ) ;
#99949 = AXIS2_PLACEMENT_3D ( 'NONE', #36322, #28709, #37324 ) ;
#99950 = EDGE_LOOP ( 'NONE', ( #54911, #17019, #6251, #41724, #12793, #78919, #82253, #63812, #14070, #5867, #43327, #60231 ) ) ;
#99951 = VERTEX_POINT ( 'NONE', #100066 ) ;
#99952 = CARTESIAN_POINT ( 'NONE',  ( -109.1250679552890830, -25.31627268072813663, 4.858945138523542262 ) ) ;
#99953 = CARTESIAN_POINT ( 'NONE',  ( -39.38163181517934675, -25.19537108852798468, 3.295112504627180972 ) ) ;
#99954 = VERTEX_POINT ( 'NONE', #62045 ) ;
#99955 = AXIS2_PLACEMENT_3D ( 'NONE', #35724, #66697, #97608 ) ;
#99956 = CARTESIAN_POINT ( 'NONE',  ( -50.06116249559564579, -25.13922480169752660, 7.066689096949080096 ) ) ;
#99957 = AXIS2_PLACEMENT_3D ( 'NONE', #86397, #8274, #23472 ) ;
#99958 = ORIENTED_EDGE ( 'NONE', *, *, #3401, .T. ) ;
#99959 = CARTESIAN_POINT ( 'NONE',  ( -80.88924702628075636, -25.29868576439400840, 4.592921234843194256 ) ) ;
#99960 = CARTESIAN_POINT ( 'NONE',  ( -35.52287095715006870, -23.48786465467240347, 11.44779295918255180 ) ) ;
#99961 = CARTESIAN_POINT ( 'NONE',  ( 10.19739565540945492, -18.13666118385682680, -1.500000000000002220 ) ) ;
#99962 = CARTESIAN_POINT ( 'NONE',  ( -17.16505717403991227, -13.39166244882208012, 11.49999999999999645 ) ) ;
#99963 = CARTESIAN_POINT ( 'NONE',  ( -52.62287095715004881, -24.33832256526968507, 0.1851278514119848728 ) ) ;
#99964 = CARTESIAN_POINT ( 'NONE',  ( -99.22161667368584403, -25.13713020721655411, 7.020935302435689529 ) ) ;
#99965 = CARTESIAN_POINT ( 'NONE',  ( -8.346146134265904237, -20.86121191590761015, 11.49999999999998934 ) ) ;
#99966 = EDGE_CURVE ( 'NONE', #89557, #63566, #24415, .T. ) ;
#99967 = LINE ( 'NONE', #98476, #15770 ) ;
#99968 = ORIENTED_EDGE ( 'NONE', *, *, #89655, .F. ) ;
#99969 = DIRECTION ( 'NONE',  ( 1.000000000000000000, 0.000000000000000000, 0.000000000000000000 ) ) ;
#99970 = CARTESIAN_POINT ( 'NONE',  ( -51.65034888587552331, -25.23263977359132681, 3.670420697275465383 ) ) ;
#99971 = VERTEX_POINT ( 'NONE', #30582 ) ;
#99972 = ORIENTED_EDGE ( 'NONE', *, *, #46621, .T. ) ;
#99973 = EDGE_CURVE ( 'NONE', #92846, #52051, #64569, .T. ) ;
#99974 = VERTEX_POINT ( 'NONE', #1648 ) ;
#99975 = CARTESIAN_POINT ( 'NONE',  ( -14.55006661338671847, 15.66751491618662406, -1.500000000000002220 ) ) ;
#99976 = VERTEX_POINT ( 'NONE', #18860 ) ;
#99977 = CARTESIAN_POINT ( 'NONE',  ( 2.700122536338566359, 20.86363338933649558, 11.49999999999998934 ) ) ;
#99978 = CARTESIAN_POINT ( 'NONE',  ( -30.63485893237310620, -23.79219688653859777, -0.9707498849204322378 ) ) ;
#99979 = CARTESIAN_POINT ( 'NONE',  ( 14.61581670307174008, 6.376774720514426953, -27.35847990810646024 ) ) ;
#99980 = DIRECTION ( 'NONE',  ( 1.000000000000000000, 3.773278334444167608E-23, 8.201307833595939069E-29 ) ) ;
#99981 = CARTESIAN_POINT ( 'NONE',  ( 17.26801960494244881, -13.64313956103151071, -1.500000000000002220 ) ) ;
#99982 = CARTESIAN_POINT ( 'NONE',  ( -87.56248950725333202, -23.48783264082478794, -1.443836473390063935 ) ) ;
#99983 = VERTEX_POINT ( 'NONE', #24967 ) ;
#99984 = CARTESIAN_POINT ( 'NONE',  ( -6.720452724358975338, -6.376774720514411854, 19.46153846153846700 ) ) ;
#99985 = DIRECTION ( 'NONE',  ( -1.000000000000000000, -0.000000000000000000, -0.000000000000000000 ) ) ;
#99986 = CIRCLE ( 'NONE', #90312, 1.399999999999988143 ) ;
#99987 = CARTESIAN_POINT ( 'NONE',  ( 30.93860345374796594, -6.475225279485573360, 19.84760796525321780 ) ) ;
#99988 = CARTESIAN_POINT ( 'NONE',  ( 14.76093561896379214, -5.965225279485572685, -26.55548769130089681 ) ) ;
#99989 = CIRCLE ( 'NONE', #10937, 0.8500000000000017542 ) ;
#99990 = CARTESIAN_POINT ( 'NONE',  ( -0.06465115118468270361, -22.21304004241711993, 9.174899246800716668 ) ) ;
#99991 = CARTESIAN_POINT ( 'NONE',  ( -4.730540317195566224, 20.75322969461001676, -1.500000000000002220 ) ) ;
#99992 = CARTESIAN_POINT ( 'NONE',  ( -46.55620429048340014, -23.48786465467240703, 11.44779295918255357 ) ) ;
#99993 = CARTESIAN_POINT ( 'NONE',  ( -107.5534830369236658, -24.15620529776628800, 10.23563542870659759 ) ) ;
#99994 = CARTESIAN_POINT ( 'NONE',  ( -90.62287095715002749, -24.51163499207176599, 0.6490370598554281445 ) ) ;
#99995 = CARTESIAN_POINT ( 'NONE',  ( -85.62287095715004170, -24.99156045073393173, 7.747789690856161648 ) ) ;
#99996 = CARTESIAN_POINT ( 'NONE',  ( 8.413247042826936806, 20.86129769029627923, -1.500000000000002220 ) ) ;
#99997 = B_SPLINE_SURFACE_WITH_KNOTS ( 'NONE', 3, 1, ( 
 ( #90110, #12971 ),
 ( #91595, #52548 ),
 ( #45938, #22073 ),
 ( #53056, #83985 ),
 ( #44442, #13969 ),
 ( #44945, #92095 ),
 ( #59674, #51557 ),
 ( #99202, #60175 ),
 ( #36823, #22562 ),
 ( #29208, #5866 ),
 ( #82487, #90603 ),
 ( #37329, #82980 ),
 ( #7352, #53557 ),
 ( #68273, #84485 ),
 ( #76849, #69264 ) ),
 .UNSPECIFIED., .F., .F., .F.,
 ( 4, 1, 1, 1, 1, 1, 1, 1, 1, 1, 1, 1, 4 ),
 ( 2, 2 ),
 ( 0.000000000000000000, 0.08524905100979000838, 0.1673265936178218727, 0.2481753245808510644, 0.3288290783116027405, 0.4099080969767707749, 0.4905844511407976838, 0.5729934871893911374, 0.6582648924880361019, 0.7442215773079896568, 0.8290604069913395380, 0.9139382978106164179, 1.000000000000000000 ),
 ( 0.000000000000000000, 1.000000000000000000 ),
 .UNSPECIFIED. ) ;
#99998 = CARTESIAN_POINT ( 'NONE',  ( -109.9080087008536140, -25.31476271379807841, 5.144092056987718209 ) ) ;
#99999 = ORIENTED_EDGE ( 'NONE', *, *, #61879, .F. ) ;
#100000 = CARTESIAN_POINT ( 'NONE',  ( -119.5228709571500758, -24.65952944569305316, 1.056160979905705899 ) ) ;
#100001 = CARTESIAN_POINT ( 'NONE',  ( 16.02095076306289201, 11.36058263404076030, 11.49999999999999645 ) ) ;
#100002 = PLANE ( 'NONE',  #81131 ) ;
#100003 = CARTESIAN_POINT ( 'NONE',  ( -100.6228709571500701, -23.47596703998600631, 11.44779298504227860 ) ) ;
#100004 = VERTEX_POINT ( 'NONE', #16858 ) ;
#100005 = CARTESIAN_POINT ( 'NONE',  ( -88.56234219288387521, -23.48786465467241413, 11.44779295918254469 ) ) ;
#100006 = CARTESIAN_POINT ( 'NONE',  ( -127.1722184633019594, -25.37177198963286173, 5.922902208572746297 ) ) ;
#100007 = CARTESIAN_POINT ( 'NONE',  ( -124.5198371736732241, -24.51419770103158768, 9.386484678747164523 ) ) ;
#100008 = CIRCLE ( 'NONE', #25510, 1.020000000000000018 ) ;
#100009 = CARTESIAN_POINT ( 'NONE',  ( -13.19171355488933983, -14.64934158388261665, 11.49999999999998934 ) ) ;
#100010 = ORIENTED_EDGE ( 'NONE', *, *, #28603, .T. ) ;
#100011 = CARTESIAN_POINT ( 'NONE',  ( -109.5639959713965510, -25.23865002439190164, 3.633762065615921077 ) ) ;
#100012 = DIRECTION ( 'NONE',  ( 0.000000000000000000, -0.9999999999976377785, -2.173523156925979128E-06 ) ) ;
#100013 = CIRCLE ( 'NONE', #56326, 1.835999999999999632 ) ;
#100014 = CALENDAR_DATE ( 2026, 9, 10 ) ;
#100015 = VERTEX_POINT ( 'NONE', #86866 ) ;
#100016 = CARTESIAN_POINT ( 'NONE',  ( 7.089543269230769162, -6.376774720514413630, 19.75741185897435415 ) ) ;
#100017 = CARTESIAN_POINT ( 'NONE',  ( -64.62287095715005592, -29.50250243563736774, 8.947779886222145151 ) ) ;
#100018 = CARTESIAN_POINT ( 'NONE',  ( -55.63444734018879245, -24.63355581998385446, 0.9682620441943891043 ) ) ;
#100019 = CARTESIAN_POINT ( 'NONE',  ( 32.74291612378888061, -3.662501476888925467, -3.918438066536008346 ) ) ;
#100020 = CARTESIAN_POINT ( 'NONE',  ( 5.994920710892026605, -6.376774720514429617, 21.76186867112717138 ) ) ;
#100021 = EDGE_CURVE ( 'NONE', #59761, #73050, #42228, .T. ) ;
#100022 = VECTOR ( 'NONE', #61093, 1000.000000000000000 ) ;
#100023 = CARTESIAN_POINT ( 'NONE',  ( -10.16634758543296613, 6.475225279485573360, 30.00402280011862288 ) ) ;
#100024 = ADVANCED_FACE ( 'NONE', ( #86374 ), #36371, .T. ) ;
#100025 = CARTESIAN_POINT ( 'NONE',  ( -29.49875734969026198, -0.3587747205144265483, 2.362022800118626531 ) ) ;
#100026 = CARTESIAN_POINT ( 'NONE',  ( -17.55682386033230102, 9.526633247210019917, 11.49999999999998934 ) ) ;
#100027 = EDGE_CURVE ( 'NONE', #99871, #62610, #81752, .T. ) ;
#100028 = CARTESIAN_POINT ( 'NONE',  ( -45.62287095715004881, -23.47593901973091235, -1.443836447539009749 ) ) ;
#100029 = LINE ( 'NONE', #22901, #74408 ) ;
#100030 = ORIENTED_EDGE ( 'NONE', *, *, #34236, .F. ) ;
#100031 = ADVANCED_FACE ( 'NONE', ( #40202 ), #34099, .T. ) ;
#100032 = CARTESIAN_POINT ( 'NONE',  ( -66.52287095715001897, -23.73907113216987952, -1.053371485793251905 ) ) ;
#100033 = CARTESIAN_POINT ( 'NONE',  ( -44.62287095715004881, -24.64965695001468404, 8.947790433994187609 ) ) ;
#100034 = CARTESIAN_POINT ( 'NONE',  ( -120.6228709571499991, -23.85196035786902158, -0.8779234886474771571 ) ) ;
#100035 = CARTESIAN_POINT ( 'NONE',  ( -48.52287095715006160, -24.64965694238574656, 8.947790433994203596 ) ) ;
#100036 = CARTESIAN_POINT ( 'NONE',  ( -27.70544111104076990, -25.26026286247342512, 1.628748458536643184 ) ) ;
#100037 = CARTESIAN_POINT ( 'NONE',  ( -1.649669150391666506, -6.376774720514411854, 19.67464842890028365 ) ) ;
#100038 = CARTESIAN_POINT ( 'NONE',  ( -79.62287095715007013, -24.66019654487199375, 8.947790411086128159 ) ) ;
#100039 = EDGE_CURVE ( 'NONE', #52932, #89989, #95988, .T. ) ;
#100040 = CARTESIAN_POINT ( 'NONE',  ( -40.52287095715004739, -24.91570333825474748, 8.075032458260915647 ) ) ;
#100041 = VERTEX_POINT ( 'NONE', #28967 ) ;
#100042 = CARTESIAN_POINT ( 'NONE',  ( 5.347689060783223702, 19.56899250667117229, -1.500000000000002220 ) ) ;
#100043 = CARTESIAN_POINT ( 'NONE',  ( -122.6244493178476631, -24.34968618360934300, 0.1864209137778896352 ) ) ;
#100044 = CARTESIAN_POINT ( 'NONE',  ( -19.80875734969026425, -5.965225279485572685, 31.02402280011862246 ) ) ;
#100045 = AXIS2_PLACEMENT_3D ( 'NONE', #71950, #56730, #49119 ) ;
#100046 = LINE ( 'NONE', #54406, #55766 ) ;
#100047 = ORIENTED_EDGE ( 'NONE', *, *, #68213, .T. ) ;
#100048 = CARTESIAN_POINT ( 'NONE',  ( -43.52287095715006160, -29.50250243563736774, 8.947779886222148704 ) ) ;
#100049 = CARTESIAN_POINT ( 'NONE',  ( 15.17442925503088169, 13.16703847180013831, -1.500000000000002220 ) ) ;
#100050 = CARTESIAN_POINT ( 'NONE',  ( 11.82777538550527119, 17.46297031709455183, 11.49999999999999645 ) ) ;
#100051 = CARTESIAN_POINT ( 'NONE',  ( 7.160000000000000142, 7.891155995661686795, 5.788828319098143993 ) ) ;
#100052 = CARTESIAN_POINT ( 'NONE',  ( 22.02032638543937182, 1.892999326154024553, -1.500000000000002220 ) ) ;
#100053 = CARTESIAN_POINT ( 'NONE',  ( -20.18818894172909140, 3.697778396234267184, -1.500000000000002220 ) ) ;
#100054 = CARTESIAN_POINT ( 'NONE',  ( -93.52287095715006160, -23.47596703998600631, 11.44779298504228393 ) ) ;
#100055 = CARTESIAN_POINT ( 'NONE',  ( -126.6228709571499991, -24.33832256527049154, 0.1851278514138672282 ) ) ;
#100056 = EDGE_LOOP ( 'NONE', ( #96153, #73630, #8805, #60798 ) ) ;
#100057 = CARTESIAN_POINT ( 'NONE',  ( -109.5228709571500616, -24.65952944569305316, 1.056160979905704123 ) ) ;
#100058 = ORIENTED_EDGE ( 'NONE', *, *, #92733, .F. ) ;
#100059 = CARTESIAN_POINT ( 'NONE',  ( -6.128026245051341192, -6.376774720514410077, 19.39236848396478763 ) ) ;
#100060 = CARTESIAN_POINT ( 'NONE',  ( -51.62287095715005592, -23.47593901973091235, -1.443836447539009749 ) ) ;
#100061 = ORIENTED_EDGE ( 'NONE', *, *, #28592, .F. ) ;
#100062 = VERTEX_POINT ( 'NONE', #88886 ) ;
#100063 = ORIENTED_EDGE ( 'NONE', *, *, #18653, .F. ) ;
#100064 = CARTESIAN_POINT ( 'NONE',  ( -118.6228709571500559, -24.64898659630368627, 1.056161002820833028 ) ) ;
#100065 = CARTESIAN_POINT ( 'NONE',  ( -31.55620429048339304, -23.47593901973091235, -1.443836447539013301 ) ) ;
#100066 = CARTESIAN_POINT ( 'NONE',  ( -50.62287095715005592, -23.47593901973091235, -1.443836447539009749 ) ) ;
#100067 = CARTESIAN_POINT ( 'NONE',  ( 10.45329875151443488, -17.81600612866554556, -1.500000000000002220 ) ) ;
#100068 = CARTESIAN_POINT ( 'NONE',  ( 5.966611984012316405, 20.80180421262142687, 11.49999999999999645 ) ) ;
#100069 = VERTEX_POINT ( 'NONE', #5134 ) ;
#100070 = CARTESIAN_POINT ( 'NONE',  ( -41.32836283488544638, -2.682774720514426559, 39.26872235229541985 ) ) ;
#100071 = DIRECTION ( 'NONE',  ( -0.1254312216594016538, 0.000000000000000000, -0.9921023176230513441 ) ) ;
#100072 = CARTESIAN_POINT ( 'NONE',  ( -11.68221627493902126, 19.09626523228051553, -1.500000000000002220 ) ) ;
#100073 = TOROIDAL_SURFACE ( 'NONE', #96931, 3.060000000000000053, 2.040000000000000036 ) ;
#100074 = CARTESIAN_POINT ( 'NONE',  ( -62.52287095715006160, -24.51283580621365132, 0.6167428607019704856 ) ) ;
#100075 = CARTESIAN_POINT ( 'NONE',  ( 14.61581670307174008, 6.376774720514426953, -27.35847990810646024 ) ) ;
#100076 = ORIENTED_EDGE ( 'NONE', *, *, #69772, .F. ) ;
#100077 = CARTESIAN_POINT ( 'NONE',  ( 32.85081302853803464, -3.622774720514426949, -13.10817780685209577 ) ) ;
#100078 = CARTESIAN_POINT ( 'NONE',  ( -49.55328999679814928, -23.96169478059712432, 10.65365249895718414 ) ) ;
#100079 = LINE ( 'NONE', #89641, #58406 ) ;
#100080 = CARTESIAN_POINT ( 'NONE',  ( -5.518977837361389582, -20.17201009624758257, 11.49999999999998934 ) ) ;
#100081 = ORIENTED_EDGE ( 'NONE', *, *, #37014, .F. ) ;
#100082 = EDGE_CURVE ( 'NONE', #6498, #98033, #95052, .T. ) ;
#100083 = CARTESIAN_POINT ( 'NONE',  ( -86.51070039854617733, -24.15543982623907837, -0.2315651400026493834 ) ) ;
#100084 = AXIS2_PLACEMENT_3D ( 'NONE', #60448, #82262, #36582 ) ;
#100085 = ORIENTED_EDGE ( 'NONE', *, *, #48935, .F. ) ;
#100086 = DIRECTION ( 'NONE',  ( 3.773278334444166432E-23, -1.000000000000000000, 0.000000000000000000 ) ) ;
#100087 = CARTESIAN_POINT ( 'NONE',  ( 15.74494995282791088, 14.18698661492608615, -1.500000000000002220 ) ) ;
#100088 = ORIENTED_EDGE ( 'NONE', *, *, #93055, .F. ) ;
#100089 = CARTESIAN_POINT ( 'NONE',  ( -117.5566936579932786, -23.73766607897671221, -1.055555164236445576 ) ) ;
#100090 = CARTESIAN_POINT ( 'NONE',  ( -99.53757426446047418, -25.26221240933978862, 6.745911554810026800 ) ) ;
#100091 = CARTESIAN_POINT ( 'NONE',  ( 19.23208339725441007, -10.27600428404867827, -1.500000000000002220 ) ) ;
#100092 = CARTESIAN_POINT ( 'NONE',  ( -121.5228709571500190, -24.66019654487199730, 8.947790411086119278 ) ) ;
#100093 = DIRECTION ( 'NONE',  ( 1.000000000000000000, 3.773278334444167608E-23, 8.201307833595939069E-29 ) ) ;
#100094 = CARTESIAN_POINT ( 'NONE',  ( -32.92287095715006018, -23.47593901973090169, -1.443836447538998424 ) ) ;
#100095 = CARTESIAN_POINT ( 'NONE',  ( 21.79142754302170815, -0.6654467836950721527, -1.500000000000002220 ) ) ;
#100096 = CARTESIAN_POINT ( 'NONE',  ( -71.39239612577370053, -25.31639534936708813, 5.186401758698863773 ) ) ;
#100097 = ORIENTED_EDGE ( 'NONE', *, *, #4122, .F. ) ;
#100098 = CARTESIAN_POINT ( 'NONE',  ( -67.52287095715003318, -23.47593901973090169, -1.443836447538996870 ) ) ;
#100099 = CARTESIAN_POINT ( 'NONE',  ( -72.62287095715005592, -24.65952944569304606, 1.056160979905698794 ) ) ;
#100100 = CARTESIAN_POINT ( 'NONE',  ( 32.24176898385614720, -6.243294140736224129, 2.116998906223432453 ) ) ;
#100101 = ORIENTED_EDGE ( 'NONE', *, *, #34042, .F. ) ;
#100102 = ORIENTED_EDGE ( 'NONE', *, *, #88168, .T. ) ;
#100103 = CIRCLE ( 'NONE', #77447, 2.399999999999999911 ) ;
#100104 = VERTEX_POINT ( 'NONE', #27486 ) ;
#100105 = DIRECTION ( 'NONE',  ( -2.338552693767719605E-15, 0.000000000000000000, 1.000000000000000000 ) ) ;
#100106 = CARTESIAN_POINT ( 'NONE',  ( 9.480266252741309074, -18.97159823121752709, 11.49999999999998934 ) ) ;
#100107 = CARTESIAN_POINT ( 'NONE',  ( -94.55792956946962136, -23.73766607897670156, -1.055555164236450905 ) ) ;
#100108 = CARTESIAN_POINT ( 'NONE',  ( -79.61785653407703478, -25.03138245405229512, 7.314036780457776388 ) ) ;
#100109 = CARTESIAN_POINT ( 'NONE',  ( 20.84838633257991347, -4.362234729430479518, -17.34205791096968241 ) ) ;
#100110 = DIRECTION ( 'NONE',  ( 0.000000000000000000, -0.000000000000000000, -1.000000000000000000 ) ) ;
#100111 = CARTESIAN_POINT ( 'NONE',  ( -18.68205546197936684, -5.105407162728520021, -1.500000000000002220 ) ) ;
#100112 = CARTESIAN_POINT ( 'NONE',  ( -45.50997245640682820, -23.85016227208580020, -0.8807180028928389692 ) ) ;
#100113 = ORIENTED_EDGE ( 'NONE', *, *, #97697, .F. ) ;
#100114 = CARTESIAN_POINT ( 'NONE',  ( -19.44331071757236273, 1.017868325215548708, 11.49999999999999645 ) ) ;
#100115 = CARTESIAN_POINT ( 'NONE',  ( 33.13288845015618023, -0.3587747205144265483, -0.1650522222209214185 ) ) ;
#100116 = CARTESIAN_POINT ( 'NONE',  ( -91.94687923781920347, -29.50249691823240994, 6.409318347766594037 ) ) ;
#100117 = ORIENTED_EDGE ( 'NONE', *, *, #28257, .T. ) ;
#100118 = CARTESIAN_POINT ( 'NONE',  ( -78.62287095715005592, -23.47596703998600631, 11.44779298504227860 ) ) ;
#100119 = DIRECTION ( 'NONE',  ( -0.06283980576413539243, -0.000000000000000000, -0.9980236263794188822 ) ) ;
#100120 = DIRECTION ( 'NONE',  ( 0.000000000000000000, -2.173523156925980399E-06, 0.9999999999976378895 ) ) ;
#100121 = EDGE_CURVE ( 'NONE', #47247, #58571, #53902, .T. ) ;
#100122 = CARTESIAN_POINT ( 'NONE',  ( -93.56158678139395590, -23.48786465467241058, 11.44779295918254469 ) ) ;
#100123 = CARTESIAN_POINT ( 'NONE',  ( -17.63651738508609412, 8.604534254076446231, 11.49999999999998934 ) ) ;
#100124 = B_SPLINE_SURFACE_WITH_KNOTS ( 'NONE', 3, 1, ( 
 ( #36514, #68967 ),
 ( #67480, #29902 ),
 ( #90809, #22272 ),
 ( #21280, #53256 ),
 ( #84184, #14675 ),
 ( #9070, #69469 ),
 ( #56271, #8577 ),
 ( #39016, #9569 ),
 ( #47647, #30904 ),
 ( #85697, #94298 ),
 ( #79073, #77565 ),
 ( #40023, #46645 ),
 ( #17178, #7569 ),
 ( #40535, #39523 ),
 ( #61870, #78562 ),
 ( #24786, #55765 ),
 ( #8068, #48149 ),
 ( #32412, #31912 ),
 ( #70980, #960 ) ),
 .UNSPECIFIED., .F., .F., .F.,
 ( 4, 1, 1, 1, 1, 1, 1, 1, 1, 1, 1, 1, 1, 1, 1, 1, 4 ),
 ( 2, 2 ),
 ( 0.000000000000000000, 0.07563486594245749650, 0.1456749912579857753, 0.2101933844674984675, 0.2691971886348948351, 0.3228467966362095209, 0.3711350468222360810, 0.4143602045761041186, 0.4526539356929057956, 0.5231868047418553047, 0.5919172609462788337, 0.6599757056395081367, 0.7292117337225374474, 0.7981350023964017826, 0.8652933977976435820, 0.9318417558440023063, 1.000000000000000000 ),
 ( 0.000000000000000000, 1.000000000000000000 ),
 .UNSPECIFIED. ) ;
#100125 = DIRECTION ( 'NONE',  ( 0.000000000000000000, 0.000000000000000000, 1.000000000000000000 ) ) ;
#100126 = ORIENTED_EDGE ( 'NONE', *, *, #90540, .T. ) ;
#100127 = CARTESIAN_POINT ( 'NONE',  ( 7.401388779597747103, 20.28278527911644247, 11.49999999999998934 ) ) ;
#100128 = CARTESIAN_POINT ( 'NONE',  ( 5.326923076923078426, -5.876774720514419847, 20.76772836538461320 ) ) ;
#100129 = PLANE ( 'NONE',  #55739 ) ;
#100130 = CYLINDRICAL_SURFACE ( 'NONE', #48908, 12.65241003308275936 ) ;
#100131 = CARTESIAN_POINT ( 'NONE',  ( -22.90524134523018773, 2.401388714834002069, -1.500000000000002220 ) ) ;
#100132 = DATE_AND_TIME ( #69217, #78071 ) ;
#100133 = CARTESIAN_POINT ( 'NONE',  ( -93.51253909850096591, -24.15543982623907837, -0.2315651400026621232 ) ) ;
#100134 = LINE ( 'NONE', #74828, #81477 ) ;
#100135 = CARTESIAN_POINT ( 'NONE',  ( -17.47620107869530770, 10.18187089365592612, 11.49999999999999645 ) ) ;
#100136 = DIRECTION ( 'NONE',  ( -3.773278334453079618E-23, 0.9999999999976377785, 2.173523156925979975E-06 ) ) ;
#100137 = DIRECTION ( 'NONE',  ( -3.773278334453080206E-23, 0.9999999999976377785, 2.173523156925979975E-06 ) ) ;
#100138 = ADVANCED_FACE ( 'NONE', ( #74152 ), #51316, .F. ) ;
#100139 = CARTESIAN_POINT ( 'NONE',  ( -110.3139465455115129, -25.10921373951931557, 2.832404819737793122 ) ) ;
#100140 = CARTESIAN_POINT ( 'NONE',  ( -29.58953762381672448, -23.40617605126033851, 11.44779300154114843 ) ) ;
#100141 = CARTESIAN_POINT ( 'NONE',  ( -99.12529836037420239, -25.26400692580550000, 4.049155320992488427 ) ) ;
#100142 = CARTESIAN_POINT ( 'NONE',  ( 17.36586316225375981, 9.700842922841564686, -1.500000000000002220 ) ) ;
#100143 = EDGE_CURVE ( 'NONE', #98594, #95213, #22420, .T. ) ;
#100144 = DIRECTION ( 'NONE',  ( 0.000000000000000000, 0.9999999999976377785, 2.173523156925979975E-06 ) ) ;
#100145 = CARTESIAN_POINT ( 'NONE',  ( 16.01007288495529224, -11.65062672332236104, -1.500000000000002220 ) ) ;
#100146 = CIRCLE ( 'NONE', #17616, 0.2500000000000011102 ) ;
#100147 = CARTESIAN_POINT ( 'NONE',  ( -56.58275159101006579, -24.51314013834315730, 0.6176544820404098468 ) ) ;
#100148 = EDGE_CURVE ( 'NONE', #1588, #7066, #95695, .T. ) ;
#100149 = ADVANCED_FACE ( 'NONE', ( #68046 ), #23273, .T. ) ;
#100150 = CARTESIAN_POINT ( 'NONE',  ( -39.89740106121153929, -25.10925613793910571, 2.930848149893042098 ) ) ;
#100151 = CARTESIAN_POINT ( 'NONE',  ( -37.52287095715009002, -23.96127896942118696, -0.6493128930941863830 ) ) ;
#100152 = CARTESIAN_POINT ( 'NONE',  ( -11.67826063220891086, 17.12864047899337550, 11.49999999999999645 ) ) ;
#100153 = FACE_OUTER_BOUND ( 'NONE', #37030, .T. ) ;
#100154 = EDGE_CURVE ( 'NONE', #59954, #76732, #81762, .T. ) ;
#100155 = CARTESIAN_POINT ( 'NONE',  ( -49.76870215116556295, -25.31439312223557181, 5.358736678790748442 ) ) ;
#100156 = CARTESIAN_POINT ( 'NONE',  ( 2.440706796964721370, 22.61111150098722788, 11.49999999999999645 ) ) ;
#100157 = ORIENTED_EDGE ( 'NONE', *, *, #22363, .T. ) ;
#100158 = DIRECTION ( 'NONE',  ( -1.000000000000000000, -1.232047923278981953E-16, 0.000000000000000000 ) ) ;
#100159 = LINE ( 'NONE', #38285, #25738 ) ;
#100160 = B_SPLINE_CURVE_WITH_KNOTS ( 'NONE', 3,
 ( #52897, #99537, #61011, #91944, #53400, #93435, #93943, #71623, #17323, #15815, #1613, #2121 ),
 .UNSPECIFIED., .F., .F.,
 ( 4, 2, 2, 2, 2, 4 ),
 ( 0.000000000000000000, 0.08114505568447454020, 0.1622901113689490804, 0.3245802227378981608, 0.4868703341068472135, 0.6491604454757963216 ),
 .UNSPECIFIED. ) ;
#100161 = AXIS2_PLACEMENT_3D ( 'NONE', #45770, #92930, #85320 ) ;
#100162 = CARTESIAN_POINT ( 'NONE',  ( 13.23653054071972512, 15.24542462990338088, -1.500000000000002220 ) ) ;
#100163 = EDGE_CURVE ( 'NONE', #64365, #71450, #58930, .T. ) ;
#100164 = CARTESIAN_POINT ( 'NONE',  ( -5.366453405989236813, 2.939152317953647894E-15, -24.00000000000000000 ) ) ;
#100165 = FACE_OUTER_BOUND ( 'NONE', #12955, .T. ) ;
#100166 = ORIENTED_EDGE ( 'NONE', *, *, #92835, .F. ) ;
#100167 = VERTEX_POINT ( 'NONE', #28464 ) ;
#100168 = DIRECTION ( 'NONE',  ( -0.000000000000000000, 1.000000000000000000, -0.000000000000000000 ) ) ;
#100169 = CARTESIAN_POINT ( 'NONE',  ( 16.30191990219073972, -16.09819076282585826, 11.49999999999998934 ) ) ;
#100170 = CARTESIAN_POINT ( 'NONE',  ( -51.26181408848110976, -25.18439757638810761, 3.790033046355993918 ) ) ;
#100171 = CARTESIAN_POINT ( 'NONE',  ( -16.79864850723062020, -13.61054813162024679, -1.500000000000002220 ) ) ;
#100172 = AXIS2_PLACEMENT_3D ( 'NONE', #12693, #75091, #20799 ) ;
#100173 = CARTESIAN_POINT ( 'NONE',  ( -123.5198859968498510, -24.34968618360933945, 0.1864209137778902459 ) ) ;
#100174 = DIRECTION ( 'NONE',  ( -3.773278334453079618E-23, 0.9999999999976377785, 2.173523156925979975E-06 ) ) ;
#100175 = CARTESIAN_POINT ( 'NONE',  ( 14.99592430652175956, 14.54719766626331889, 11.49999999999999645 ) ) ;
#100176 = ORIENTED_EDGE ( 'NONE', *, *, #58106, .F. ) ;
#100177 = CARTESIAN_POINT ( 'NONE',  ( 27.53860345374771867, 4.772774720514425972, -9.482392034746240483 ) ) ;
#100178 = CARTESIAN_POINT ( 'NONE',  ( -11.61111146657235871, -18.70866699758865792, -1.500000000000002220 ) ) ;
#100179 = CARTESIAN_POINT ( 'NONE',  ( -105.5074300981244875, -25.00182538069147142, 7.747789668545045139 ) ) ;
#100180 = CARTESIAN_POINT ( 'NONE',  ( -30.47287095715007510, -25.26798360067225246, 6.132490479008352757 ) ) ;
#100181 = VERTEX_POINT ( 'NONE', #59429 ) ;
#100182 = CARTESIAN_POINT ( 'NONE',  ( 4.588387839717440464, -6.376774720514401196, 18.52756237589653665 ) ) ;
#100183 = DIRECTION ( 'NONE',  ( 0.000000000000000000, 0.000000000000000000, -1.000000000000000000 ) ) ;
#100184 = ORIENTED_EDGE ( 'NONE', *, *, #52014, .F. ) ;
#100185 = CARTESIAN_POINT ( 'NONE',  ( -72.54158254937220818, -24.51419770103156281, 9.386484678747185839 ) ) ;
#100186 = ORIENTED_EDGE ( 'NONE', *, *, #72010, .T. ) ;
#100187 = ORIENTED_EDGE ( 'NONE', *, *, #81963, .T. ) ;
#100188 = CARTESIAN_POINT ( 'NONE',  ( -32.62287095715004881, -24.64898659630367206, 1.056161002820817485 ) ) ;
#100189 = CARTESIAN_POINT ( 'NONE',  ( -0.02075734969026423599, -5.965225279485572685, -0.08597719988137648983 ) ) ;
#100190 = CARTESIAN_POINT ( 'NONE',  ( -4.141166922167975883, -6.376774720514420736, 20.63520656483649063 ) ) ;
#100191 = CARTESIAN_POINT ( 'NONE',  ( 16.92567061652012228, 11.46397006495115534, -1.500000000000002220 ) ) ;
#100192 = ADVANCED_FACE ( 'NONE', ( #90370 ), #20845, .T. ) ;
#100193 = ORIENTED_EDGE ( 'NONE', *, *, #57526, .T. ) ;
#100194 = DIRECTION ( 'NONE',  ( 0.000000000000000000, 0.000000000000000000, 1.000000000000000000 ) ) ;
#100195 = LINE ( 'NONE', #70283, #32032 ) ;
#100196 = CARTESIAN_POINT ( 'NONE',  ( -99.62287095715005592, -23.48783264082478794, -1.443836473390061936 ) ) ;
#100197 = CARTESIAN_POINT ( 'NONE',  ( -22.27612280437926273, 0.2766752662994830247, 11.49999999999998934 ) ) ;
#100198 = EDGE_CURVE ( 'NONE', #14515, #25882, #98466, .T. ) ;
#100199 = CARTESIAN_POINT ( 'NONE',  ( -37.62287095715005592, -29.50250786944525672, 11.44777988621624232 ) ) ;
#100200 = DIRECTION ( 'NONE',  ( 1.000000000000000000, -0.000000000000000000, 0.000000000000000000 ) ) ;
#100201 = VERTEX_POINT ( 'NONE', #37584 ) ;
#100202 = B_SPLINE_CURVE_WITH_KNOTS ( 'NONE', 3,
 ( #48041, #54655, #39917, #39422, #859, #1865 ),
 .UNSPECIFIED., .F., .F.,
 ( 4, 2, 4 ),
 ( 0.000000000000000000, 0.001380764517854760195, 0.002761529035709520390 ),
 .UNSPECIFIED. ) ;
#100203 = CARTESIAN_POINT ( 'NONE',  ( -28.90439778889242461, -24.81322729368779179, 2.055611166137502721 ) ) ;
#100204 = CARTESIAN_POINT ( 'NONE',  ( -29.47349813062140100, -24.63645800325529933, 7.035456400021670831 ) ) ;
#100205 = CARTESIAN_POINT ( 'NONE',  ( 12.46380520747237419, 16.70348211664046900, -1.500000000000002220 ) ) ;
#100206 = ORIENTED_EDGE ( 'NONE', *, *, #6924, .T. ) ;
#100208 = VERTEX_POINT ( 'NONE', #45701 ) ;
#100207 = CARTESIAN_POINT ( 'NONE',  ( 33.69795529655567634, -0.6647747205144264315, 23.11160796525322070 ) ) ;
#100209 = B_SPLINE_SURFACE_WITH_KNOTS ( 'NONE', 3, 1, ( 
 ( #12985, #61189 ),
 ( #52565, #37344 ),
 ( #99701, #44959 ),
 ( #37830, #68784 ),
 ( #43950, #92109 ),
 ( #83497, #5880 ),
 ( #36842, #7366 ),
 ( #59688, #53574 ),
 ( #29221, #21098 ),
 ( #76865, #53072 ),
 ( #67297, #52066 ),
 ( #51571, #75884 ),
 ( #91609, #20602 ),
 ( #84499, #38319 ),
 ( #30206, #36341 ),
 ( #98218, #5386 ),
 ( #6384, #69279 ),
 ( #60189, #68287 ),
 ( #44456, #99216 ) ),
 .UNSPECIFIED., .F., .F., .F.,
 ( 4, 1, 1, 1, 1, 1, 1, 1, 1, 1, 1, 1, 1, 1, 1, 1, 4 ),
 ( 2, 2 ),
 ( 0.000000000000000000, 0.06761452606740225857, 0.1311670463014497079, 0.1902933887105121569, 0.2450610151831991157, 0.2960272302790619703, 0.3428447301738881681, 0.3860527037713289422, 0.4255709801320508578, 0.4995034801514162126, 0.5702922612469554231, 0.6402757819125015626, 0.7105295546786241090, 0.7812030014762990637, 0.8520349845172640046, 0.9243956695042545579, 1.000000000000000000 ),
 ( 0.000000000000000000, 1.000000000000000000 ),
 .UNSPECIFIED. ) ;
#100210 = CARTESIAN_POINT ( 'NONE',  ( -51.11259392460791418, -25.25854530677348109, 6.923368444302069769 ) ) ;
#100212 = EDGE_LOOP ( 'NONE', ( #61532, #30982 ) ) ;
#100211 = ADVANCED_FACE ( 'NONE', ( #62432 ), #8142, .T. ) ;
#100213 = ORIENTED_EDGE ( 'NONE', *, *, #97455, .F. ) ;
#100214 = DIRECTION ( 'NONE',  ( -0.000000000000000000, -0.000000000000000000, -1.000000000000000000 ) ) ;
#100215 = PLANE ( 'NONE',  #77180 ) ;
#100216 = CARTESIAN_POINT ( 'NONE',  ( -111.9545732713065291, -25.06732945298220372, 7.447791367849804445 ) ) ;
#100217 = VECTOR ( 'NONE', #98074, 1000.000000000000000 ) ;
#100218 = CARTESIAN_POINT ( 'NONE',  ( -20.27875734969026311, -6.143225279485574397, 24.00402280011862288 ) ) ;
#100219 = FACE_OUTER_BOUND ( 'NONE', #37470, .T. ) ;
#100220 = CARTESIAN_POINT ( 'NONE',  ( -100.6228709571500559, -25.00182538069145721, 7.747789668545099317 ) ) ;
#100222 = ORIENTED_EDGE ( 'NONE', *, *, #34481, .F. ) ;
#100221 = CARTESIAN_POINT ( 'NONE',  ( 14.71430157977438924, -16.63553917435140406, 11.49999999999999645 ) ) ;
#100223 = EDGE_CURVE ( 'NONE', #14845, #99263, #7636, .T. ) ;
#100224 = CARTESIAN_POINT ( 'NONE',  ( -38.62287095715004881, -24.51283580621364067, 0.6167428607019701525 ) ) ;
#100225 = ORIENTED_EDGE ( 'NONE', *, *, #49674, .T. ) ;
#100226 = CARTESIAN_POINT ( 'NONE',  ( 18.27610663105864219, 13.37729726205769154, -1.500000000000002220 ) ) ;
#100227 = VECTOR ( 'NONE', #36298, 1000.000000000000000 ) ;
#100229 = VERTEX_POINT ( 'NONE', #14230 ) ;
#100228 = DIRECTION ( 'NONE',  ( -0.000000000000000000, 1.000000000000000000, -0.000000000000000000 ) ) ;
#100230 = VERTEX_POINT ( 'NONE', #6630 ) ;
#100231 = VECTOR ( 'NONE', #15309, 1000.000000000000114 ) ;
#100232 = CARTESIAN_POINT ( 'NONE',  ( -48.62287095715004881, -29.50250243563736774, 8.947779886222146928 ) ) ;
#100233 = APPROVAL ( #24032, 'UNSPECIFIED' ) ;
#100234 = CARTESIAN_POINT ( 'NONE',  ( -12.53166870608491479, 15.75175023352509385, 11.49999999999998934 ) ) ;
#100235 = DIRECTION ( 'NONE',  ( -3.773278334453079030E-23, 0.9999999999976377785, 2.173523156925979128E-06 ) ) ;
#100236 = ORIENTED_EDGE ( 'NONE', *, *, #91665, .T. ) ;
#100237 = VECTOR ( 'NONE', #70370, 1000.000000000000114 ) ;
#100238 = CARTESIAN_POINT ( 'NONE',  ( -58.52287095715004739, -23.48783264082477018, -1.443836473390092801 ) ) ;
#100239 = CARTESIAN_POINT ( 'NONE',  ( -10.99827004860668822, -19.42154297629913628, -1.500000000000002220 ) ) ;
#100240 = ORIENTED_EDGE ( 'NONE', *, *, #93180, .T. ) ;
#100241 = ORIENTED_EDGE ( 'NONE', *, *, #88393, .F. ) ;
#100242 = DIRECTION ( 'NONE',  ( 0.000000000000000000, 0.000000000000000000, 1.000000000000000000 ) ) ;
#100243 = LINE ( 'NONE', #38868, #18336 ) ;
#100244 = FACE_OUTER_BOUND ( 'NONE', #19705, .T. ) ;
#100245 = CARTESIAN_POINT ( 'NONE',  ( -68.52287095715001897, -23.73934037231756022, 11.05740245334328975 ) ) ;
#100246 = FACE_BOUND ( 'NONE', #30703, .T. ) ;
#100247 = CARTESIAN_POINT ( 'NONE',  ( 18.95637782189878706, 4.751392969308117387, -1.500000000000002220 ) ) ;
#100248 = CARTESIAN_POINT ( 'NONE',  ( 30.09341516180546350, -1.682774720514426114, -11.39311774897855933 ) ) ;
#100249 = CARTESIAN_POINT ( 'NONE',  ( -12.84383942963603964, -17.20202612561282862, 11.49999999999998934 ) ) ;
#100250 = CARTESIAN_POINT ( 'NONE',  ( -25.64067666839992299, -24.57999935372392741, 3.645612436503677500 ) ) ;
#100251 = CARTESIAN_POINT ( 'NONE',  ( -46.62287095715004881, -23.47596703998600276, 11.44779298504227505 ) ) ;
#100252 = CARTESIAN_POINT ( 'NONE',  ( -113.5228709571500474, -23.73934037231757443, 11.05740245334328087 ) ) ;
#100253 = CARTESIAN_POINT ( 'NONE',  ( -32.07722060962682775, -25.11010177581465186, 2.831122766525584478 ) ) ;
#100254 = CARTESIAN_POINT ( 'NONE',  ( 12.66508800429495629, 19.07499079241581086, -1.500000000000002220 ) ) ;
#100255 = AXIS2_PLACEMENT_3D ( 'NONE', #20659, #67358, #6446 ) ;
#100256 = DATE_AND_TIME ( #1338, #29411 ) ;
#100257 = CYLINDRICAL_SURFACE ( 'NONE', #7751, 91.74549126261076992 ) ;
#100258 = CARTESIAN_POINT ( 'NONE',  ( -108.5228709571501327, -23.96127896942116564, -0.6493128930942506649 ) ) ;
#100259 = CARTESIAN_POINT ( 'NONE',  ( 17.53424486177994623, -9.724335930198575895, 11.49999999999999645 ) ) ;
#100260 = CARTESIAN_POINT ( 'NONE',  ( -78.99596516450635875, -25.26612595557550378, 5.526334007569491114 ) ) ;
#100261 = CARTESIAN_POINT ( 'NONE',  ( 30.53060340732036337, 4.484642458114688424, -4.073424848557150924 ) ) ;
#100262 = DIRECTION ( 'NONE',  ( -3.773278334453079618E-23, 0.9999999999976377785, 2.173523156925979975E-06 ) ) ;
#100263 = CARTESIAN_POINT ( 'NONE',  ( -3.212051231530180573, 17.72614232434105119, 0.000000000000000000 ) ) ;
#100264 = EDGE_CURVE ( 'NONE', #27790, #991, #6622, .T. ) ;
#100265 = ORIENTED_EDGE ( 'NONE', *, *, #98965, .F. ) ;
#100266 = CARTESIAN_POINT ( 'NONE',  ( -27.70544111104076990, -24.61528742064533049, 1.628749860405701799 ) ) ;
#100267 = DIRECTION ( 'NONE',  ( -3.773278334453079618E-23, 0.9999999999976377785, 2.173523156925979975E-06 ) ) ;
#100268 = CARTESIAN_POINT ( 'NONE',  ( 2.995010171738120786, 21.53247193037183038, 11.49999999999998934 ) ) ;
#100269 = PLANE ( 'NONE',  #78797 ) ;
#100270 = CARTESIAN_POINT ( 'NONE',  ( -5.058734511472819051, -18.94576116945722788, -1.500000000000002220 ) ) ;
#100271 = CARTESIAN_POINT ( 'NONE',  ( -85.52287095715007581, -24.83620972994591725, 8.398175272781369216 ) ) ;
#100272 = CARTESIAN_POINT ( 'NONE',  ( -41.24596773881854972, -25.22682451471871090, 3.618500823024371371 ) ) ;
#100273 = DATE_AND_TIME ( #40412, #99299 ) ;
#100274 = EDGE_CURVE ( 'NONE', #17650, #52247, #44197, .T. ) ;
#100275 = FACE_OUTER_BOUND ( 'NONE', #52497, .T. ) ;
#100276 = CARTESIAN_POINT ( 'NONE',  ( 3.797776442307698286, -5.876774720514427841, 21.83974358974358410 ) ) ;
#100277 = CARTESIAN_POINT ( 'NONE',  ( 1.259202695315177589, 20.44674571593545664, 11.49999999999999645 ) ) ;
#100278 = CARTESIAN_POINT ( 'NONE',  ( 30.59431191903084013, 4.508530027678929741, 26.46517314890041916 ) ) ;
#100279 = EDGE_CURVE ( 'NONE', #13521, #80017, #83750, .T. ) ;
#100280 = CARTESIAN_POINT ( 'NONE',  ( -120.5523430223616828, -24.92564183028979841, 1.928384488918253536 ) ) ;
#100281 = ORIENTED_EDGE ( 'NONE', *, *, #57873, .T. ) ;
#100282 = CARTESIAN_POINT ( 'NONE',  ( -100.5167721066480908, -25.26387453228739588, 4.733455361238839032 ) ) ;
#100283 = DIRECTION ( 'NONE',  ( -0.9978940991575084851, -0.000000000000000000, -0.06486421869277853025 ) ) ;
#100284 = VECTOR ( 'NONE', #58655, 1000.000000000000114 ) ;
#100285 = CARTESIAN_POINT ( 'NONE',  ( -0.02075734969026423599, 3.316774720514426456, -28.03397719988137382 ) ) ;
#100286 = CARTESIAN_POINT ( 'NONE',  ( -24.97666371003640506, 0.3587747205143964613, -15.72894043976419454 ) ) ;
#100287 = AXIS2_PLACEMENT_3D ( 'NONE', #71760, #2252, #48927 ) ;
#100288 = EDGE_CURVE ( 'NONE', #37811, #60161, #45205, .T. ) ;
#100289 = CARTESIAN_POINT ( 'NONE',  ( -25.53215482860445107, -24.61459415544598883, 5.039155396214215266 ) ) ;
#100290 = CARTESIAN_POINT ( 'NONE',  ( 31.55302460176084978, 5.360765615368469739, -3.312397695011010335 ) ) ;
#100291 = VECTOR ( 'NONE', #31663, 1000.000000000000000 ) ;
#100292 = CARTESIAN_POINT ( 'NONE',  ( 19.44587849558928738, -12.39355811350142922, 11.49999999999999645 ) ) ;
#100293 = CARTESIAN_POINT ( 'NONE',  ( -7.756741253720922380, -21.46081514045699024, -1.500000000000002220 ) ) ;
#100294 = CARTESIAN_POINT ( 'NONE',  ( -74.51666569301140441, -23.73766607897670511, -1.055555164236458898 ) ) ;
#100295 = CARTESIAN_POINT ( 'NONE',  ( -67.52287095715009002, -23.48783264082477018, -1.443836473390090802 ) ) ;
#100296 = CARTESIAN_POINT ( 'NONE',  ( -57.52287095715008292, -23.47593901973090524, -1.443836447538997092 ) ) ;
#100297 = CARTESIAN_POINT ( 'NONE',  ( 16.55124408090292576, 15.08944307983326638, 11.49999999999999645 ) ) ;
#100298 = VERTEX_POINT ( 'NONE', #21840 ) ;
#100299 = VECTOR ( 'NONE', #89469, 1000.000000000000000 ) ;
#100300 = CARTESIAN_POINT ( 'NONE',  ( -40.52287095715005449, -24.92604778743017491, 8.074972756849357225 ) ) ;
#100301 = CARTESIAN_POINT ( 'NONE',  ( -43.52203320906042450, -23.48783264082478084, -1.443836473390076369 ) ) ;
#100302 = CARTESIAN_POINT ( 'NONE',  ( 11.39931579351042679, 18.75040340349860557, 11.49999999999998934 ) ) ;
#100303 = CARTESIAN_POINT ( 'NONE',  ( -5.706951327759631099, -5.876774720514411854, 19.48569229636961353 ) ) ;
#100304 = CARTESIAN_POINT ( 'NONE',  ( -87.63899336050222644, -23.73791477778911840, 11.05961554403170588 ) ) ;
#100305 = FACE_OUTER_BOUND ( 'NONE', #9492, .T. ) ;
#100306 = CARTESIAN_POINT ( 'NONE',  ( 11.62916340711181284, 5.965225279485572685, 28.75961759920349792 ) ) ;
#100307 = DIRECTION ( 'NONE',  ( 0.000000000000000000, 0.000000000000000000, -1.000000000000000000 ) ) ;
#100308 = ORIENTED_EDGE ( 'NONE', *, *, #98122, .F. ) ;
#100309 = AXIS2_PLACEMENT_3D ( 'NONE', #93215, #77483, #78486 ) ;
#100310 = CARTESIAN_POINT ( 'NONE',  ( 4.362881659454829197, 20.01674633476859810, 11.49999999999998934 ) ) ;
#100311 =( BOUNDED_CURVE ( )  B_SPLINE_CURVE ( 3, ( #66434, #18722, #59297, #28337 ),
 .UNSPECIFIED., .F., .T. ) 
 B_SPLINE_CURVE_WITH_KNOTS ( ( 4, 4 ),
 ( 4.712388980384689674, 4.821597757366586912 ),
 .UNSPECIFIED. ) 
 CURVE ( )  GEOMETRIC_REPRESENTATION_ITEM ( )  RATIONAL_B_SPLINE_CURVE ( ( 1.000000000000000000, 0.9990063671772055898, 0.9990063671772055898, 1.000000000000000000 ) ) 
 REPRESENTATION_ITEM ( '' )  );
#100312 = ORIENTED_EDGE ( 'NONE', *, *, #12531, .F. ) ;
#100313 = VERTEX_POINT ( 'NONE', #76132 ) ;
#100314 = ORIENTED_EDGE ( 'NONE', *, *, #2514, .F. ) ;
#100315 = VERTEX_POINT ( 'NONE', #23850 ) ;
#100316 = CARTESIAN_POINT ( 'NONE',  ( -21.10450430117995424, 9.351148110661185342, 11.49999999999998934 ) ) ;
#100317 = PLANE ( 'NONE',  #79542 ) ;
#100318 = CARTESIAN_POINT ( 'NONE',  ( 20.05935882324986963, -3.104462954613115500, -1.500000000000002220 ) ) ;
#100319 = ORIENTED_EDGE ( 'NONE', *, *, #89894, .T. ) ;
#100320 = CARTESIAN_POINT ( 'NONE',  ( -90.62287095715002749, -25.00182538069145366, 7.747789668545099317 ) ) ;
#100321 = DIRECTION ( 'NONE',  ( 0.000000000000000000, -1.000000000000000000, 0.000000000000000000 ) ) ;
#100322 = ADVANCED_FACE ( 'NONE', ( #52815 ), #54824, .T. ) ;
#100323 = LINE ( 'NONE', #99827, #22134 ) ;
#100324 = CARTESIAN_POINT ( 'NONE',  ( -99.55261023400132103, -24.15620529776628800, 10.23563542870660115 ) ) ;
#100326 = EDGE_LOOP ( 'NONE', ( #85812, #88771, #8522, #34358 ) ) ;
#100325 = CARTESIAN_POINT ( 'NONE',  ( -2.374466145016132845, -21.38244973876172494, 11.49999999999999645 ) ) ;
#100327 = CARTESIAN_POINT ( 'NONE',  ( -75.54219529750555751, -24.63355581998385802, 0.9682620441943947664 ) ) ;
#100328 = FACE_OUTER_BOUND ( 'NONE', #64478, .T. ) ;
#100329 = ORIENTED_EDGE ( 'NONE', *, *, #34498, .T. ) ;
#100330 = CARTESIAN_POINT ( 'NONE',  ( 19.63682106917175929, 6.691539877478525966, 11.49999999999998934 ) ) ;
#100331 = EDGE_CURVE ( 'NONE', #5245, #94573, #91865, .T. ) ;
#100332 = ORIENTED_EDGE ( 'NONE', *, *, #40864, .T. ) ;
#100334 = ORIENTED_EDGE ( 'NONE', *, *, #85333, .T. ) ;
#100333 = DIRECTION ( 'NONE',  ( 0.000000000000000000, -1.000000000000000000, 0.000000000000000000 ) ) ;
#100335 = EDGE_CURVE ( 'NONE', #79151, #5695, #65970, .T. ) ;
#100336 = LINE ( 'NONE', #70930, #85836 ) ;
#100337 = EDGE_LOOP ( 'NONE', ( #79415, #27163, #72298, #18596 ) ) ;
#100338 = VERTEX_POINT ( 'NONE', #53320 ) ;
#100339 = CARTESIAN_POINT ( 'NONE',  ( 3.960454120839856706, -6.376774720514402972, 18.17119035270509997 ) ) ;
#100340 = CARTESIAN_POINT ( 'NONE',  ( -42.62371196275277896, -24.66019654487198665, 8.947790411086131712 ) ) ;
#100341 = CARTESIAN_POINT ( 'NONE',  ( -65.53713097341704952, -24.73486907724918282, 1.287355809206962354 ) ) ;
#100342 = CARTESIAN_POINT ( 'NONE',  ( -3.625624329714521643, -21.66436044012089468, 11.49999999999999645 ) ) ;
#100343 = CARTESIAN_POINT ( 'NONE',  ( -89.55462512098306149, -23.96169478059713498, 10.65365249895717703 ) ) ;
#100344 = CARTESIAN_POINT ( 'NONE',  ( 21.78986343443989071, 5.811249688775594002, -1.500000000000002220 ) ) ;
#100345 = CARTESIAN_POINT ( 'NONE',  ( -4.092705237139750984, -20.55955383578756113, -1.500000000000002220 ) ) ;
#100346 = CARTESIAN_POINT ( 'NONE',  ( -89.62287095715009855, -23.94994826722566117, -0.6494450866342719175 ) ) ;
#100347 = CARTESIAN_POINT ( 'NONE',  ( -100.6814946224345562, -25.30648942091844233, 5.043962049610569487 ) ) ;
#100348 = ORIENTED_EDGE ( 'NONE', *, *, #65199, .T. ) ;
#100349 = ORIENTED_EDGE ( 'NONE', *, *, #79456, .F. ) ;
#100350 = ORIENTED_EDGE ( 'NONE', *, *, #47245, .T. ) ;
#100351 = CARTESIAN_POINT ( 'NONE',  ( -80.62287095715005592, -23.47593901973091235, -1.443836447539004642 ) ) ;
#100352 = EDGE_CURVE ( 'NONE', #55725, #38334, #39334, .T. ) ;
#100353 = EDGE_CURVE ( 'NONE', #44715, #76875, #97389, .T. ) ;
#100354 = CARTESIAN_POINT ( 'NONE',  ( -21.26083644630951142, -3.357327265692296780, -1.500000000000002220 ) ) ;
#100355 = CARTESIAN_POINT ( 'NONE',  ( 22.81105451610979173, 8.475225279485572472, -18.46691820600746681 ) ) ;
#100356 = ORIENTED_EDGE ( 'NONE', *, *, #41367, .F. ) ;
#100357 = CARTESIAN_POINT ( 'NONE',  ( -18.69274626484788371, 9.848020819832786543, -1.500000000000002220 ) ) ;
#100358 = CARTESIAN_POINT ( 'NONE',  ( -52.62287095715005592, -24.64965695001467694, 8.947790433994185832 ) ) ;
#100359 = CARTESIAN_POINT ( 'NONE',  ( -64.52209062953060936, -23.48783264082477018, -1.443836473390096353 ) ) ;
#100361 = CARTESIAN_POINT ( 'NONE',  ( -83.64043898051973258, -23.73791477778912196, 11.05961554403170588 ) ) ;
#100360 = VECTOR ( 'NONE', #10874, 1000.000000000000000 ) ;
#100362 = DIRECTION ( 'NONE',  ( 0.000000000000000000, 0.000000000000000000, 1.000000000000000000 ) ) ;
#100363 = LINE ( 'NONE', #79047, #26008 ) ;
#100364 = CARTESIAN_POINT ( 'NONE',  ( -21.91529987491217923, -3.391794311424265018, -1.500000000000002220 ) ) ;
#100365 = CARTESIAN_POINT ( 'NONE',  ( -71.53800216701264958, -24.65952944569304961, 1.056160979905700570 ) ) ;
#100366 = ORIENTED_EDGE ( 'NONE', *, *, #22200, .F. ) ;
#100367 = CARTESIAN_POINT ( 'NONE',  ( 13.43165536947796213, 3.316774720514427344, -28.18099828186571187 ) ) ;
#100368 = CARTESIAN_POINT ( 'NONE',  ( -104.6228709571500559, -29.50250786944525672, 11.44777988621623166 ) ) ;
#100369 = CARTESIAN_POINT ( 'NONE',  ( -1.480291460309441920, -19.30061035156251847, 11.49999999999999645 ) ) ;
#100370 = ADVANCED_FACE ( 'NONE', ( #30966 ), #61932, .F. ) ;
#100371 = VECTOR ( 'NONE', #30976, 1000.000000000000000 ) ;
#100372 = ADVANCED_FACE ( 'NONE', ( #39079 ), #70033, .T. ) ;
#100373 = CARTESIAN_POINT ( 'NONE',  ( -5.891025641025637860, -5.876774720514426953, 21.75000000000000711 ) ) ;
#100374 = CIRCLE ( 'NONE', #76052, 3.060000000000000053 ) ;
#100375 = CARTESIAN_POINT ( 'NONE',  ( -12.57844902324429448, -14.85176824229388437, -1.500000000000002220 ) ) ;
#100376 = CIRCLE ( 'NONE', #3144, 2.350000000000000089 ) ;
#100377 = CARTESIAN_POINT ( 'NONE',  ( -14.55006661338671847, 15.66751491618662406, -1.500000000000002220 ) ) ;
#100378 = CARTESIAN_POINT ( 'NONE',  ( -62.59791772935989229, -23.96119346886881019, -0.6495511937832098015 ) ) ;
#100379 = PLANE ( 'NONE',  #96510 ) ;
#100380 = DIRECTION ( 'NONE',  ( 0.000000000000000000, -0.000000000000000000, -1.000000000000000000 ) ) ;
#100381 = CARTESIAN_POINT ( 'NONE',  ( -44.52287095715006160, -24.50321055353803601, 9.387540953477515160 ) ) ;
#100382 = CARTESIAN_POINT ( 'NONE',  ( 11.07647423179810531, -19.82844882884714366, -1.500000000000002220 ) ) ;
#100383 = VECTOR ( 'NONE', #68306, 1000.000000000000114 ) ;
#100384 = CARTESIAN_POINT ( 'NONE',  ( 16.36243866176394945, 2.939152317953647106E-16, -2.399999999999999911 ) ) ;
#100385 = DIRECTION ( 'NONE',  ( -0.4771587602595986910, -0.8788171126619707119, 0.000000000000000000 ) ) ;
#100386 = CARTESIAN_POINT ( 'NONE',  ( -18.79335158860655142, 6.462138572525057967, 11.49999999999999645 ) ) ;
#100387 = CARTESIAN_POINT ( 'NONE',  ( -112.5228709571500616, -23.47596703998600631, 11.44779298504228038 ) ) ;
#100388 = ADVANCED_FACE ( 'NONE', ( #41098 ), #87255, .F. ) ;
#100389 = ORIENTED_EDGE ( 'NONE', *, *, #47630, .F. ) ;
#100390 = LINE ( 'NONE', #46644, #28317 ) ;
#100391 = DIRECTION ( 'NONE',  ( -3.773278334453079618E-23, 0.9999999999976377785, 2.173523156925979975E-06 ) ) ;
#100392 = CARTESIAN_POINT ( 'NONE',  ( -68.52287095715006160, -24.65952944569304606, 1.056160979905697239 ) ) ;
#100393 = CARTESIAN_POINT ( 'NONE',  ( 12.90450488963236353, -17.39418326053592168, 11.49999999999998934 ) ) ;
#100394 = CARTESIAN_POINT ( 'NONE',  ( -32.55620429048338593, -24.66019654487198665, 8.947790411086138818 ) ) ;
#100395 = CARTESIAN_POINT ( 'NONE',  ( -1.307668758097810358, 19.38731951181482671, -1.500000000000002220 ) ) ;
#100396 = CARTESIAN_POINT ( 'NONE',  ( -82.52287095715007581, -24.66019654487199730, 8.947790411086122830 ) ) ;
#100397 = CARTESIAN_POINT ( 'NONE',  ( -61.62287095715007013, -24.50321055353805377, 9.387540953477527594 ) ) ;
#100398 = CARTESIAN_POINT ( 'NONE',  ( -19.21288746854601115, 4.878285775029977955, -1.500000000000002220 ) ) ;
#100399 = VERTEX_POINT ( 'NONE', #32982 ) ;
#100400 = CARTESIAN_POINT ( 'NONE',  ( 19.36038471569032993, -6.267470172042458820, 11.49999999999999645 ) ) ;
#100401 = CARTESIAN_POINT ( 'NONE',  ( -80.60939277392598967, -23.48783264082476308, -1.443836473390095687 ) ) ;
#100402 = ADVANCED_FACE ( 'NONE', ( #17750 ), #71547, .F. ) ;
#100403 = CARTESIAN_POINT ( 'NONE',  ( 32.84232313084928023, -4.840274619472680229, -11.71291885348849782 ) ) ;
#100404 = EDGE_CURVE ( 'NONE', #78861, #3153, #84079, .T. ) ;
#100405 = ORIENTED_EDGE ( 'NONE', *, *, #52545, .F. ) ;
#100406 = B_SPLINE_SURFACE_WITH_KNOTS ( 'NONE', 3, 3, ( 
 ( #91465, #14836, #92959, #53923 ),
 ( #23433, #54919, #622, #99562 ),
 ( #22440, #15335, #30066, #38173 ),
 ( #30570, #31568, #54416, #85351 ),
 ( #85864, #91970, #39179, #52926 ),
 ( #61541, #8240, #62531, #15835 ),
 ( #93459, #23952, #53425, #16341 ),
 ( #47307, #8742, #84353, #72576 ),
 ( #64987, #95406, #35514, #10170 ),
 ( #66489, #20262, #49254, #34513 ) ),
 .UNSPECIFIED., .F., .F., .F.,
 ( 4, 3, 3, 4 ),
 ( 4, 4 ),
 ( 0.0004766839783814420415, 0.1491231665100169468, 0.2234464077758346878, 0.2977696490416524289 ),
 ( 0.6995784914910528896, 0.7010080913662430913 ),
 .UNSPECIFIED. ) ;
#100407 = CARTESIAN_POINT ( 'NONE',  ( -102.5127707047232946, -24.35071581493543746, 9.817618358456027039 ) ) ;
#100408 = DIRECTION ( 'NONE',  ( -0.000000000000000000, 1.000000000000000000, -0.000000000000000000 ) ) ;
#100409 = CARTESIAN_POINT ( 'NONE',  ( -60.72380231474227230, -25.14083923594766645, 2.947789366383933185 ) ) ;
#100410 = CARTESIAN_POINT ( 'NONE',  ( -40.63310041807535811, -24.73531770709094957, 8.716586749053510275 ) ) ;
#100411 = CARTESIAN_POINT ( 'NONE',  ( -1.001577508147789342, -6.376774720514411854, 19.87297243748311004 ) ) ;
#100412 = CARTESIAN_POINT ( 'NONE',  ( 3.315226082619958881, 19.80964767386612380, 11.49999999999998934 ) ) ;
#100413 = ADVANCED_FACE ( 'NONE', ( #32473 ), #93867, .F. ) ;
#100414 = CARTESIAN_POINT ( 'NONE',  ( -95.58953762381672448, -24.99132157543084531, 2.256160258750496972 ) ) ;
#100415 = ORIENTED_EDGE ( 'NONE', *, *, #43960, .F. ) ;
#100416 = FACE_OUTER_BOUND ( 'NONE', #66190, .T. ) ;
#100417 = EDGE_CURVE ( 'NONE', #59375, #98210, #93793, .T. ) ;
#100418 = CARTESIAN_POINT ( 'NONE',  ( -2.380104427745746154, 22.76713797270899065, 11.49999999999999645 ) ) ;
#100419 = CARTESIAN_POINT ( 'NONE',  ( -16.51154719052397724, 15.62863258182435189, -1.500000000000002220 ) ) ;
#100420 = CARTESIAN_POINT ( 'NONE',  ( -45.52287095715005449, -24.14321612903113845, -0.2833117244521469180 ) ) ;
#100421 = NEXT_ASSEMBLY_USAGE_OCCURRENCE ( 'NAUO1', ' ', ' ', #69913, #10919, $ ) ;
#100422 = NEXT_ASSEMBLY_USAGE_OCCURRENCE ( 'NAUO2', ' ', ' ', #69913, #19046, $ ) ;
#100423 = NEXT_ASSEMBLY_USAGE_OCCURRENCE ( 'NAUO3', ' ', ' ', #69913, #94066, $ ) ;
#100424 = NEXT_ASSEMBLY_USAGE_OCCURRENCE ( 'NAUO4', ' ', ' ', #69913, #70488, $ ) ;
#100425 = NEXT_ASSEMBLY_USAGE_OCCURRENCE ( 'NAUO5', ' ', ' ', #69913, #29568, $ ) ;
#100426 = NEXT_ASSEMBLY_USAGE_OCCURRENCE ( 'NAUO6', ' ', ' ', #69913, #34522, $ ) ;
#100427 = NEXT_ASSEMBLY_USAGE_OCCURRENCE ( 'NAUO7', ' ', ' ', #69913, #57555, $ ) ;
#100428 = NEXT_ASSEMBLY_USAGE_OCCURRENCE ( 'NAUO8', ' ', ' ', #69913, #30849, $ ) ;
#100429 = NEXT_ASSEMBLY_USAGE_OCCURRENCE ( 'NAUO9', ' ', ' ', #69913, #30849, $ ) ;
#100430 = NEXT_ASSEMBLY_USAGE_OCCURRENCE ( 'NAUO10', ' ', ' ', #69913, #95340, $ ) ;
#100431 = NEXT_ASSEMBLY_USAGE_OCCURRENCE ( 'NAUO11', ' ', ' ', #69913, #14113, $ ) ;
#100432 = NEXT_ASSEMBLY_USAGE_OCCURRENCE ( 'NAUO12', ' ', ' ', #69913, #14113, $ ) ;
#100433 = NEXT_ASSEMBLY_USAGE_OCCURRENCE ( 'NAUO13', ' ', ' ', #69913, #3602, $ ) ;
#100434 = COLOUR_RGB('Deep Blue', 0.66274510, 0.83137255, 0.94901961);
#100435 = FILL_AREA_STYLE_COLOUR('',#100434);
#100436 = FILL_AREA_STYLE('',(#100435));
#100437 = SURFACE_STYLE_FILL_AREA(#100436);
#100438 = SURFACE_SIDE_STYLE('',(#100437));
#100439 = SURFACE_STYLE_USAGE(.BOTH.,#100438);
#100440 = PRESENTATION_STYLE_ASSIGNMENT((#100439));
#100441 = COLOUR_RGB('Light Blue', 0.31764706, 0.68627451, 0.89019608);
#100442 = FILL_AREA_STYLE_COLOUR('',#100441);
#100443 = FILL_AREA_STYLE('',(#100442));
#100444 = SURFACE_STYLE_FILL_AREA(#100443);
#100445 = SURFACE_SIDE_STYLE('',(#100444));
#100446 = SURFACE_STYLE_USAGE(.BOTH.,#100445);
#100447 = PRESENTATION_STYLE_ASSIGNMENT((#100446));
#100448 = COLOUR_RGB('Sky Blue', 0.40784314, 0.44705882, 0.49803922);
#100449 = FILL_AREA_STYLE_COLOUR('',#100448);
#100450 = FILL_AREA_STYLE('',(#100449));
#100451 = SURFACE_STYLE_FILL_AREA(#100450);
#100452 = SURFACE_SIDE_STYLE('',(#100451));
#100453 = SURFACE_STYLE_USAGE(.BOTH.,#100452);
#100454 = PRESENTATION_STYLE_ASSIGNMENT((#100453));
#100455 = COLOUR_RGB('Slate Gray', 0.72549020, 0.75294118, 0.79215686);
#100456 = FILL_AREA_STYLE_COLOUR('',#100455);
#100457 = FILL_AREA_STYLE('',(#100456));
#100458 = SURFACE_STYLE_FILL_AREA(#100457);
#100459 = SURFACE_SIDE_STYLE('',(#100458));
#100460 = SURFACE_STYLE_USAGE(.BOTH.,#100459);
#100461 = PRESENTATION_STYLE_ASSIGNMENT((#100460));
#100462 = COLOUR_RGB('Light Gray', 0.08235294, 0.09019608, 0.10196078);
#100463 = FILL_AREA_STYLE_COLOUR('',#100462);
#100464 = FILL_AREA_STYLE('',(#100463));
#100465 = SURFACE_STYLE_FILL_AREA(#100464);
#100466 = SURFACE_SIDE_STYLE('',(#100465));
#100467 = SURFACE_STYLE_USAGE(.BOTH.,#100466);
#100468 = PRESENTATION_STYLE_ASSIGNMENT((#100467));
#100469 = COLOUR_RGB('Black', 0.09019608, 0.27058824, 0.51372549);
#100470 = FILL_AREA_STYLE_COLOUR('',#100469);
#100471 = FILL_AREA_STYLE('',(#100470));
#100472 = SURFACE_STYLE_FILL_AREA(#100471);
#100473 = SURFACE_SIDE_STYLE('',(#100472));
#100474 = SURFACE_STYLE_USAGE(.BOTH.,#100473);
#100475 = PRESENTATION_STYLE_ASSIGNMENT((#100474));
#100476 = STYLED_ITEM('',(#100475),#42246);
#100477 = MECHANICAL_DESIGN_GEOMETRIC_PRESENTATION_REPRESENTATION('',(#100476),#19636);
#100478 = STYLED_ITEM('',(#100461),#11338);
#100479 = MECHANICAL_DESIGN_GEOMETRIC_PRESENTATION_REPRESENTATION('',(#100478),#11455);
#100480 = STYLED_ITEM('',(#100440),#8170);
#100481 = MECHANICAL_DESIGN_GEOMETRIC_PRESENTATION_REPRESENTATION('',(#100480),#27759);
#100482 = STYLED_ITEM('',(#100461),#75728);
#100483 = MECHANICAL_DESIGN_GEOMETRIC_PRESENTATION_REPRESENTATION('',(#100482),#35871);
#100484 = STYLED_ITEM('',(#100447),#43720);
#100485 = MECHANICAL_DESIGN_GEOMETRIC_PRESENTATION_REPRESENTATION('',(#100484),#45585);
#100486 = STYLED_ITEM('',(#100468),#29565);
#100487 = MECHANICAL_DESIGN_GEOMETRIC_PRESENTATION_REPRESENTATION('',(#100486),#69909);
#100488 = STYLED_ITEM('',(#100447),#8332);
#100489 = MECHANICAL_DESIGN_GEOMETRIC_PRESENTATION_REPRESENTATION('',(#100488),#48843);
#100490 = STYLED_ITEM('',(#100440),#42411);
#100491 = MECHANICAL_DESIGN_GEOMETRIC_PRESENTATION_REPRESENTATION('',(#100490),#16366);
#100492 = STYLED_ITEM('',(#100468),#76408);
#100493 = MECHANICAL_DESIGN_GEOMETRIC_PRESENTATION_REPRESENTATION('',(#100492),#82851);
#100494 = STYLED_ITEM('',(#100454),#44893);
#100495 = MECHANICAL_DESIGN_GEOMETRIC_PRESENTATION_REPRESENTATION('',(#100494),#61811);
#100496 = STYLED_ITEM('',(#100454),#10173);
#100497 = MECHANICAL_DESIGN_GEOMETRIC_PRESENTATION_REPRESENTATION('',(#100496),#14765);
ENDSEC;
END-ISO-10303-21;
